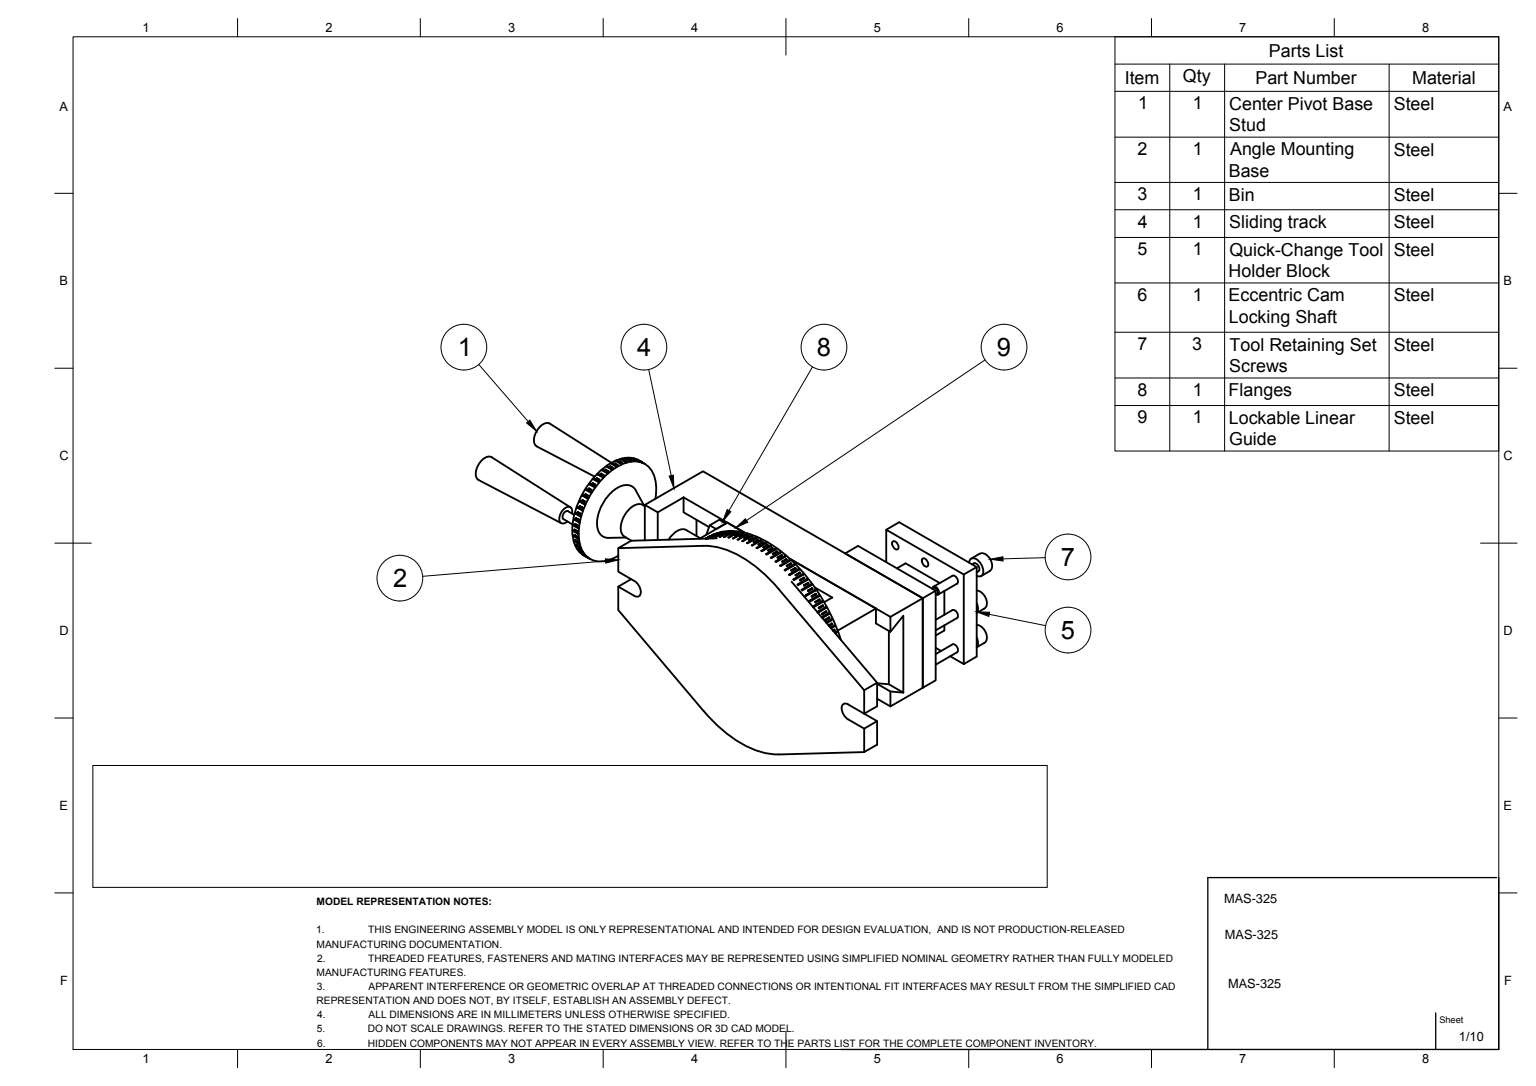
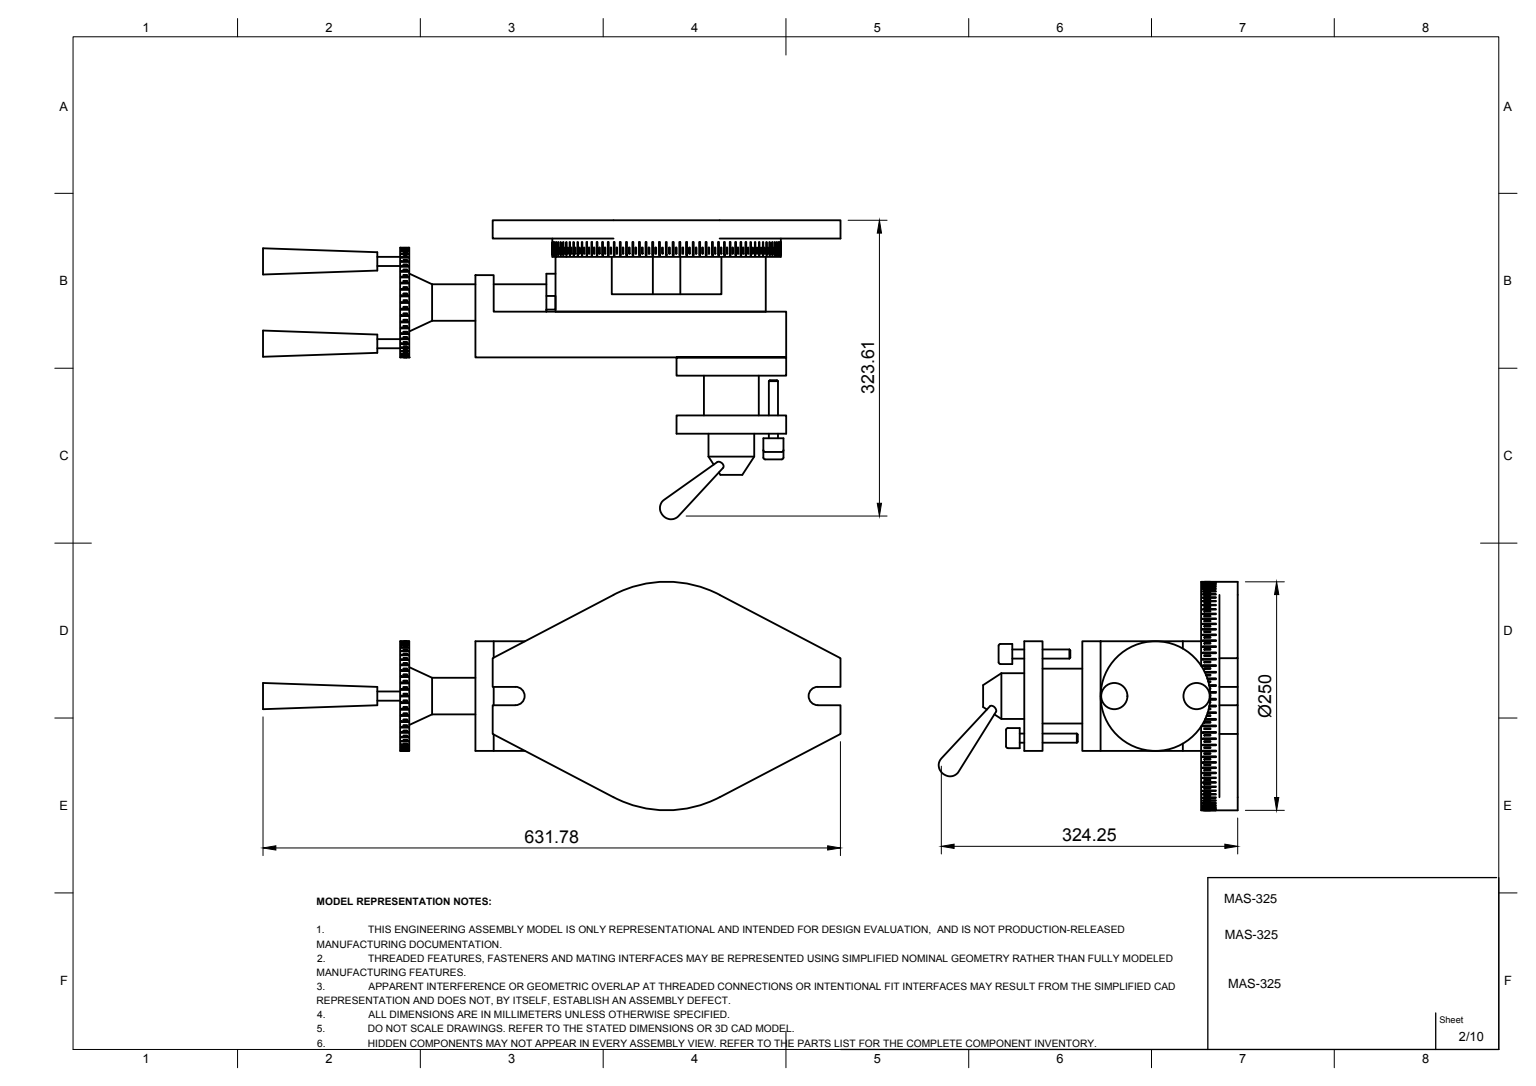
ISO-10303-21;
HEADER;
FILE_DESCRIPTION (('STEP AP214'),
    '1' );
FILE_NAME ('MAS-325',
    '2026-10-08T01:23:29',
    ( '' ),
    ( '' ),
    'SwSTEP 2.0',
    'SolidWorks 2025',
    '' );
FILE_SCHEMA (( 'AUTOMOTIVE_DESIGN' ));
ENDSEC;

DATA;
#1 = PLANE ( 'NONE',  #17713 ) ;
#2 = FACE_OUTER_BOUND ( 'NONE', #26944, .T. ) ;
#3 = VERTEX_POINT ( 'NONE', #17850 ) ;
#4 = VERTEX_POINT ( 'NONE', #2063 ) ;
#5 = EDGE_LOOP ( 'NONE', ( #45365, #39449, #49591, #6514 ) ) ;
#6 = EDGE_CURVE ( 'NONE', #30158, #26369, #45209, .T. ) ;
#7 = DIRECTION ( 'NONE',  ( 1.000000000000000000, -0.000000000000000000, -0.000000000000000000 ) ) ;
#8 = DIRECTION ( 'NONE',  ( 0.000000000000000000, 0.000000000000000000, -1.000000000000000000 ) ) ;
#9 = FACE_OUTER_BOUND ( 'NONE', #31225, .T. ) ;
#10 = ORIENTED_EDGE ( 'NONE', *, *, #44040, .F. ) ;
#11 = CARTESIAN_POINT ( 'NONE',  ( 2.729299751253404072, 51.29764658765966345, -20.73231253916988237 ) ) ;
#12 = ORIENTED_EDGE ( 'NONE', *, *, #51700, .T. ) ;
#13 = ORIENTED_EDGE ( 'NONE', *, *, #43268, .F. ) ;
#14 = ORIENTED_EDGE ( 'NONE', *, *, #20809, .T. ) ;
#15 = LINE ( 'NONE', #16057, #4072 ) ;
#16 = EDGE_CURVE ( 'NONE', #34125, #29247, #18107, .T. ) ;
#17 = ADVANCED_FACE ( 'NONE', ( #34134 ), #14181, .T. ) ;
#18 = ORIENTED_EDGE ( 'NONE', *, *, #15943, .T. ) ;
#19 = AXIS2_PLACEMENT_3D ( 'NONE', #21420, #9597, #9087 ) ;
#20 = AXIS2_PLACEMENT_3D ( 'NONE', #37352, #1353, #33432 ) ;
#21 = EDGE_CURVE ( 'NONE', #1891, #35017, #9977, .T. ) ;
#22 = CARTESIAN_POINT ( 'NONE',  ( -159.8192355313504720, -177.1207230881787780, -56.81883646197830018 ) ) ;
#23 = DIRECTION ( 'NONE',  ( -0.000000000000000000, 1.000000000000000000, -0.000000000000000000 ) ) ;
#26 = ORIENTED_EDGE ( 'NONE', *, *, #11216, .F. ) ;
#25 = CARTESIAN_POINT ( 'NONE',  ( -336.3521761649654422, -170.5607375887735770, 35.68215131113770155 ) ) ;
#24 = CARTESIAN_POINT ( 'NONE',  ( -0.3054481938615447034, -177.1207230881787780, 115.3442529744090592 ) ) ;
#27 = DIRECTION ( 'NONE',  ( -0.000000000000000000, 1.000000000000000000, -0.000000000000000000 ) ) ;
#28 = EDGE_LOOP ( 'NONE', ( #8074, #9559, #4118, #19918 ) ) ;
#29 = DIRECTION ( 'NONE',  ( 0.000000000000000000, -0.3546048870425363986, -0.9350162426854146114 ) ) ;
#30 = ORIENTED_EDGE ( 'NONE', *, *, #16889, .F. ) ;
#31 = CARTESIAN_POINT ( 'NONE',  ( -339.1964088526558498, -131.1080185721124849, 58.50955523165764305 ) ) ;
#32 = LINE ( 'NONE', #15292, #22958 ) ;
#34 = CARTESIAN_POINT ( 'NONE',  ( 15.29189835570547551, -175.3837268820161057, 106.3450133598704213 ) ) ;
#33 = CARTESIAN_POINT ( 'NONE',  ( -56.05401443572774411, -175.3837268820161057, 124.7702732086912931 ) ) ;
#35 = VERTEX_POINT ( 'NONE', #9196 ) ;
#36 = DIRECTION ( 'NONE',  ( -1.000000000000000000, -0.000000000000000000, -0.000000000000000000 ) ) ;
#37 = FACE_OUTER_BOUND ( 'NONE', #25266, .T. ) ;
#39 = AXIS2_PLACEMENT_3D ( 'NONE', #35953, #36729, #8094 ) ;
#38 =( NAMED_UNIT ( * ) PLANE_ANGLE_UNIT ( ) SI_UNIT ( $, .RADIAN. ) );
#40 = ORIENTED_EDGE ( 'NONE', *, *, #10845, .T. ) ;
#41 = EDGE_CURVE ( 'NONE', #38866, #36143, #5787, .T. ) ;
#42 = DIRECTION ( 'NONE',  ( -0.000000000000000000, 1.000000000000000000, -0.000000000000000000 ) ) ;
#43 = LINE ( 'NONE', #8442, #5592 ) ;
#44 = DIRECTION ( 'NONE',  ( -0.8455960035018311727, 0.000000000000000000, 0.5338233779647826305 ) ) ;
#45 = ORIENTED_EDGE ( 'NONE', *, *, #35189, .T. ) ;
#46 = CARTESIAN_POINT ( 'NONE',  ( 63.31225588004632243, -183.6283474603465606, 55.92572546981597981 ) ) ;
#47 = FACE_OUTER_BOUND ( 'NONE', #8464, .T. ) ;
#48 = EDGE_CURVE ( 'NONE', #19235, #10210, #19545, .T. ) ;
#49 = ORIENTED_EDGE ( 'NONE', *, *, #34843, .T. ) ;
#50 = DIRECTION ( 'NONE',  ( -0.4031234292879665171, 0.000000000000000000, -0.9151456172430210145 ) ) ;
#51 = ORIENTED_EDGE ( 'NONE', *, *, #6223, .F. ) ;
#52 = DIRECTION ( 'NONE',  ( 0.000000000000000000, 1.341519488088730767E-14, -1.000000000000000000 ) ) ;
#53 = CARTESIAN_POINT ( 'NONE',  ( -47.55243714407702527, -193.5000000000000000, 0.3758275821142491591 ) ) ;
#54 = AXIS2_PLACEMENT_3D ( 'NONE', #38179, #2187, #21657 ) ;
#55 = CARTESIAN_POINT ( 'NONE',  ( -332.3517673607765914, -139.2044816956407089, -56.89493493766761389 ) ) ;
#56 = CARTESIAN_POINT ( 'NONE',  ( 74.95461934957533856, -175.3837268820161057, -11.83705339977243121 ) ) ;
#57 = PLANE ( 'NONE',  #3915 ) ;
#58 = CIRCLE ( 'NONE', #10119, 125.0000000000000000 ) ;
#59 = CARTESIAN_POINT ( 'NONE',  ( -336.3521761649654422, -123.5000000000000284, 0.000000000000000000 ) ) ;
#60 = CARTESIAN_POINT ( 'NONE',  ( -330.4913330509368166, -178.8432607619606358, 20.45418021416736565 ) ) ;
#61 = LINE ( 'NONE', #8461, #49088 ) ;
#63 = ORIENTED_EDGE ( 'NONE', *, *, #44474, .F. ) ;
#62 = CARTESIAN_POINT ( 'NONE',  ( -135.4449840867448813, -193.5000000000000000, -88.39086586114740385 ) ) ;
#64 = ORIENTED_EDGE ( 'NONE', *, *, #9737, .T. ) ;
#65 = CARTESIAN_POINT ( 'NONE',  ( -339.1964088526558498, -175.5095439275173135, 27.86139516340941213 ) ) ;
#66 = CARTESIAN_POINT ( 'NONE',  ( -332.3517673607765914, -91.61526299123897843, -50.82679948493848343 ) ) ;
#67 = ORIENTED_EDGE ( 'NONE', *, *, #21766, .T. ) ;
#68 = ORIENTED_EDGE ( 'NONE', *, *, #41329, .T. ) ;
#69 = VECTOR ( 'NONE', #22524, 1000.000000000000000 ) ;
#70 = ORIENTED_EDGE ( 'NONE', *, *, #36153, .T. ) ;
#71 = CARTESIAN_POINT ( 'NONE',  ( 74.13662511985246795, -189.7472609257535510, 18.47640724094593523 ) ) ;
#72 = DIRECTION ( 'NONE',  ( 0.000000000000000000, 0.000000000000000000, 1.000000000000000000 ) ) ;
#73 = EDGE_CURVE ( 'NONE', #1427, #18230, #29600, .T. ) ;
#74 = CARTESIAN_POINT ( 'NONE',  ( -52.47502265695594303, -183.6283474603465606, -124.9361149384469627 ) ) ;
#75 = DIRECTION ( 'NONE',  ( 0.000000000000000000, -0.000000000000000000, 1.000000000000000000 ) ) ;
#76 = VERTEX_POINT ( 'NONE', #10211 ) ;
#77 = VERTEX_POINT ( 'NONE', #49406 ) ;
#78 = ORIENTED_EDGE ( 'NONE', *, *, #31301, .F. ) ;
#79 = DIRECTION ( 'NONE',  ( -0.000000000000000000, 1.000000000000000000, -0.000000000000000000 ) ) ;
#80 = DIRECTION ( 'NONE',  ( 0.6749830015182038956, 0.000000000000000000, 0.7378332790417333475 ) ) ;
#81 = CARTESIAN_POINT ( 'NONE',  ( -330.4913330509368166, -183.4979166304964622, -0.4999999999999551470 ) ) ;
#82 = LINE ( 'NONE', #16386, #13659 ) ;
#83 = FACE_OUTER_BOUND ( 'NONE', #49301, .T. ) ;
#84 = ORIENTED_EDGE ( 'NONE', *, *, #48754, .F. ) ;
#85 = DIRECTION ( 'NONE',  ( -0.000000000000000000, 1.000000000000000000, -0.000000000000000000 ) ) ;
#86 = AXIS2_PLACEMENT_3D ( 'NONE', #8984, #303, #32633 ) ;
#87 = LINE ( 'NONE', #8748, #33300 ) ;
#88 = CARTESIAN_POINT ( 'NONE',  ( -29.73468717939733708, -193.5000000000000000, 123.5865930638410930 ) ) ;
#89 = DIRECTION ( 'NONE',  ( -0.2059786187411094538, 0.000000000000000000, 0.9785564922995017012 ) ) ;
#90 = ORIENTED_EDGE ( 'NONE', *, *, #2858, .T. ) ;
#91 = ORIENTED_EDGE ( 'NONE', *, *, #37914, .F. ) ;
#92 = ORIENTED_EDGE ( 'NONE', *, *, #9964, .T. ) ;
#93 = CARTESIAN_POINT ( 'NONE',  ( -171.9740864388383557, -189.7472609257535510, -11.18012358327903577 ) ) ;
#94 = DIRECTION ( 'NONE',  ( -0.8757349421956412971, 0.000000000000000000, 0.4827922027307366970 ) ) ;
#95 = ORIENTED_EDGE ( 'NONE', *, *, #42836, .F. ) ;
#96 = EDGE_CURVE ( 'NONE', #8568, #51994, #49908, .T. ) ;
#97 = LINE ( 'NONE', #16919, #528 ) ;
#98 = DIRECTION ( 'NONE',  ( -0.9982437317643214625, 0.000000000000000000, -0.05924062789371441901 ) ) ;
#99 = CARTESIAN_POINT ( 'NONE',  ( 141.7825277784304205, -193.5000000000000000, -9.999999999999987566 ) ) ;
#100 = ORIENTED_EDGE ( 'NONE', *, *, #32040, .F. ) ;
#101 = LINE ( 'NONE', #40291, #9133 ) ;
#102 = ORIENTED_EDGE ( 'NONE', *, *, #46111, .F. ) ;
#103 = CARTESIAN_POINT ( 'NONE',  ( -336.3521761649654422, -123.5000000000000284, 0.000000000000000000 ) ) ;
#104 = ORIENTED_EDGE ( 'NONE', *, *, #44978, .T. ) ;
#105 = LINE ( 'NONE', #39778, #22073 ) ;
#106 = FACE_BOUND ( 'NONE', #42826, .T. ) ;
#107 = VECTOR ( 'NONE', #36864, 1000.000000000000000 ) ;
#108 = DIRECTION ( 'NONE',  ( -0.1768902751225802927, 0.000000000000000000, 0.9842305779475953864 ) ) ;
#109 = ORIENTED_EDGE ( 'NONE', *, *, #36766, .T. ) ;
#110 = DIRECTION ( 'NONE',  ( 1.000000000000000000, -0.000000000000000000, -0.000000000000000000 ) ) ;
#111 = DIRECTION ( 'NONE',  ( 0.9785564922995032555, 0.000000000000000000, 0.2059786187411021818 ) ) ;
#112 = DIRECTION ( 'NONE',  ( 0.000000000000000000, -1.000000000000000000, 0.000000000000000000 ) ) ;
#113 = EDGE_CURVE ( 'NONE', #39629, #40896, #21795, .T. ) ;
#114 = CARTESIAN_POINT ( 'NONE',  ( -339.1964088526558498, -122.9999999999993747, 59.00000000000002132 ) ) ;
#115 = EDGE_LOOP ( 'NONE', ( #6615, #26573, #34341, #46200 ) ) ;
#116 = CARTESIAN_POINT ( 'NONE',  ( -162.3451783319732726, -183.6283474603465606, 51.57055649762781968 ) ) ;
#117 = VERTEX_POINT ( 'NONE', #22299 ) ;
#118 = EDGE_LOOP ( 'NONE', ( #5505, #7567, #35660, #29019 ) ) ;
#119 = CARTESIAN_POINT ( 'NONE',  ( -47.97059563285962724, -189.7472609257535510, -0.8610436117673480050 ) ) ;
#121 = VERTEX_POINT ( 'NONE', #29930 ) ;
#120 = DIRECTION ( 'NONE',  ( 0.000000000000000000, 0.000000000000000000, -1.000000000000000000 ) ) ;
#122 = VECTOR ( 'NONE', #5953, 1000.000000000000000 ) ;
#123 = ORIENTED_EDGE ( 'NONE', *, *, #8914, .F. ) ;
#124 = CARTESIAN_POINT ( 'NONE',  ( 76.04209377433248562, -193.5000000000000000, -10.93003379476866677 ) ) ;
#125 = CIRCLE ( 'NONE', #14436, 125.0000000000000000 ) ;
#126 = AXIS2_PLACEMENT_3D ( 'NONE', #20035, #19509, #35530 ) ;
#127 = EDGE_CURVE ( 'NONE', #48981, #10059, #6022, .T. ) ;
#128 = CARTESIAN_POINT ( 'NONE',  ( 23.33927677392131628, -183.6283474603465606, -102.3089288139528747 ) ) ;
#129 = EDGE_LOOP ( 'NONE', ( #1022, #18617, #38243, #43508 ) ) ;
#130 = FACE_OUTER_BOUND ( 'NONE', #50584, .T. ) ;
#131 = FACE_OUTER_BOUND ( 'NONE', #2320, .T. ) ;
#132 = EDGE_LOOP ( 'NONE', ( #26426, #7526, #45933, #33902, #50296, #18073, #41197, #48921 ) ) ;
#133 = LINE ( 'NONE', #35615, #5709 ) ;
#134 = DIRECTION ( 'NONE',  ( 0.000000000000000000, 0.000000000000000000, -1.000000000000000000 ) ) ;
#135 = ADVANCED_FACE ( 'NONE', ( #33613 ), #26232, .F. ) ;
#136 = LINE ( 'NONE', #12733, #6804 ) ;
#137 = CARTESIAN_POINT ( 'NONE',  ( -180.0000000000000568, -123.5000000000000284, 6.938893903907228378E-15 ) ) ;
#138 = VERTEX_POINT ( 'NONE', #51213 ) ;
#139 = EDGE_LOOP ( 'NONE', ( #49981, #10287, #23201, #19361 ) ) ;
#140 = EDGE_CURVE ( 'NONE', #35696, #40857, #2842, .T. ) ;
#141 = EDGE_LOOP ( 'NONE', ( #33716, #13532, #31496, #14076 ) ) ;
#142 = FACE_OUTER_BOUND ( 'NONE', #28523, .T. ) ;
#143 = FACE_OUTER_BOUND ( 'NONE', #34738, .T. ) ;
#144 = ADVANCED_FACE ( 'NONE', ( #30434 ), #14678, .T. ) ;
#145 = AXIS2_PLACEMENT_3D ( 'NONE', #44882, #32531, #8363 ) ;
#146 = DIRECTION ( 'NONE',  ( 0.000000000000000000, 0.000000000000000000, 1.000000000000000000 ) ) ;
#147 = FACE_BOUND ( 'NONE', #3566, .T. ) ;
#148 = CARTESIAN_POINT ( 'NONE',  ( -49.42645310536303782, -193.5000000000000000, -0.3202698538628417357 ) ) ;
#149 = EDGE_LOOP ( 'NONE', ( #37158, #34749, #12622, #8315 ) ) ;
#150 = VERTEX_POINT ( 'NONE', #38840 ) ;
#152 = ORIENTED_EDGE ( 'NONE', *, *, #45435, .F. ) ;
#151 = DIRECTION ( 'NONE',  ( 0.000000000000000000, -0.000000000000000000, 1.000000000000000000 ) ) ;
#153 = VERTEX_POINT ( 'NONE', #46748 ) ;
#154 = CARTESIAN_POINT ( 'NONE',  ( -332.3517673607765914, -153.2494431741581025, -51.01861988938816950 ) ) ;
#155 = EDGE_CURVE ( 'NONE', #5943, #22832, #22063, .T. ) ;
#156 = DIRECTION ( 'NONE',  ( -1.000000000000000000, 0.000000000000000000, 0.000000000000000000 ) ) ;
#157 = VECTOR ( 'NONE', #9488, 1000.000000000000000 ) ;
#158 = DIRECTION ( 'NONE',  ( 0.000000000000000000, 0.000000000000000000, 1.000000000000000000 ) ) ;
#159 = CARTESIAN_POINT ( 'NONE',  ( -84.53143451966467126, -175.3837268820161057, -118.6432945265036807 ) ) ;
#160 = ORIENTED_EDGE ( 'NONE', *, *, #6029, .T. ) ;
#161 = LINE ( 'NONE', #28016, #26684 ) ;
#162 = AXIS2_PLACEMENT_3D ( 'NONE', #7997, #20089, #36113 ) ;
#163 = ORIENTED_EDGE ( 'NONE', *, *, #20136, .T. ) ;
#164 = AXIS2_PLACEMENT_3D ( 'NONE', #24435, #20760, #36510 ) ;
#165 = ORIENTED_EDGE ( 'NONE', *, *, #4140, .T. ) ;
#166 = DIRECTION ( 'NONE',  ( 0.000000000000000000, -0.000000000000000000, 1.000000000000000000 ) ) ;
#167 = CARTESIAN_POINT ( 'NONE',  ( -139.0630283577175987, -193.5000000000000000, -86.13684908212448477 ) ) ;
#168 = CARTESIAN_POINT ( 'NONE',  ( -15.24927435600541692, -177.1207230881787780, 120.5021863277719234 ) ) ;
#169 = CARTESIAN_POINT ( 'NONE',  ( -336.3521761649654422, -161.4024510877913485, 45.24454186338643780 ) ) ;
#170 = CARTESIAN_POINT ( 'NONE',  ( -144.0067397530739299, -183.6283474603465606, -80.61932246194588458 ) ) ;
#171 = CARTESIAN_POINT ( 'NONE',  ( -41.24387117724851493, -189.7472609257535510, 124.7904286264581231 ) ) ;
#172 = VERTEX_POINT ( 'NONE', #26760 ) ;
#173 = DIRECTION ( 'NONE',  ( -0.8896570909947467687, 0.000000000000000000, -0.4566292373937140270 ) ) ;
#174 = CARTESIAN_POINT ( 'NONE',  ( -134.9734323446613473, -175.3837268820161057, 88.85232316304892208 ) ) ;
#175 = CIRCLE ( 'NONE', #31206, 125.0000000000000000 ) ;
#176 = FACE_BOUND ( 'NONE', #45465, .T. ) ;
#177 = VERTEX_POINT ( 'NONE', #42529 ) ;
#178 = AXIS2_PLACEMENT_3D ( 'NONE', #15666, #4339, #31680 ) ;
#179 = CIRCLE ( 'NONE', #49719, 4.000000000000003553 ) ;
#180 = DIRECTION ( 'NONE',  ( -0.000000000000000000, 1.000000000000000000, -0.000000000000000000 ) ) ;
#181 = FACE_OUTER_BOUND ( 'NONE', #6191, .T. ) ;
#182 = EDGE_CURVE ( 'NONE', #39742, #38924, #15463, .T. ) ;
#183 = ORIENTED_EDGE ( 'NONE', *, *, #47786, .F. ) ;
#184 = ADVANCED_FACE ( 'NONE', ( #15201 ), #27530, .F. ) ;
#185 = DIRECTION ( 'NONE',  ( 0.4827922027307366970, 0.000000000000000000, 0.8757349421956412971 ) ) ;
#186 = VERTEX_POINT ( 'NONE', #51463 ) ;
#187 = CARTESIAN_POINT ( 'NONE',  ( -148.0127667507368585, -183.6283474603465606, -75.61781872352626976 ) ) ;
#188 = CARTESIAN_POINT ( 'NONE',  ( -48.47912675150885065, -193.5000000000000000, 6.938893903907228378E-15 ) ) ;
#190 = EDGE_LOOP ( 'NONE', ( #41506, #8467, #35219, #32996 ) ) ;
#189 = DIRECTION ( 'NONE',  ( 0.000000000000000000, 0.000000000000000000, 1.000000000000000000 ) ) ;
#191 = AXIS2_PLACEMENT_3D ( 'NONE', #6779, #42505, #19123 ) ;
#192 = ADVANCED_FACE ( 'NONE', ( #46484 ), #50954, .F. ) ;
#193 = FACE_OUTER_BOUND ( 'NONE', #27346, .T. ) ;
#194 = VERTEX_POINT ( 'NONE', #14955 ) ;
#195 = EDGE_CURVE ( 'NONE', #34486, #40282, #15361, .T. ) ;
#196 = AXIS2_PLACEMENT_3D ( 'NONE', #12070, #3180, #43634 ) ;
#197 = ORIENTED_EDGE ( 'NONE', *, *, #15389, .T. ) ;
#198 = ADVANCED_FACE ( 'NONE', ( #19392 ), #26495, .F. ) ;
#199 = EDGE_LOOP ( 'NONE', ( #48171, #38497, #32246, #32492 ) ) ;
#200 = DIRECTION ( 'NONE',  ( 0.000000000000000000, 0.2393156642875615969, 0.9709418174260511236 ) ) ;
#201 = CARTESIAN_POINT ( 'NONE',  ( -339.1964088526558498, -180.9052250602809977, -13.63415328425247885 ) ) ;
#202 = EDGE_CURVE ( 'NONE', #8838, #28521, #30963, .T. ) ;
#203 = AXIS2_PLACEMENT_3D ( 'NONE', #1568, #37299, #37818 ) ;
#204 = AXIS2_PLACEMENT_3D ( 'NONE', #4568, #29258, #44511 ) ;
#205 = CARTESIAN_POINT ( 'NONE',  ( -157.8637630444124795, -175.3837268820161057, -60.49794494914009135 ) ) ;
#206 = CARTESIAN_POINT ( 'NONE',  ( -332.3517673607765914, -86.34605966037949543, -45.90766452162698386 ) ) ;
#207 = ORIENTED_EDGE ( 'NONE', *, *, #866, .T. ) ;
#210 = VERTEX_POINT ( 'NONE', #34890 ) ;
#209 = DIRECTION ( 'NONE',  ( 0.000000000000000000, 0.000000000000000000, 1.000000000000000000 ) ) ;
#208 = DIRECTION ( 'NONE',  ( 0.000000000000000000, 0.000000000000000000, 1.000000000000000000 ) ) ;
#211 = AXIS2_PLACEMENT_3D ( 'NONE', #44344, #36428, #28543 ) ;
#212 = AXIS2_PLACEMENT_3D ( 'NONE', #15523, #6858, #2909 ) ;
#213 = EDGE_LOOP ( 'NONE', ( #16091, #33158, #8108, #2239 ) ) ;
#214 = CARTESIAN_POINT ( 'NONE',  ( -339.1964088526558498, -157.4273119900853146, -48.27201571435997352 ) ) ;
#215 = ORIENTED_EDGE ( 'NONE', *, *, #9578, .T. ) ;
#216 = CARTESIAN_POINT ( 'NONE',  ( -339.1964088526558498, -83.33976666098951114, 44.57752413667933666 ) ) ;
#217 = ORIENTED_EDGE ( 'NONE', *, *, #6337, .T. ) ;
#218 = VECTOR ( 'NONE', #39857, 1000.000000000000227 ) ;
#219 = DIRECTION ( 'NONE',  ( 0.000000000000000000, 1.000000000000000000, 0.000000000000000000 ) ) ;
#220 = ORIENTED_EDGE ( 'NONE', *, *, #16410, .F. ) ;
#222 = DIRECTION ( 'NONE',  ( -0.000000000000000000, 0.2393156642875685636, 0.9709418174260492362 ) ) ;
#221 = CARTESIAN_POINT ( 'NONE',  ( 0.000000000000000000, 103.6102204319011832, -100.2584055548201292 ) ) ;
#223 = ORIENTED_EDGE ( 'NONE', *, *, #649, .T. ) ;
#224 = ORIENTED_EDGE ( 'NONE', *, *, #48940, .F. ) ;
#225 = FACE_OUTER_BOUND ( 'NONE', #49522, .T. ) ;
#226 = DIRECTION ( 'NONE',  ( -0.9890401873221633666, 0.000000000000000000, -0.1476465640024850756 ) ) ;
#227 = FACE_OUTER_BOUND ( 'NONE', #2223, .T. ) ;
#228 = DIRECTION ( 'NONE',  ( 0.000000000000000000, 0.000000000000000000, 1.000000000000000000 ) ) ;
#229 = FACE_OUTER_BOUND ( 'NONE', #4833, .T. ) ;
#230 = CIRCLE ( 'NONE', #6149, 125.0000000000000000 ) ;
#231 = DIRECTION ( 'NONE',  ( -0.000000000000000000, 1.000000000000000000, -0.000000000000000000 ) ) ;
#232 = VERTEX_POINT ( 'NONE', #18624 ) ;
#233 = FACE_OUTER_BOUND ( 'NONE', #34259, .T. ) ;
#234 = CARTESIAN_POINT ( 'NONE',  ( -47.82630463331833681, -177.1207230881787780, 0.7575112421616305713 ) ) ;
#235 = AXIS2_PLACEMENT_3D ( 'NONE', #29797, #45849, #41895 ) ;
#236 = ADVANCED_FACE ( 'NONE', ( #38589 ), #47005, .T. ) ;
#237 = CARTESIAN_POINT ( 'NONE',  ( -180.0000000000000568, -115.7896721143442278, 18.45401972188388839 ) ) ;
#238 = ORIENTED_EDGE ( 'NONE', *, *, #26470, .F. ) ;
#239 = CARTESIAN_POINT ( 'NONE',  ( 74.49773146996551532, -183.6283474603465606, -22.39848972532281834 ) ) ;
#240 = EDGE_CURVE ( 'NONE', #16530, #9197, #11238, .T. ) ;
#241 = FACE_OUTER_BOUND ( 'NONE', #10500, .T. ) ;
#242 = CYLINDRICAL_SURFACE ( 'NONE', #15746, 20.00000000000001066 ) ;
#243 = EDGE_CURVE ( 'NONE', #48355, #27011, #50682, .T. ) ;
#244 = ORIENTED_EDGE ( 'NONE', *, *, #45271, .T. ) ;
#245 = EDGE_CURVE ( 'NONE', #35901, #35187, #7056, .T. ) ;
#246 = VERTEX_POINT ( 'NONE', #50438 ) ;
#247 = CIRCLE ( 'NONE', #6976, 125.0000000000000000 ) ;
#248 = EDGE_LOOP ( 'NONE', ( #15059, #26707, #42311, #35212 ) ) ;
#249 = CIRCLE ( 'NONE', #45592, 125.0000000000000000 ) ;
#250 = EDGE_CURVE ( 'NONE', #5889, #26611, #27078, .T. ) ;
#251 = LINE ( 'NONE', #40705, #46952 ) ;
#252 = AXIS2_PLACEMENT_3D ( 'NONE', #33154, #25277, #24755 ) ;
#253 = ADVANCED_FACE ( 'NONE', ( #3105 ), #7314, .F. ) ;
#254 = CARTESIAN_POINT ( 'NONE',  ( 1.959434878635765131E-15, -63.50000000000000000, 16.00000000000000000 ) ) ;
#255 = CARTESIAN_POINT ( 'NONE',  ( -157.8637630444124795, -175.3837268820161057, -60.49794494914009846 ) ) ;
#256 = DIRECTION ( 'NONE',  ( -0.000000000000000000, 0.8229838658936556861, -0.5680647467311569221 ) ) ;
#257 = EDGE_LOOP ( 'NONE', ( #21171, #20586, #46600, #11240 ) ) ;
#258 = AXIS2_PLACEMENT_3D ( 'NONE', #32515, #48563, #24621 ) ;
#259 = EDGE_CURVE ( 'NONE', #47910, #27371, #721, .T. ) ;
#260 = CARTESIAN_POINT ( 'NONE',  ( -332.3517673607765914, -133.2247606357419443, -58.25253621232173629 ) ) ;
#261 = ORIENTED_EDGE ( 'NONE', *, *, #51004, .T. ) ;
#262 = EDGE_CURVE ( 'NONE', #7509, #26454, #12272, .T. ) ;
#263 = ORIENTED_EDGE ( 'NONE', *, *, #26885, .T. ) ;
#264 = EDGE_CURVE ( 'NONE', #15715, #30086, #23588, .T. ) ;
#265 = VERTEX_POINT ( 'NONE', #44078 ) ;
#266 = CARTESIAN_POINT ( 'NONE',  ( -111.6834028793037987, -175.3837268820161057, 106.6827995071088253 ) ) ;
#267 = VECTOR ( 'NONE', #9756, 1000.000000000000000 ) ;
#268 = EDGE_CURVE ( 'NONE', #19322, #4539, #40375, .T. ) ;
#269 = ORIENTED_EDGE ( 'NONE', *, *, #12211, .F. ) ;
#270 = ADVANCED_FACE ( 'NONE', ( #39602 ), #440, .T. ) ;
#271 = AXIS2_PLACEMENT_3D ( 'NONE', #37551, #38049, #18093 ) ;
#272 = CARTESIAN_POINT ( 'NONE',  ( -102.9981419485577732, -193.5000000000000000, -111.3726929437936377 ) ) ;
#273 = LINE ( 'NONE', #29176, #44951 ) ;
#276 = ORIENTED_EDGE ( 'NONE', *, *, #30764, .F. ) ;
#275 = DIRECTION ( 'NONE',  ( 0.000000000000000000, 0.000000000000000000, -1.000000000000000000 ) ) ;
#274 = DIRECTION ( 'NONE',  ( -0.6300878435817094392, 0.000000000000000000, -0.7765238627180437447 ) ) ;
#277 = CARTESIAN_POINT ( 'NONE',  ( -108.4791267515088435, -173.5000000000000284, 60.00000000000002132 ) ) ;
#278 = ORIENTED_EDGE ( 'NONE', *, *, #14380, .F. ) ;
#279 = LINE ( 'NONE', #11844, #1238 ) ;
#280 = ORIENTED_EDGE ( 'NONE', *, *, #40635, .T. ) ;
#281 = DIRECTION ( 'NONE',  ( 0.000000000000000000, 0.000000000000000000, 1.000000000000000000 ) ) ;
#282 = CARTESIAN_POINT ( 'NONE',  ( -117.6201219941651601, -193.5000000000000000, 104.1370384486469902 ) ) ;
#284 = LINE ( 'NONE', #32615, #29005 ) ;
#283 = DIRECTION ( 'NONE',  ( 0.9785564922995060311, 0.000000000000000000, -0.2059786187410889424 ) ) ;
#285 = VECTOR ( 'NONE', #4558, 999.9999999999998863 ) ;
#286 = EDGE_CURVE ( 'NONE', #41564, #12706, #20162, .T. ) ;
#287 = EDGE_LOOP ( 'NONE', ( #13570, #29381, #45686, #19106 ) ) ;
#288 = CARTESIAN_POINT ( 'NONE',  ( -332.3517673607765914, -139.4384828369889249, -57.84431488793872944 ) ) ;
#289 = VECTOR ( 'NONE', #42767, 1000.000000000000000 ) ;
#290 = LINE ( 'NONE', #41018, #22829 ) ;
#291 =( NAMED_UNIT ( * ) SI_UNIT ( $, .STERADIAN. ) SOLID_ANGLE_UNIT ( ) );
#292 = ORIENTED_EDGE ( 'NONE', *, *, #4293, .T. ) ;
#293 = DIRECTION ( 'NONE',  ( -0.7378332790417285736, 0.000000000000000000, 0.6749830015182091136 ) ) ;
#294 = DIRECTION ( 'NONE',  ( 0.000000000000000000, 1.000000000000000000, 0.000000000000000000 ) ) ;
#295 = DIRECTION ( 'NONE',  ( -0.5315839928299663786, 0.000000000000000000, 0.8470055835512245723 ) ) ;
#296 = ORIENTED_EDGE ( 'NONE', *, *, #7021, .F. ) ;
#297 = PLANE ( 'NONE',  #12496 ) ;
#298 = CARTESIAN_POINT ( 'NONE',  ( -332.3517673607765914, -70.03480886230919111, 25.08789112700620194 ) ) ;
#299 = ORIENTED_EDGE ( 'NONE', *, *, #48513, .F. ) ;
#300 = DIRECTION ( 'NONE',  ( -0.000000000000000000, 1.000000000000000000, -0.000000000000000000 ) ) ;
#301 = ORIENTED_EDGE ( 'NONE', *, *, #17600, .T. ) ;
#302 = LINE ( 'NONE', #51846, #44972 ) ;
#303 = DIRECTION ( 'NONE',  ( 0.000000000000000000, -1.000000000000000000, -0.000000000000000000 ) ) ;
#304 = VECTOR ( 'NONE', #6008, 999.9999999999998863 ) ;
#305 = EDGE_CURVE ( 'NONE', #49014, #8114, #15730, .T. ) ;
#306 = CARTESIAN_POINT ( 'NONE',  ( -305.0000000000000568, -71.64707600775140861, -30.18731974611341684 ) ) ;
#307 = DIRECTION ( 'NONE',  ( 0.000000000000000000, 1.000000000000000000, 0.000000000000000000 ) ) ;
#308 = DIRECTION ( 'NONE',  ( -1.000000000000000000, 0.000000000000000000, 0.000000000000000000 ) ) ;
#309 = ADVANCED_FACE ( 'NONE', ( #15976 ), #8082, .T. ) ;
#310 = AXIS2_PLACEMENT_3D ( 'NONE', #50252, #42607, #38132 ) ;
#311 = EDGE_CURVE ( 'NONE', #37290, #775, #44603, .T. ) ;
#312 = DIRECTION ( 'NONE',  ( -0.000000000000000000, 1.000000000000000000, -0.000000000000000000 ) ) ;
#313 = EDGE_CURVE ( 'NONE', #8692, #47336, #37219, .T. ) ;
#314 = CARTESIAN_POINT ( 'NONE',  ( 60.00000000000000000, -113.5000000000000000, 60.00000000000000711 ) ) ;
#315 = LINE ( 'NONE', #15321, #378 ) ;
#317 = EDGE_LOOP ( 'NONE', ( #32171, #36986, #20388, #10523 ) ) ;
#316 = CARTESIAN_POINT ( 'NONE',  ( -330.4913330509368166, -109.8658467157472813, -57.40522506028090532 ) ) ;
#318 = EDGE_LOOP ( 'NONE', ( #38235, #13867, #475, #2486 ) ) ;
#319 = CARTESIAN_POINT ( 'NONE',  ( 52.36832552120769435, -189.7472609257535510, -72.15117186584490128 ) ) ;
#320 = CARTESIAN_POINT ( 'NONE',  ( -41.24387117724851493, -189.7472609257535510, 124.7904286264581231 ) ) ;
#321 = EDGE_LOOP ( 'NONE', ( #34166, #26853, #15993, #21976 ) ) ;
#322 = EDGE_LOOP ( 'NONE', ( #10542, #48454, #37812, #15490 ) ) ;
#323 = EDGE_CURVE ( 'NONE', #36975, #28008, #47779, .T. ) ;
#324 = ORIENTED_EDGE ( 'NONE', *, *, #11588, .T. ) ;
#325 = DIRECTION ( 'NONE',  ( 0.000000000000000000, 0.2393156642875516049, -0.9709418174260534551 ) ) ;
#326 = DIRECTION ( 'NONE',  ( 0.000000000000000000, 0.000000000000000000, 1.000000000000000000 ) ) ;
#327 = CARTESIAN_POINT ( 'NONE',  ( -66.64622755927948106, -193.5000000000000000, 123.6727797384707515 ) ) ;
#328 = ORIENTED_EDGE ( 'NONE', *, *, #49475, .F. ) ;
#329 = ORIENTED_EDGE ( 'NONE', *, *, #42921, .T. ) ;
#330 = EDGE_CURVE ( 'NONE', #27930, #47785, #15401, .T. ) ;
#331 = ORIENTED_EDGE ( 'NONE', *, *, #18307, .T. ) ;
#332 = DIRECTION ( 'NONE',  ( 0.000000000000000000, 0.000000000000000000, -1.000000000000000000 ) ) ;
#333 = CARTESIAN_POINT ( 'NONE',  ( -330.4913330509368166, -75.22798428563987727, -33.92731199008506593 ) ) ;
#335 = EDGE_LOOP ( 'NONE', ( #354, #13466, #39178, #31091 ) ) ;
#334 = DIRECTION ( 'NONE',  ( 0.000000000000000000, -1.000000000000000000, 0.000000000000000000 ) ) ;
#336 = CARTESIAN_POINT ( 'NONE',  ( -170.0000000000000284, -123.5000000000000284, 41.63467731922665394 ) ) ;
#337 = CARTESIAN_POINT ( 'NONE',  ( -84.19171550243321178, -175.3837268820161057, 119.7898618611247485 ) ) ;
#338 = VECTOR ( 'NONE', #11663, 1000.000000000000000 ) ;
#339 = ORIENTED_EDGE ( 'NONE', *, *, #31396, .F. ) ;
#340 = CARTESIAN_POINT ( 'NONE',  ( -339.1964088526558498, -137.1341532842523065, 57.40522506028101901 ) ) ;
#341 = VECTOR ( 'NONE', #5496, 1000.000000000000000 ) ;
#342 = DIRECTION ( 'NONE',  ( 0.000000000000000000, 0.000000000000000000, -1.000000000000000000 ) ) ;
#343 = CARTESIAN_POINT ( 'NONE',  ( -332.3517673607765914, -126.1322888500942270, -59.00000000000001421 ) ) ;
#344 = DIRECTION ( 'NONE',  ( -1.000000000000000000, 0.000000000000000000, 0.000000000000000000 ) ) ;
#345 = VECTOR ( 'NONE', #6207, 1000.000000000000000 ) ;
#346 = VERTEX_POINT ( 'NONE', #3887 ) ;
#347 = ORIENTED_EDGE ( 'NONE', *, *, #7630, .T. ) ;
#348 = EDGE_LOOP ( 'NONE', ( #40499, #34840, #43093, #48028 ) ) ;
#349 = CARTESIAN_POINT ( 'NONE',  ( -180.0000000000000568, -130.6726371812771959, -60.00000000000000711 ) ) ;
#350 = CARTESIAN_POINT ( 'NONE',  ( -332.3517673607765914, -65.24746378767824240, -9.724760635741734660 ) ) ;
#351 = ORIENTED_EDGE ( 'NONE', *, *, #10876, .T. ) ;
#352 = DIRECTION ( 'NONE',  ( 0.000000000000000000, 0.000000000000000000, 1.000000000000000000 ) ) ;
#353 = CARTESIAN_POINT ( 'NONE',  ( -332.3517673607765914, -135.2893155068536828, 58.83036664750491695 ) ) ;
#354 = ORIENTED_EDGE ( 'NONE', *, *, #40714, .F. ) ;
#355 = CARTESIAN_POINT ( 'NONE',  ( -59.28786813212836648, -183.6283474603465606, 124.5318076226587465 ) ) ;
#356 = VECTOR ( 'NONE', #3324, 1000.000000000000000 ) ;
#357 = CARTESIAN_POINT ( 'NONE',  ( 27.50603775690333563, -175.3837268820161057, -99.25348746834811209 ) ) ;
#358 = ORIENTED_EDGE ( 'NONE', *, *, #16677, .F. ) ;
#359 = DIRECTION ( 'NONE',  ( 1.000000000000000000, -0.000000000000000000, -0.000000000000000000 ) ) ;
#360 = ORIENTED_EDGE ( 'NONE', *, *, #30567, .T. ) ;
#361 = FACE_BOUND ( 'NONE', #24793, .T. ) ;
#362 = DIRECTION ( 'NONE',  ( 0.000000000000000000, -1.000000000000000000, 0.000000000000000000 ) ) ;
#363 = ORIENTED_EDGE ( 'NONE', *, *, #47489, .F. ) ;
#364 = DIRECTION ( 'NONE',  ( -0.000000000000000000, -0.9350162426854132791, 0.3546048870425396182 ) ) ;
#365 = CARTESIAN_POINT ( 'NONE',  ( -330.4913330509368166, -145.2430625708875880, -55.92172413327818958 ) ) ;
#366 = DIRECTION ( 'NONE',  ( -8.718379230999707126E-17, 0.7485107481711024136, 0.6631226582407937498 ) ) ;
#367 = ADVANCED_FACE ( 'NONE', ( #12542 ), #28557, .F. ) ;
#368 = EDGE_CURVE ( 'NONE', #39057, #30451, #5316, .T. ) ;
#369 = LINE ( 'NONE', #36375, #20714 ) ;
#370 = ORIENTED_EDGE ( 'NONE', *, *, #34030, .F. ) ;
#371 = CARTESIAN_POINT ( 'NONE',  ( -336.3521761649654422, -135.0638248728647852, 57.91551518289418254 ) ) ;
#372 = EDGE_LOOP ( 'NONE', ( #12308, #32950, #15983, #21673 ) ) ;
#373 = ORIENTED_EDGE ( 'NONE', *, *, #33329, .T. ) ;
#374 = DIRECTION ( 'NONE',  ( 0.000000000000000000, 0.7485107481711000821, -0.6631226582407965253 ) ) ;
#376 = ORIENTED_EDGE ( 'NONE', *, *, #30512, .F. ) ;
#375 = DIRECTION ( 'NONE',  ( -0.000000000000000000, 1.000000000000000000, -0.000000000000000000 ) ) ;
#377 = CIRCLE ( 'NONE', #16331, 125.0000000000000000 ) ;
#378 = VECTOR ( 'NONE', #32371, 1000.000000000000114 ) ;
#379 = EDGE_LOOP ( 'NONE', ( #7863, #48040, #19439, #9554 ) ) ;
#380 = CARTESIAN_POINT ( 'NONE',  ( 67.66641500972446011, -193.5000000000000000, 46.20836643931067300 ) ) ;
#381 = AXIS2_PLACEMENT_3D ( 'NONE', #38755, #31139, #39013 ) ;
#382 = CARTESIAN_POINT ( 'NONE',  ( 67.29303306501927295, -175.3837268820161057, 47.13604789772129777 ) ) ;
#383 = EDGE_LOOP ( 'NONE', ( #92, #27260, #27029, #39388 ) ) ;
#384 = LINE ( 'NONE', #24315, #19709 ) ;
#385 = EDGE_CURVE ( 'NONE', #3976, #38174, #2777, .T. ) ;
#386 = ORIENTED_EDGE ( 'NONE', *, *, #9915, .F. ) ;
#387 = CARTESIAN_POINT ( 'NONE',  ( -339.1964088526558498, -123.5000000000000284, 0.000000000000000000 ) ) ;
#388 = PLANE ( 'NONE',  #37573 ) ;
#390 = AXIS2_PLACEMENT_3D ( 'NONE', #5869, #10563, #18713 ) ;
#389 = DIRECTION ( 'NONE',  ( -0.4566292373937018145, 0.000000000000000000, -0.8896570909947529859 ) ) ;
#391 = LINE ( 'NONE', #24573, #45885 ) ;
#392 = ORIENTED_EDGE ( 'NONE', *, *, #15989, .F. ) ;
#393 = ORIENTED_EDGE ( 'NONE', *, *, #9573, .T. ) ;
#394 = EDGE_CURVE ( 'NONE', #38668, #51204, #28813, .T. ) ;
#395 = ORIENTED_EDGE ( 'NONE', *, *, #34509, .F. ) ;
#396 = DIRECTION ( 'NONE',  ( -0.000000000000000000, 1.000000000000000000, -0.000000000000000000 ) ) ;
#397 = CARTESIAN_POINT ( 'NONE',  ( -105.4063847101408840, -189.7472609257535510, -111.2847127925096657 ) ) ;
#398 = CARTESIAN_POINT ( 'NONE',  ( -332.3517673607765914, -174.5186198893880771, 29.74944317415823392 ) ) ;
#399 = FACE_BOUND ( 'NONE', #32267, .T. ) ;
#400 = DIRECTION ( 'NONE',  ( 0.000000000000000000, -0.8854560256532110207, -0.4647231720437664526 ) ) ;
#401 = ORIENTED_EDGE ( 'NONE', *, *, #48751, .T. ) ;
#402 = EDGE_CURVE ( 'NONE', #42461, #43377, #31986, .T. ) ;
#403 = ORIENTED_EDGE ( 'NONE', *, *, #7972, .T. ) ;
#405 = ORIENTED_EDGE ( 'NONE', *, *, #47135, .T. ) ;
#404 = DIRECTION ( 'NONE',  ( 0.000000000000000000, -0.000000000000000000, -1.000000000000000000 ) ) ;
#406 = ORIENTED_EDGE ( 'NONE', *, *, #20390, .F. ) ;
#407 = AXIS2_PLACEMENT_3D ( 'NONE', #634, #16408, #32423 ) ;
#408 = DIRECTION ( 'NONE',  ( 0.000000000000000000, 0.000000000000000000, -1.000000000000000000 ) ) ;
#409 = DIRECTION ( 'NONE',  ( -0.000000000000000000, 1.000000000000000000, -0.000000000000000000 ) ) ;
#410 = VECTOR ( 'NONE', #3277, 1000.000000000000000 ) ;
#411 = VECTOR ( 'NONE', #28290, 1000.000000000000114 ) ;
#412 = CARTESIAN_POINT ( 'NONE',  ( -339.1964088526558498, -171.7720157143598669, 33.92731199008546383 ) ) ;
#413 = CARTESIAN_POINT ( 'NONE',  ( 61.38599058177058510, -189.7472609257535510, 59.62093586438192716 ) ) ;
#414 = ORIENTED_EDGE ( 'NONE', *, *, #28899, .F. ) ;
#415 = CARTESIAN_POINT ( 'NONE',  ( -161.6832731452239500, -175.3837268820161057, -53.00774697410101055 ) ) ;
#416 = ORIENTED_EDGE ( 'NONE', *, *, #12405, .T. ) ;
#417 = AXIS2_PLACEMENT_3D ( 'NONE', #40245, #307, #23211 ) ;
#418 = ADVANCED_FACE ( 'NONE', ( #4154 ), #32244, .T. ) ;
#419 = ORIENTED_EDGE ( 'NONE', *, *, #11216, .T. ) ;
#420 = CARTESIAN_POINT ( 'NONE',  ( -58.17235712592530916, -183.6283474603465606, 123.6213615703899649 ) ) ;
#421 = AXIS2_PLACEMENT_3D ( 'NONE', #37260, #26195, #17811 ) ;
#422 = DIRECTION ( 'NONE',  ( -0.000000000000000000, 0.2393156642875685636, 0.9709418174260492362 ) ) ;
#423 = PLANE ( 'NONE',  #17324 ) ;
#424 = VECTOR ( 'NONE', #5391, 999.9999999999998863 ) ;
#425 = DIRECTION ( 'NONE',  ( 0.000000000000000000, -1.000000000000000000, 0.000000000000000000 ) ) ;
#426 = DIRECTION ( 'NONE',  ( 0.000000000000000000, -1.000000000000000000, 0.000000000000000000 ) ) ;
#427 = CARTESIAN_POINT ( 'NONE',  ( -172.9089226952081617, -175.3837268820161057, 11.92584929509620117 ) ) ;
#428 = EDGE_CURVE ( 'NONE', #27513, #27045, #24890, .T. ) ;
#429 = ORIENTED_EDGE ( 'NONE', *, *, #25783, .T. ) ;
#430 = VECTOR ( 'NONE', #3916, 1000.000000000000227 ) ;
#431 = CARTESIAN_POINT ( 'NONE',  ( -305.0000000000000568, -104.7054247829104270, -56.98038208374144631 ) ) ;
#432 = DIRECTION ( 'NONE',  ( -0.6528221181905227155, 0.000000000000000000, 0.7575112421616191360 ) ) ;
#433 = AXIS2_PLACEMENT_3D ( 'NONE', #44101, #16519, #40659 ) ;
#434 = FACE_BOUND ( 'NONE', #5358, .T. ) ;
#435 = ORIENTED_EDGE ( 'NONE', *, *, #51093, .T. ) ;
#436 = EDGE_CURVE ( 'NONE', #23558, #41176, #21468, .T. ) ;
#437 = DIRECTION ( 'NONE',  ( -0.000000000000000000, 1.000000000000000000, -0.000000000000000000 ) ) ;
#438 = CARTESIAN_POINT ( 'NONE',  ( -332.3517673607765914, -64.87442053112221174, 12.76876783163883466 ) ) ;
#439 = EDGE_LOOP ( 'NONE', ( #48444, #5234, #33273, #2136 ) ) ;
#440 = PLANE ( 'NONE',  #29634 ) ;
#441 = ORIENTED_EDGE ( 'NONE', *, *, #34593, .F. ) ;
#442 = LINE ( 'NONE', #40137, #35182 ) ;
#443 = AXIS2_PLACEMENT_3D ( 'NONE', #25570, #1406, #41340 ) ;
#444 = FACE_BOUND ( 'NONE', #2815, .T. ) ;
#446 = ORIENTED_EDGE ( 'NONE', *, *, #50072, .F. ) ;
#445 = LINE ( 'NONE', #39606, #1079 ) ;
#447 = EDGE_CURVE ( 'NONE', #41848, #50197, #50115, .T. ) ;
#448 = VECTOR ( 'NONE', #9806, 999.9999999999998863 ) ;
#449 = CIRCLE ( 'NONE', #45791, 60.00000000000000000 ) ;
#450 = DIRECTION ( 'NONE',  ( -0.000000000000000000, 1.000000000000000000, -0.000000000000000000 ) ) ;
#451 = ORIENTED_EDGE ( 'NONE', *, *, #12405, .F. ) ;
#452 = ORIENTED_EDGE ( 'NONE', *, *, #45255, .T. ) ;
#453 = DIRECTION ( 'NONE',  ( -1.000000000000000000, -0.000000000000000000, 0.000000000000000000 ) ) ;
#454 = ORIENTED_EDGE ( 'NONE', *, *, #27223, .T. ) ;
#455 = CIRCLE ( 'NONE', #14742, 125.0000000000000000 ) ;
#456 =( NAMED_UNIT ( * ) SI_UNIT ( $, .STERADIAN. ) SOLID_ANGLE_UNIT ( ) );
#457 = VECTOR ( 'NONE', #6292, 1000.000000000000000 ) ;
#458 = LINE ( 'NONE', #21229, #24488 ) ;
#459 = LINE ( 'NONE', #16516, #47341 ) ;
#460 = CIRCLE ( 'NONE', #37427, 125.0000000000000000 ) ;
#461 = VECTOR ( 'NONE', #50848, 1000.000000000000000 ) ;
#462 = DIRECTION ( 'NONE',  ( -0.000000000000000000, 1.000000000000000000, -0.000000000000000000 ) ) ;
#463 = ORIENTED_EDGE ( 'NONE', *, *, #19689, .T. ) ;
#466 = ORIENTED_EDGE ( 'NONE', *, *, #5475, .F. ) ;
#465 = DIRECTION ( 'NONE',  ( -0.000000000000000000, 1.000000000000000000, -0.000000000000000000 ) ) ;
#464 = LINE ( 'NONE', #17047, #51738 ) ;
#467 = VERTEX_POINT ( 'NONE', #40910 ) ;
#468 = DIRECTION ( 'NONE',  ( 0.000000000000000000, 0.000000000000000000, 1.000000000000000000 ) ) ;
#469 = EDGE_LOOP ( 'NONE', ( #38599, #878, #20633, #16037 ) ) ;
#470 = LINE ( 'NONE', #12822, #33168 ) ;
#471 = VERTEX_POINT ( 'NONE', #25411 ) ;
#472 = EDGE_CURVE ( 'NONE', #25437, #18236, #29078, .T. ) ;
#473 = CARTESIAN_POINT ( 'NONE',  ( -305.0000000000000568, -150.9396941197155968, -53.35787839313373127 ) ) ;
#474 = DIRECTION ( 'NONE',  ( 0.000000000000000000, 1.000000000000000000, 0.000000000000000000 ) ) ;
#475 = ORIENTED_EDGE ( 'NONE', *, *, #47971, .T. ) ;
#477 = CARTESIAN_POINT ( 'NONE',  ( -171.2727421180348415, -193.5000000000000000, 23.38221600314377113 ) ) ;
#476 = CARTESIAN_POINT ( 'NONE',  ( -111.3904503173946523, -193.5000000000000000, -106.8558168688113312 ) ) ;
#478 = ORIENTED_EDGE ( 'NONE', *, *, #41754, .F. ) ;
#479 = ORIENTED_EDGE ( 'NONE', *, *, #35123, .F. ) ;
#480 = DIRECTION ( 'NONE',  ( -0.9982437317643222396, 0.000000000000000000, 0.05924062789370006937 ) ) ;
#481 = PLANE ( 'NONE',  #41527 ) ;
#482 = DIRECTION ( 'NONE',  ( 0.000000000000000000, 0.000000000000000000, 1.000000000000000000 ) ) ;
#483 = LINE ( 'NONE', #20735, #14074 ) ;
#484 = DIRECTION ( 'NONE',  ( -0.000000000000000000, 1.000000000000000000, 0.000000000000000000 ) ) ;
#485 = AXIS2_PLACEMENT_3D ( 'NONE', #11794, #47566, #31787 ) ;
#486 = PLANE ( 'NONE',  #22221 ) ;
#487 = VECTOR ( 'NONE', #43426, 1000.000000000000000 ) ;
#488 = APPLICATION_PROTOCOL_DEFINITION ( 'draft international standard', 'automotive_design', 1998, #41108 ) ;
#489 = DIRECTION ( 'NONE',  ( 0.000000000000000000, 0.000000000000000000, -1.000000000000000000 ) ) ;
#490 = EDGE_CURVE ( 'NONE', #1315, #121, #1960, .T. ) ;
#491 = DIRECTION ( 'NONE',  ( 0.000000000000000000, -0.4647231720437664526, 0.8854560256532110207 ) ) ;
#492 = LINE ( 'NONE', #31262, #6402 ) ;
#493 = EDGE_CURVE ( 'NONE', #46777, #16167, #41946, .T. ) ;
#494 = DIRECTION ( 'NONE',  ( 0.7378332790417285736, 0.000000000000000000, -0.6749830015182091136 ) ) ;
#495 = ORIENTED_EDGE ( 'NONE', *, *, #20083, .F. ) ;
#496 = EDGE_LOOP ( 'NONE', ( #18205, #42343, #51625, #42919 ) ) ;
#497 = EDGE_CURVE ( 'NONE', #30653, #14763, #4477, .T. ) ;
#498 = DIRECTION ( 'NONE',  ( 0.7175072570443249420, 0.000000000000000000, 0.6965510290630033685 ) ) ;
#499 = AXIS2_PLACEMENT_3D ( 'NONE', #42166, #25251, #24463 ) ;
#500 = AXIS2_PLACEMENT_3D ( 'NONE', #889, #41099, #37682 ) ;
#501 = CARTESIAN_POINT ( 'NONE',  ( -47.51449116960048968, -175.3837268820161057, 0.2635871660690785045 ) ) ;
#502 = CARTESIAN_POINT ( 'NONE',  ( 3.652658254809377336, -183.6283474603465606, -112.5098962032389522 ) ) ;
#503 = VERTEX_POINT ( 'NONE', #45393 ) ;
#504 = ORIENTED_EDGE ( 'NONE', *, *, #17516, .T. ) ;
#505 = VECTOR ( 'NONE', #2539, 1000.000000000000000 ) ;
#506 = ORIENTED_EDGE ( 'NONE', *, *, #34160, .T. ) ;
#507 = AXIS2_PLACEMENT_3D ( 'NONE', #38992, #47165, #35568 ) ;
#508 = LINE ( 'NONE', #40199, #762 ) ;
#509 = DIRECTION ( 'NONE',  ( 0.000000000000000000, 1.000000000000000000, 0.000000000000000000 ) ) ;
#510 = CARTESIAN_POINT ( 'NONE',  ( -336.3521761649654422, -87.81784868886214213, 47.06073758877343494 ) ) ;
#511 = DIRECTION ( 'NONE',  ( 1.000000000000000000, -0.000000000000000000, 0.000000000000000000 ) ) ;
#512 = VERTEX_POINT ( 'NONE', #41693 ) ;
#513 = CARTESIAN_POINT ( 'NONE',  ( -330.4913330509368166, -89.82879061784696262, -49.66134974749687103 ) ) ;
#514 = DIRECTION ( 'NONE',  ( -0.000000000000000000, 1.000000000000000000, -0.000000000000000000 ) ) ;
#515 = EDGE_LOOP ( 'NONE', ( #35303, #20587, #15349, #40172 ) ) ;
#516 = DIRECTION ( 'NONE',  ( -0.000000000000000000, 1.000000000000000000, -0.000000000000000000 ) ) ;
#517 = ORIENTED_EDGE ( 'NONE', *, *, #50630, .F. ) ;
#518 = AXIS2_PLACEMENT_3D ( 'NONE', #30428, #18860, #10727 ) ;
#519 = CIRCLE ( 'NONE', #6403, 4.999999999999997335 ) ;
#520 = EDGE_LOOP ( 'NONE', ( #44694, #25345, #12703, #2844 ) ) ;
#521 = DIRECTION ( 'NONE',  ( 1.000000000000000000, -0.000000000000000000, -0.000000000000000000 ) ) ;
#522 = AXIS2_PLACEMENT_3D ( 'NONE', #5834, #21590, #45254 ) ;
#523 = CARTESIAN_POINT ( 'NONE',  ( -48.65601702663143868, -175.3837268820161057, 0.9842305779476024918 ) ) ;
#524 = DIRECTION ( 'NONE',  ( 0.000000000000000000, 1.000000000000000000, 0.000000000000000000 ) ) ;
#527 = ORIENTED_EDGE ( 'NONE', *, *, #25028, .F. ) ;
#526 = LINE ( 'NONE', #16591, #33385 ) ;
#525 = DIRECTION ( 'NONE',  ( 0.9564009842765244240, 0.000000000000000000, -0.2920567706369695538 ) ) ;
#528 = VECTOR ( 'NONE', #5098, 1000.000000000000000 ) ;
#529 =( GEOMETRIC_REPRESENTATION_CONTEXT ( 3 ) GLOBAL_UNCERTAINTY_ASSIGNED_CONTEXT ( ( #31631 ) ) GLOBAL_UNIT_ASSIGNED_CONTEXT ( ( #33419, #33134, #45500 ) ) REPRESENTATION_CONTEXT ( 'NONE', 'WORKASPACE' ) );
#530 = VECTOR ( 'NONE', #17595, 1000.000000000000114 ) ;
#531 = DIRECTION ( 'NONE',  ( 0.000000000000000000, 0.000000000000000000, -1.000000000000000000 ) ) ;
#533 = ORIENTED_EDGE ( 'NONE', *, *, #2819, .F. ) ;
#532 = VECTOR ( 'NONE', #16412, 1000.000000000000000 ) ;
#534 = DIRECTION ( 'NONE',  ( -1.000000000000000000, 0.000000000000000000, 0.000000000000000000 ) ) ;
#535 = CARTESIAN_POINT ( 'NONE',  ( -48.47912675150885065, -177.1207230881787780, 6.938893903907228378E-15 ) ) ;
#536 = EDGE_LOOP ( 'NONE', ( #8280, #13076, #45536, #37068 ) ) ;
#537 = EDGE_CURVE ( 'NONE', #48832, #33712, #33804, .T. ) ;
#538 = ADVANCED_FACE ( 'NONE', ( #9385 ), #38000, .T. ) ;
#539 = ADVANCED_FACE ( 'NONE', ( #1222 ), #33292, .T. ) ;
#540 = CYLINDRICAL_SURFACE ( 'NONE', #26625, 125.0000000000000000 ) ;
#541 = CIRCLE ( 'NONE', #34986, 125.0000000000000000 ) ;
#542 = PLANE ( 'NONE',  #18314 ) ;
#544 = CARTESIAN_POINT ( 'NONE',  ( -330.4913330509368166, -96.52406086224436876, -52.47426709956133806 ) ) ;
#543 = PLANE ( 'NONE',  #42489 ) ;
#545 = ORIENTED_EDGE ( 'NONE', *, *, #18432, .T. ) ;
#546 = ADVANCED_FACE ( 'NONE', ( #5447 ), #41169, .F. ) ;
#547 = AXIS2_PLACEMENT_3D ( 'NONE', #8240, #28457, #27946 ) ;
#548 = DIRECTION ( 'NONE',  ( 0.000000000000000000, 1.156482317317871449E-14, 1.000000000000000000 ) ) ;
#549 = CARTESIAN_POINT ( 'NONE',  ( -336.3521761649654422, -94.63601285149479736, 51.48334306143172512 ) ) ;
#550 = DIRECTION ( 'NONE',  ( -0.000000000000000000, -1.000000000000000000, 0.000000000000000000 ) ) ;
#551 = ORIENTED_EDGE ( 'NONE', *, *, #41443, .F. ) ;
#552 = EDGE_CURVE ( 'NONE', #15284, #26962, #8852, .T. ) ;
#553 = CARTESIAN_POINT ( 'NONE',  ( -47.82630463331833681, -175.3837268820161057, 0.7575112421616305713 ) ) ;
#554 = CARTESIAN_POINT ( 'NONE',  ( -59.86929868745811945, -183.6283474603465606, -124.4799742258549458 ) ) ;
#555 = EDGE_CURVE ( 'NONE', #9556, #9203, #5961, .T. ) ;
#556 = DIRECTION ( 'NONE',  ( 0.8455960035018234011, 0.000000000000000000, 0.5338233779647948429 ) ) ;
#557 = ORIENTED_EDGE ( 'NONE', *, *, #40396, .F. ) ;
#558 = CARTESIAN_POINT ( 'NONE',  ( -165.2002711502080672, -177.1207230881787780, 44.73448837594998651 ) ) ;
#559 = EDGE_CURVE ( 'NONE', #4633, #10838, #13706, .T. ) ;
#560 = DIRECTION ( 'NONE',  ( 0.000000000000000000, -1.000000000000000000, 0.000000000000000000 ) ) ;
#561 = ADVANCED_FACE ( 'NONE', ( #17273 ), #45651, .T. ) ;
#562 = ADVANCED_FACE ( 'NONE', ( #30126 ), #20957, .T. ) ;
#563 = VERTEX_POINT ( 'NONE', #10148 ) ;
#564 = DIRECTION ( 'NONE',  ( 0.000000000000000000, 0.000000000000000000, -1.000000000000000000 ) ) ;
#565 = ORIENTED_EDGE ( 'NONE', *, *, #9989, .F. ) ;
#566 = AXIS2_PLACEMENT_3D ( 'NONE', #47062, #11037, #17979 ) ;
#567 = VECTOR ( 'NONE', #28228, 1000.000000000000000 ) ;
#568 = EDGE_CURVE ( 'NONE', #13340, #30763, #46948, .T. ) ;
#569 = CARTESIAN_POINT ( 'NONE',  ( -339.1964088526558498, -84.75001853787809125, 44.49369547121489887 ) ) ;
#570 = DIRECTION ( 'NONE',  ( -0.000000000000000000, 1.000000000000000000, -0.000000000000000000 ) ) ;
#571 = AXIS2_PLACEMENT_3D ( 'NONE', #47908, #11884, #19515 ) ;
#572 = EDGE_CURVE ( 'NONE', #18675, #17957, #26165, .T. ) ;
#573 = DIRECTION ( 'NONE',  ( 0.4566292373937077542, 0.000000000000000000, 0.8896570909947499883 ) ) ;
#574 = LINE ( 'NONE', #20541, #13865 ) ;
#575 = FACE_OUTER_BOUND ( 'NONE', #48196, .T. ) ;
#576 = DIRECTION ( 'NONE',  ( 0.000000000000000000, 0.000000000000000000, -1.000000000000000000 ) ) ;
#577 = VECTOR ( 'NONE', #4041, 1000.000000000000000 ) ;
#578 = CARTESIAN_POINT ( 'NONE',  ( -330.4913330509368166, -157.4273119900845757, 48.27201571436049932 ) ) ;
#579 = PLANE ( 'NONE',  #5256 ) ;
#581 = ORIENTED_EDGE ( 'NONE', *, *, #32751, .F. ) ;
#580 = DIRECTION ( 'NONE',  ( 0.000000000000000000, 0.000000000000000000, 1.000000000000000000 ) ) ;
#582 = VECTOR ( 'NONE', #15550, 1000.000000000000000 ) ;
#583 = AXIS2_PLACEMENT_3D ( 'NONE', #26617, #42121, #49770 ) ;
#584 = ORIENTED_EDGE ( 'NONE', *, *, #37671, .T. ) ;
#585 = CARTESIAN_POINT ( 'NONE',  ( -116.2964108826154330, -193.5000000000000000, -105.0038855142073260 ) ) ;
#586 = AXIS2_PLACEMENT_3D ( 'NONE', #20301, #16649, #32387 ) ;
#587 = EDGE_CURVE ( 'NONE', #26454, #4175, #3633, .T. ) ;
#588 = AXIS2_PLACEMENT_3D ( 'NONE', #26268, #42293, #6829 ) ;
#589 = LINE ( 'NONE', #24496, #50635 ) ;
#590 = ORIENTED_EDGE ( 'NONE', *, *, #34142, .F. ) ;
#591 = ORIENTED_EDGE ( 'NONE', *, *, #49335, .F. ) ;
#592 = EDGE_LOOP ( 'NONE', ( #44540, #11697, #28068, #50995 ) ) ;
#593 = DIRECTION ( 'NONE',  ( 0.9473263538541899509, 0.000000000000000000, 0.3202698538628415692 ) ) ;
#594 = CARTESIAN_POINT ( 'NONE',  ( 76.28370911321322012, -177.1207230881787780, -7.696413904697510411 ) ) ;
#595 = DIRECTION ( 'NONE',  ( -1.000000000000000000, 0.000000000000000000, -0.000000000000000000 ) ) ;
#596 = ORIENTED_EDGE ( 'NONE', *, *, #42681, .F. ) ;
#597 = ADVANCED_FACE ( 'NONE', ( #6737 ), #50883, .T. ) ;
#598 = DIRECTION ( 'NONE',  ( -0.000000000000000000, 1.000000000000000000, -0.000000000000000000 ) ) ;
#599 = DIRECTION ( 'NONE',  ( -0.000000000000000000, 1.000000000000000000, -0.000000000000000000 ) ) ;
#600 = VECTOR ( 'NONE', #9609, 1000.000000000000000 ) ;
#602 = VERTEX_POINT ( 'NONE', #27200 ) ;
#601 = FACE_OUTER_BOUND ( 'NONE', #39994, .T. ) ;
#603 = CIRCLE ( 'NONE', #46761, 125.0000000000000000 ) ;
#604 = DIRECTION ( 'NONE',  ( -0.9960498426152158968, 0.000000000000000000, -0.08879589532294571153 ) ) ;
#605 = CARTESIAN_POINT ( 'NONE',  ( 67.29303306501925874, -175.3837268820161057, 47.13604789772129777 ) ) ;
#606 = ORIENTED_EDGE ( 'NONE', *, *, #1748, .F. ) ;
#607 = CARTESIAN_POINT ( 'NONE',  ( -330.4913330509368166, -108.6560878169896256, 58.13482838284702581 ) ) ;
#608 = VECTOR ( 'NONE', #44679, 1000.000000000000114 ) ;
#609 = EDGE_LOOP ( 'NONE', ( #43892, #41673, #35161, #47597 ) ) ;
#610 = ADVANCED_FACE ( 'NONE', ( #10402 ), #26946, .F. ) ;
#611 = ADVANCED_FACE ( 'NONE', ( #22233 ), #22758, .F. ) ;
#612 = EDGE_CURVE ( 'NONE', #17894, #29760, #22933, .T. ) ;
#613 = ADVANCED_FACE ( 'NONE', ( #30368 ), #18310, .T. ) ;
#614 = CARTESIAN_POINT ( 'NONE',  ( -102.0975050429523776, -183.6283474603465606, -111.8087531435654682 ) ) ;
#615 = LINE ( 'NONE', #29498, #4504 ) ;
#616 = DIRECTION ( 'NONE',  ( -0.7948544414133523750, 0.000000000000000000, -0.6068001458185945385 ) ) ;
#617 = EDGE_CURVE ( 'NONE', #30167, #21474, #51158, .T. ) ;
#618 = ORIENTED_EDGE ( 'NONE', *, *, #18542, .T. ) ;
#619 = CIRCLE ( 'NONE', #20770, 60.00000000000000000 ) ;
#620 = ORIENTED_EDGE ( 'NONE', *, *, #35779, .F. ) ;
#621 = CARTESIAN_POINT ( 'NONE',  ( -47.55243714407701816, -189.7472609257535510, -0.3758275821142288420 ) ) ;
#622 = DIRECTION ( 'NONE',  ( 0.000000000000000000, 0.000000000000000000, -1.000000000000000000 ) ) ;
#623 = CONICAL_SURFACE ( 'NONE', #29126, 10.00000000000000711, 0.03490658503988659789 ) ;
#624 = ORIENTED_EDGE ( 'NONE', *, *, #8566, .T. ) ;
#625 = EDGE_CURVE ( 'NONE', #8999, #27120, #46420, .T. ) ;
#626 = EDGE_CURVE ( 'NONE', #50991, #48252, #50369, .T. ) ;
#627 = DIRECTION ( 'NONE',  ( 0.000000000000000000, -1.000000000000000000, -0.000000000000000000 ) ) ;
#628 = AXIS2_PLACEMENT_3D ( 'NONE', #14923, #21763, #1775 ) ;
#629 = DIRECTION ( 'NONE',  ( -1.000000000000000000, -0.000000000000000000, 0.000000000000000000 ) ) ;
#630 = ORIENTED_EDGE ( 'NONE', *, *, #47620, .F. ) ;
#631 = CARTESIAN_POINT ( 'NONE',  ( -365.0000000000001137, -78.50000000000002842, 0.000000000000000000 ) ) ;
#632 = AXIS2_PLACEMENT_3D ( 'NONE', #7367, #43090, #14727 ) ;
#633 = EDGE_CURVE ( 'NONE', #35850, #14215, #51404, .T. ) ;
#634 = CARTESIAN_POINT ( 'NONE',  ( 0.000000000000000000, -162.6242368362065918, 44.16213414209531862 ) ) ;
#635 = EDGE_CURVE ( 'NONE', #30065, #6051, #38528, .T. ) ;
#636 = VECTOR ( 'NONE', #32808, 1000.000000000000000 ) ;
#637 = ORIENTED_EDGE ( 'NONE', *, *, #43796, .F. ) ;
#638 = CARTESIAN_POINT ( 'NONE',  ( -23.01747912075234836, -193.5000000000000000, -122.3793467049370634 ) ) ;
#639 = ORIENTED_EDGE ( 'NONE', *, *, #7258, .T. ) ;
#640 = LINE ( 'NONE', #48731, #27621 ) ;
#641 = EDGE_CURVE ( 'NONE', #20455, #18266, #17916, .T. ) ;
#642 = FACE_OUTER_BOUND ( 'NONE', #50489, .T. ) ;
#643 = ORIENTED_EDGE ( 'NONE', *, *, #44701, .T. ) ;
#644 = EDGE_CURVE ( 'NONE', #25704, #37475, #2776, .T. ) ;
#645 = DIRECTION ( 'NONE',  ( -0.8757349421956412971, 0.000000000000000000, 0.4827922027307366970 ) ) ;
#646 = DIRECTION ( 'NONE',  ( 1.000000000000000000, -0.000000000000000000, 6.978251959525016136E-17 ) ) ;
#647 = DIRECTION ( 'NONE',  ( 0.000000000000000000, 0.1205366802553164696, -0.9927088740980548609 ) ) ;
#648 = DIRECTION ( 'NONE',  ( 0.000000000000000000, 0.000000000000000000, -1.000000000000000000 ) ) ;
#649 = EDGE_CURVE ( 'NONE', #21906, #4350, #15399, .T. ) ;
#650 = VERTEX_POINT ( 'NONE', #26700 ) ;
#651 = CARTESIAN_POINT ( 'NONE',  ( -81.70897914701308196, -183.6283474603465606, -120.5021863277716534 ) ) ;
#652 = ORIENTED_EDGE ( 'NONE', *, *, #33377, .T. ) ;
#653 = VERTEX_POINT ( 'NONE', #42734 ) ;
#654 = CIRCLE ( 'NONE', #29192, 125.0000000000000000 ) ;
#655 = VECTOR ( 'NONE', #37602, 1000.000000000000114 ) ;
#656 = CARTESIAN_POINT ( 'NONE',  ( -92.43312097795266880, -175.3837268820161057, -115.9484881370935483 ) ) ;
#658 = ORIENTED_EDGE ( 'NONE', *, *, #5431, .T. ) ;
#657 = DIRECTION ( 'NONE',  ( 0.000000000000000000, -1.000000000000000000, 0.000000000000000000 ) ) ;
#659 = ORIENTED_EDGE ( 'NONE', *, *, #1459, .T. ) ;
#660 = DIRECTION ( 'NONE',  ( -0.000000000000000000, 0.6631226582407863113, -0.7485107481711089639 ) ) ;
#661 = EDGE_CURVE ( 'NONE', #39966, #40406, #17095, .T. ) ;
#662 = DIRECTION ( 'NONE',  ( -1.000000000000000000, 0.000000000000000000, -0.000000000000000000 ) ) ;
#663 = VECTOR ( 'NONE', #44301, 1000.000000000000000 ) ;
#664 = VERTEX_POINT ( 'NONE', #28494 ) ;
#665 = CARTESIAN_POINT ( 'NONE',  ( 9.518239912201957864, -213.5000000000000000, 110.7307791902283043 ) ) ;
#666 = ORIENTED_EDGE ( 'NONE', *, *, #48169, .F. ) ;
#667 = CARTESIAN_POINT ( 'NONE',  ( -330.4913330509368166, -150.4759391377553186, 52.47426709956150859 ) ) ;
#668 = CARTESIAN_POINT ( 'NONE',  ( -48.71401279728984690, -175.3837268820161057, 0.9720229140804159673 ) ) ;
#669 = CARTESIAN_POINT ( 'NONE',  ( -9.671950287350391307, -177.1207230881787780, -118.8234112238815641 ) ) ;
#670 = DIRECTION ( 'NONE',  ( -0.000000000000000000, 1.000000000000000000, -0.000000000000000000 ) ) ;
#671 = ORIENTED_EDGE ( 'NONE', *, *, #14170, .F. ) ;
#672 = VERTEX_POINT ( 'NONE', #23531 ) ;
#673 = ORIENTED_EDGE ( 'NONE', *, *, #38806, .F. ) ;
#674 = VECTOR ( 'NONE', #17108, 1000.000000000000000 ) ;
#675 = CARTESIAN_POINT ( 'NONE',  ( 70.68712318874649725, -193.5000000000000000, -37.74128873232327663 ) ) ;
#676 = CARTESIAN_POINT ( 'NONE',  ( -59.28786813212837359, -177.1207230881787780, 124.5318076226587323 ) ) ;
#677 = DIRECTION ( 'NONE',  ( 0.000000000000000000, 0.000000000000000000, -1.000000000000000000 ) ) ;
#678 = CARTESIAN_POINT ( 'NONE',  ( -305.0000000000000568, -123.5000000000000284, 0.000000000000000000 ) ) ;
#679 = DIRECTION ( 'NONE',  ( 0.000000000000000000, -0.000000000000000000, -1.000000000000000000 ) ) ;
#680 = ORIENTED_EDGE ( 'NONE', *, *, #28374, .T. ) ;
#681 = EDGE_CURVE ( 'NONE', #49313, #49622, #43755, .T. ) ;
#682 = ADVANCED_FACE ( 'NONE', ( #43509 ), #31674, .F. ) ;
#683 = EDGE_LOOP ( 'NONE', ( #15147, #11656, #13583, #27814 ) ) ;
#685 = ORIENTED_EDGE ( 'NONE', *, *, #39363, .T. ) ;
#684 = CARTESIAN_POINT ( 'NONE',  ( 2.266533711611407043, -189.7472609257535510, 113.1409892739925453 ) ) ;
#686 = PLANE ( 'NONE',  #7824 ) ;
#687 = VECTOR ( 'NONE', #26344, 999.9999999999998863 ) ;
#688 = ORIENTED_EDGE ( 'NONE', *, *, #14374, .T. ) ;
#689 = AXIS2_PLACEMENT_3D ( 'NONE', #43278, #30663, #18596 ) ;
#691 = CIRCLE ( 'NONE', #15817, 125.0000000000000000 ) ;
#690 = FACE_OUTER_BOUND ( 'NONE', #23025, .T. ) ;
#692 = CARTESIAN_POINT ( 'NONE',  ( 60.00000000000000000, -113.5000000000000000, 60.00000000000000711 ) ) ;
#693 = VECTOR ( 'NONE', #26320, 1000.000000000000000 ) ;
#694 = CARTESIAN_POINT ( 'NONE',  ( -162.3451783319732442, -193.5000000000000000, 51.57055649762783389 ) ) ;
#695 = DIRECTION ( 'NONE',  ( -1.000000000000000000, -0.000000000000000000, -0.000000000000000000 ) ) ;
#696 = ORIENTED_EDGE ( 'NONE', *, *, #41387, .T. ) ;
#697 = FACE_OUTER_BOUND ( 'NONE', #41985, .T. ) ;
#698 = ORIENTED_EDGE ( 'NONE', *, *, #20067, .T. ) ;
#699 = ORIENTED_EDGE ( 'NONE', *, *, #15129, .T. ) ;
#700 = DIRECTION ( 'NONE',  ( 0.000000000000000000, -0.8854560256532093554, 0.4647231720437695057 ) ) ;
#701 = VECTOR ( 'NONE', #47280, 1000.000000000000000 ) ;
#702 = ADVANCED_FACE ( 'NONE', ( #27983 ), #12209, .T. ) ;
#703 = CARTESIAN_POINT ( 'NONE',  ( 75.02564229359539638, -175.3837268820161057, -19.27620354518634826 ) ) ;
#704 = DIRECTION ( 'NONE',  ( 0.000000000000000000, 0.000000000000000000, 1.000000000000000000 ) ) ;
#705 = LINE ( 'NONE', #17971, #36499 ) ;
#706 = CARTESIAN_POINT ( 'NONE',  ( -336.3521761649654422, -64.50000000000000000, -2.632288850093980503 ) ) ;
#707 = FACE_OUTER_BOUND ( 'NONE', #11234, .T. ) ;
#708 = DIRECTION ( 'NONE',  ( 0.6965510290629982615, 0.000000000000000000, -0.7175072570443298270 ) ) ;
#709 = ORIENTED_EDGE ( 'NONE', *, *, #13446, .T. ) ;
#710 = LINE ( 'NONE', #28803, #21329 ) ;
#711 = LINE ( 'NONE', #28547, #40806 ) ;
#712 = ADVANCED_FACE ( 'NONE', ( #16169 ), #36129, .F. ) ;
#713 = VECTOR ( 'NONE', #18142, 1000.000000000000000 ) ;
#714 = LINE ( 'NONE', #49585, #32837 ) ;
#715 = FACE_BOUND ( 'NONE', #39731, .T. ) ;
#716 = VERTEX_POINT ( 'NONE', #8281 ) ;
#717 = FACE_OUTER_BOUND ( 'NONE', #32723, .T. ) ;
#718 = ORIENTED_EDGE ( 'NONE', *, *, #2218, .F. ) ;
#719 = DIRECTION ( 'NONE',  ( 1.000000000000000000, 0.000000000000000000, 0.000000000000000000 ) ) ;
#720 = ORIENTED_EDGE ( 'NONE', *, *, #4486, .T. ) ;
#721 = LINE ( 'NONE', #24371, #22893 ) ;
#722 = EDGE_LOOP ( 'NONE', ( #13255, #44779, #48049, #3646 ) ) ;
#723 = CARTESIAN_POINT ( 'NONE',  ( -106.2948367055610106, -189.7472609257535510, -110.8257356506552185 ) ) ;
#724 = AXIS2_PLACEMENT_3D ( 'NONE', #34745, #11088, #18732 ) ;
#725 = VECTOR ( 'NONE', #35694, 1000.000000000000114 ) ;
#726 = FACE_BOUND ( 'NONE', #3636, .T. ) ;
#728 = VERTEX_POINT ( 'NONE', #39544 ) ;
#727 = CARTESIAN_POINT ( 'NONE',  ( -330.4913330509368166, -131.1080185721124849, 58.50955523165764305 ) ) ;
#729 = VECTOR ( 'NONE', #13592, 1000.000000000000114 ) ;
#730 = CARTESIAN_POINT ( 'NONE',  ( -332.3517673607765914, -170.5607375887735770, 35.68215131113770155 ) ) ;
#731 = EDGE_LOOP ( 'NONE', ( #11953, #13338, #18048, #14655 ) ) ;
#732 = ORIENTED_EDGE ( 'NONE', *, *, #40407, .F. ) ;
#733 = CARTESIAN_POINT ( 'NONE',  ( -49.45768324380835423, -183.6283474603465606, 0.2059786187410958813 ) ) ;
#734 = VECTOR ( 'NONE', #15159, 1000.000000000000000 ) ;
#735 = CARTESIAN_POINT ( 'NONE',  ( -127.4665351220365892, -177.1207230881787780, -96.88131563365291754 ) ) ;
#736 = ORIENTED_EDGE ( 'NONE', *, *, #2249, .F. ) ;
#737 = SURFACE_STYLE_FILL_AREA ( #32790 ) ;
#738 = CARTESIAN_POINT ( 'NONE',  ( 0.000000000000000000, 108.6102204319011832, -108.9186595926644969 ) ) ;
#739 = DIRECTION ( 'NONE',  ( 1.000000000000000000, -7.719741424018441012E-17, 4.051632851310786670E-17 ) ) ;
#740 = ADVANCED_FACE ( 'NONE', ( #35605 ), #3552, .F. ) ;
#741 = VECTOR ( 'NONE', #42768, 1000.000000000000000 ) ;
#742 = DIRECTION ( 'NONE',  ( 0.000000000000000000, -1.000000000000000000, 0.000000000000000000 ) ) ;
#743 = LINE ( 'NONE', #44889, #7201 ) ;
#744 = ORIENTED_EDGE ( 'NONE', *, *, #18260, .T. ) ;
#747 = EDGE_LOOP ( 'NONE', ( #32037, #24725, #215, #545 ) ) ;
#746 = CARTESIAN_POINT ( 'NONE',  ( -46.00000000000000711, 0.000000000000000000, 8.673617379884035472E-15 ) ) ;
#745 = DIRECTION ( 'NONE',  ( -0.000000000000000000, -1.000000000000000000, -0.000000000000000000 ) ) ;
#748 = ORIENTED_EDGE ( 'NONE', *, *, #46870, .F. ) ;
#749 = PLANE ( 'NONE',  #44990 ) ;
#750 = EDGE_LOOP ( 'NONE', ( #47763, #48042, #43578, #36505 ) ) ;
#751 = DIRECTION ( 'NONE',  ( -0.000000000000000000, -1.000000000000000000, 0.000000000000000000 ) ) ;
#752 = ORIENTED_EDGE ( 'NONE', *, *, #16107, .F. ) ;
#753 = FACE_OUTER_BOUND ( 'NONE', #12516, .T. ) ;
#754 = LINE ( 'NONE', #16800, #2405 ) ;
#755 = VERTEX_POINT ( 'NONE', #51930 ) ;
#757 = DIRECTION ( 'NONE',  ( -0.000000000000000000, 1.000000000000000000, -0.000000000000000000 ) ) ;
#756 = DIRECTION ( 'NONE',  ( 1.000000000000000000, -0.000000000000000000, 0.000000000000000000 ) ) ;
#758 = ORIENTED_EDGE ( 'NONE', *, *, #47440, .F. ) ;
#759 = ORIENTED_EDGE ( 'NONE', *, *, #12652, .T. ) ;
#760 = CARTESIAN_POINT ( 'NONE',  ( -37.78865854180985195, -183.6283474603465606, -123.5388265266451242 ) ) ;
#761 = CARTESIAN_POINT ( 'NONE',  ( -339.1964088526558498, -137.1341532842523065, 57.40522506028101901 ) ) ;
#762 = VECTOR ( 'NONE', #33094, 1000.000000000000000 ) ;
#763 = ADVANCED_FACE ( 'NONE', ( #11698 ), #48503, .F. ) ;
#764 = CARTESIAN_POINT ( 'NONE',  ( -330.4913330509368166, -102.1108035431471279, 54.98865587491800255 ) ) ;
#765 = CARTESIAN_POINT ( 'NONE',  ( 22.03849146056077757, -175.3837268820161057, 103.2098131075567267 ) ) ;
#766 = ORIENTED_EDGE ( 'NONE', *, *, #47209, .F. ) ;
#767 = AXIS2_PLACEMENT_3D ( 'NONE', #28514, #22135, #9088 ) ;
#768 = CARTESIAN_POINT ( 'NONE',  ( -160.4991136281923332, -193.5000000000000000, 53.17445600718630061 ) ) ;
#769 = DIRECTION ( 'NONE',  ( 1.000000000000000000, 0.000000000000000000, 0.000000000000000000 ) ) ;
#770 = CARTESIAN_POINT ( 'NONE',  ( -48.47912675150885065, -189.7472609257535510, 6.938893903907228378E-15 ) ) ;
#771 = LINE ( 'NONE', #21264, #26347 ) ;
#772 = CARTESIAN_POINT ( 'NONE',  ( -339.1964088526558498, -79.66942718702493664, 39.49849221029193558 ) ) ;
#773 = DIRECTION ( 'NONE',  ( 0.000000000000000000, -1.000000000000000000, 0.000000000000000000 ) ) ;
#774 = EDGE_LOOP ( 'NONE', ( #44968, #19861, #24735, #2334 ) ) ;
#775 = VERTEX_POINT ( 'NONE', #27723 ) ;
#776 = DIRECTION ( 'NONE',  ( 0.000000000000000000, -0.000000000000000000, -1.000000000000000000 ) ) ;
#777 = DIRECTION ( 'NONE',  ( 0.000000000000000000, 0.000000000000000000, -1.000000000000000000 ) ) ;
#778 = FACE_OUTER_BOUND ( 'NONE', #41872, .T. ) ;
#779 = VERTEX_POINT ( 'NONE', #32188 ) ;
#780 = ORIENTED_EDGE ( 'NONE', *, *, #5158, .F. ) ;
#781 = ORIENTED_EDGE ( 'NONE', *, *, #37550, .T. ) ;
#782 = VECTOR ( 'NONE', #29574, 1000.000000000000000 ) ;
#783 = DIRECTION ( 'NONE',  ( 0.000000000000000000, 0.000000000000000000, -1.000000000000000000 ) ) ;
#784 = DIRECTION ( 'NONE',  ( 0.9720229140804089729, 0.000000000000000000, 0.2348860457809911206 ) ) ;
#785 = LINE ( 'NONE', #510, #16196 ) ;
#786 = FACE_OUTER_BOUND ( 'NONE', #39466, .T. ) ;
#787 = VERTEX_POINT ( 'NONE', #11430 ) ;
#788 = EDGE_CURVE ( 'NONE', #45751, #9248, #24559, .T. ) ;
#789 = CARTESIAN_POINT ( 'NONE',  ( -330.4913330509368166, -183.1207326066167411, -6.735595255826296146 ) ) ;
#790 = CARTESIAN_POINT ( 'NONE',  ( 23.33927677392130917, -183.6283474603465606, -102.3089288139528747 ) ) ;
#791 = ORIENTED_EDGE ( 'NONE', *, *, #493, .T. ) ;
#792 = CARTESIAN_POINT ( 'NONE',  ( -164.3791542526839180, -175.3837268820161057, 46.82076062204521349 ) ) ;
#793 = EDGE_CURVE ( 'NONE', #5683, #31493, #23789, .T. ) ;
#794 = VERTEX_POINT ( 'NONE', #32452 ) ;
#795 = AXIS2_PLACEMENT_3D ( 'NONE', #19587, #662, #28498 ) ;
#796 = ORIENTED_EDGE ( 'NONE', *, *, #49816, .F. ) ;
#797 = DIRECTION ( 'NONE',  ( -0.7765238627180393038, 0.000000000000000000, -0.6300878435817147682 ) ) ;
#798 = VECTOR ( 'NONE', #3197, 1000.000000000000000 ) ;
#799 = EDGE_CURVE ( 'NONE', #11174, #43506, #40316, .T. ) ;
#800 = EDGE_CURVE ( 'NONE', #35554, #10123, #31928, .T. ) ;
#801 = LINE ( 'NONE', #5808, #45204 ) ;
#802 = PRODUCT ( 'Lockable Linear Guide', 'Lockable Linear Guide', '', ( #17073 ) ) ;
#803 = CARTESIAN_POINT ( 'NONE',  ( -332.3517673607765914, -100.1170788342122080, 54.23253582808833073 ) ) ;
#806 = ORIENTED_EDGE ( 'NONE', *, *, #37358, .F. ) ;
#805 = CARTESIAN_POINT ( 'NONE',  ( 46.00000000000000711, 0.000000000000000000, 41.00000000000000000 ) ) ;
#804 = LINE ( 'NONE', #44961, #32554 ) ;
#807 = EDGE_CURVE ( 'NONE', #6494, #17445, #2198, .T. ) ;
#808 = DIRECTION ( 'NONE',  ( -0.9027978299657416494, 0.000000000000000000, -0.4300652022765245608 ) ) ;
#809 = VERTEX_POINT ( 'NONE', #15919 ) ;
#810 = LINE ( 'NONE', #33403, #44881 ) ;
#811 = CARTESIAN_POINT ( 'NONE',  ( -124.9871112439422092, -175.3837268820161057, -98.85104101073275729 ) ) ;
#812 = ORIENTED_EDGE ( 'NONE', *, *, #27131, .F. ) ;
#813 = CARTESIAN_POINT ( 'NONE',  ( -140.5285791076019279, -189.7472609257535510, -83.08371579725672973 ) ) ;
#815 = DIRECTION ( 'NONE',  ( -1.000000000000000000, -0.000000000000000000, -0.000000000000000000 ) ) ;
#814 = CARTESIAN_POINT ( 'NONE',  ( -339.1964088526558498, -175.9742670995615015, -26.97593913775538965 ) ) ;
#816 = ORIENTED_EDGE ( 'NONE', *, *, #28380, .T. ) ;
#817 = VECTOR ( 'NONE', #4352, 999.9999999999998863 ) ;
#818 = CARTESIAN_POINT ( 'NONE',  ( -170.0000000000000284, -123.5000000000000284, -15.24495751795538290 ) ) ;
#819 = CARTESIAN_POINT ( 'NONE',  ( -180.0000000000000568, -130.6726371812771959, 60.00000000000000711 ) ) ;
#820 = DIRECTION ( 'NONE',  ( -0.000000000000000000, -0.9350162426854169428, -0.3546048870425300148 ) ) ;
#821 = ORIENTED_EDGE ( 'NONE', *, *, #21477, .T. ) ;
#822 = EDGE_CURVE ( 'NONE', #37318, #29662, #44017, .T. ) ;
#823 = DIRECTION ( 'NONE',  ( 0.05924062789371441901, 0.000000000000000000, -0.9982437317643214625 ) ) ;
#824 = LINE ( 'NONE', #19745, #7267 ) ;
#825 = FACE_OUTER_BOUND ( 'NONE', #25719, .T. ) ;
#826 = ORIENTED_EDGE ( 'NONE', *, *, #45474, .F. ) ;
#827 = FACE_OUTER_BOUND ( 'NONE', #21946, .T. ) ;
#828 = CARTESIAN_POINT ( 'NONE',  ( -260.0000000000000000, -113.5000000000000000, -40.00000000000001421 ) ) ;
#829 = ORIENTED_EDGE ( 'NONE', *, *, #34198, .F. ) ;
#830 = CIRCLE ( 'NONE', #7550, 60.00000000000000000 ) ;
#831 = LINE ( 'NONE', #36308, #22296 ) ;
#832 = CARTESIAN_POINT ( 'NONE',  ( -171.7300019102062549, -193.5000000000000000, -20.83798868929510562 ) ) ;
#833 = DIRECTION ( 'NONE',  ( 0.1768902751225666370, 0.000000000000000000, 0.9842305779475979399 ) ) ;
#834 = DIRECTION ( 'NONE',  ( 0.000000000000000000, 0.000000000000000000, 1.000000000000000000 ) ) ;
#835 = DIRECTION ( 'NONE',  ( 0.000000000000000000, 1.000000000000000000, 0.000000000000000000 ) ) ;
#836 = CARTESIAN_POINT ( 'NONE',  ( 63.10841233855954613, -193.5000000000000000, -54.07611884703302962 ) ) ;
#837 = CARTESIAN_POINT ( 'NONE',  ( -108.4791267515088435, -173.5000000000000284, -186.7953921478704729 ) ) ;
#838 = DIRECTION ( 'NONE',  ( -0.000000000000000000, 1.000000000000000000, -0.000000000000000000 ) ) ;
#840 = VERTEX_POINT ( 'NONE', #40068 ) ;
#839 = DIRECTION ( 'NONE',  ( 0.000000000000000000, 1.000000000000000000, -0.000000000000000000 ) ) ;
#841 = ORIENTED_EDGE ( 'NONE', *, *, #9249, .F. ) ;
#842 = EDGE_CURVE ( 'NONE', #32383, #1430, #31407, .T. ) ;
#843 = EDGE_CURVE ( 'NONE', #40953, #1071, #11946, .T. ) ;
#844 = CARTESIAN_POINT ( 'NONE',  ( -336.3521761649654422, -123.5000000000000284, 0.000000000000000000 ) ) ;
#845 = CIRCLE ( 'NONE', #30231, 124.9999999999999858 ) ;
#846 = AXIS2_PLACEMENT_3D ( 'NONE', #1945, #25341, #16944 ) ;
#847 = DIRECTION ( 'NONE',  ( 0.000000000000000000, 0.7485107481711089639, 0.6631226582407863113 ) ) ;
#848 = ORIENTED_EDGE ( 'NONE', *, *, #2477, .T. ) ;
#849 = ORIENTED_EDGE ( 'NONE', *, *, #7386, .T. ) ;
#850 = ORIENTED_EDGE ( 'NONE', *, *, #23322, .T. ) ;
#851 = DIRECTION ( 'NONE',  ( 0.000000000000000000, -1.000000000000000000, 0.000000000000000000 ) ) ;
#852 = EDGE_CURVE ( 'NONE', #6390, #47279, #33225, .T. ) ;
#853 = LINE ( 'NONE', #25048, #29478 ) ;
#854 = CARTESIAN_POINT ( 'NONE',  ( -47.47956591500005885, -193.5000000000000000, -0.02963332782254939762 ) ) ;
#855 = ORIENTED_EDGE ( 'NONE', *, *, #4126, .F. ) ;
#856 = ORIENTED_EDGE ( 'NONE', *, *, #47489, .T. ) ;
#857 = EDGE_CURVE ( 'NONE', #42035, #39327, #29921, .T. ) ;
#858 = CARTESIAN_POINT ( 'NONE',  ( -5.113431607746556473, -193.5000000000000000, 117.2365833888819537 ) ) ;
#860 = ORIENTED_EDGE ( 'NONE', *, *, #5508, .F. ) ;
#859 = FACE_OUTER_BOUND ( 'NONE', #28097, .T. ) ;
#861 = EDGE_CURVE ( 'NONE', #38326, #8427, #29287, .T. ) ;
#862 = VECTOR ( 'NONE', #6226, 1000.000000000000000 ) ;
#863 = DIRECTION ( 'NONE',  ( 0.000000000000000000, 0.5680647467311540355, -0.8229838658936575735 ) ) ;
#864 = ORIENTED_EDGE ( 'NONE', *, *, #28901, .F. ) ;
#865 = DIRECTION ( 'NONE',  ( 0.000000000000000000, -0.8854560256532062468, 0.4647231720437755564 ) ) ;
#866 = EDGE_CURVE ( 'NONE', #47840, #37031, #15636, .T. ) ;
#867 = EDGE_LOOP ( 'NONE', ( #46785, #23788, #50525, #40212 ) ) ;
#868 = PLANE ( 'NONE',  #25728 ) ;
#869 = LINE ( 'NONE', #16911, #34690 ) ;
#870 = CARTESIAN_POINT ( 'NONE',  ( -153.7332855749581881, -193.5000000000000000, 67.42819922234390617 ) ) ;
#871 = ORIENTED_EDGE ( 'NONE', *, *, #43423, .T. ) ;
#872 = ORIENTED_EDGE ( 'NONE', *, *, #17504, .T. ) ;
#873 = FACE_OUTER_BOUND ( 'NONE', #29196, .T. ) ;
#874 = DIRECTION ( 'NONE',  ( -0.5586467658036415873, 0.000000000000000000, -0.8294056854502090959 ) ) ;
#875 = VERTEX_POINT ( 'NONE', #37695 ) ;
#876 = CARTESIAN_POINT ( 'NONE',  ( -37.08895481556041318, -183.6283474603465606, 124.4799742258550452 ) ) ;
#877 = CARTESIAN_POINT ( 'NONE',  ( 75.43907105790114542, -193.5000000000000000, -4.503971736580765217 ) ) ;
#878 = ORIENTED_EDGE ( 'NONE', *, *, #33812, .F. ) ;
#879 = FACE_BOUND ( 'NONE', #13817, .T. ) ;
#880 = LINE ( 'NONE', #29514, #15543 ) ;
#881 = AXIS2_PLACEMENT_3D ( 'NONE', #18199, #1900, #2427 ) ;
#882 = VECTOR ( 'NONE', #10796, 1000.000000000000000 ) ;
#883 = ORIENTED_EDGE ( 'NONE', *, *, #5967, .F. ) ;
#884 = PLANE ( 'NONE',  #11452 ) ;
#885 = VERTEX_POINT ( 'NONE', #20900 ) ;
#886 = FACE_BOUND ( 'NONE', #8884, .T. ) ;
#887 = PLANE ( 'NONE',  #37947 ) ;
#888 = EDGE_LOOP ( 'NONE', ( #12030, #10347, #16731, #21899 ) ) ;
#889 = CARTESIAN_POINT ( 'NONE',  ( 46.00000000000000711, 20.00000000000000000, 46.00000000000000000 ) ) ;
#890 = DIRECTION ( 'NONE',  ( 0.000000000000000000, 0.000000000000000000, -1.000000000000000000 ) ) ;
#891 = DIRECTION ( 'NONE',  ( -1.000000000000000000, 0.000000000000000000, 0.000000000000000000 ) ) ;
#892 = DIRECTION ( 'NONE',  ( -0.000000000000000000, -0.1205366802553233113, -0.9927088740980538617 ) ) ;
#893 = EDGE_LOOP ( 'NONE', ( #26823, #18504, #1153, #44757 ) ) ;
#894 = CARTESIAN_POINT ( 'NONE',  ( 39.18328161278952138, -189.7472609257535510, 89.10837311819237527 ) ) ;
#895 = VERTEX_POINT ( 'NONE', #24825 ) ;
#896 = EDGE_CURVE ( 'NONE', #15597, #13271, #36917, .T. ) ;
#897 = ORIENTED_EDGE ( 'NONE', *, *, #18009, .T. ) ;
#898 = VECTOR ( 'NONE', #3315, 1000.000000000000000 ) ;
#899 = LINE ( 'NONE', #29006, #1687 ) ;
#901 = EDGE_LOOP ( 'NONE', ( #1534, #46424, #46077, #38731 ) ) ;
#900 = CARTESIAN_POINT ( 'NONE',  ( -332.3517673607765914, -182.3871109312487420, -4.498567634386014369 ) ) ;
#902 = EDGE_CURVE ( 'NONE', #32022, #7418, #51728, .T. ) ;
#903 = VERTEX_POINT ( 'NONE', #16950 ) ;
#904 = EDGE_CURVE ( 'NONE', #21757, #43156, #32958, .T. ) ;
#905 = DIRECTION ( 'NONE',  ( 0.000000000000000000, 0.000000000000000000, 1.000000000000000000 ) ) ;
#906 = EDGE_CURVE ( 'NONE', #39920, #28294, #29044, .T. ) ;
#907 = ADVANCED_FACE ( 'NONE', ( #17209 ), #33746, .T. ) ;
#908 = CARTESIAN_POINT ( 'NONE',  ( 5.761208793373444359E-16, 50.59471834446340921, -21.36672353920344491 ) ) ;
#909 = ORIENTED_EDGE ( 'NONE', *, *, #36556, .F. ) ;
#910 = CARTESIAN_POINT ( 'NONE',  ( -48.47912675150885065, -177.1207230881787780, 6.938893903907228378E-15 ) ) ;
#911 = EDGE_CURVE ( 'NONE', #19332, #33563, #21674, .T. ) ;
#912 = ORIENTED_EDGE ( 'NONE', *, *, #15930, .T. ) ;
#913 = DIRECTION ( 'NONE',  ( 0.8610436117673514467, 0.000000000000000000, 0.5085311186492273983 ) ) ;
#914 = DIRECTION ( 'NONE',  ( 0.000000000000000000, 0.000000000000000000, -1.000000000000000000 ) ) ;
#915 = VECTOR ( 'NONE', #37349, 1000.000000000000000 ) ;
#916 = EDGE_CURVE ( 'NONE', #37855, #15026, #32709, .T. ) ;
#917 = FACE_OUTER_BOUND ( 'NONE', #10592, .T. ) ;
#918 = FACE_OUTER_BOUND ( 'NONE', #42235, .T. ) ;
#919 = ORIENTED_EDGE ( 'NONE', *, *, #27607, .F. ) ;
#920 = ORIENTED_EDGE ( 'NONE', *, *, #23700, .F. ) ;
#921 = EDGE_CURVE ( 'NONE', #5941, #31777, #13986, .T. ) ;
#923 = EDGE_LOOP ( 'NONE', ( #21309, #38408, #51549, #25066 ) ) ;
#922 = CIRCLE ( 'NONE', #7638, 4.000000000000003553 ) ;
#924 = CARTESIAN_POINT ( 'NONE',  ( -260.0000000000000000, -113.5000000000000142, 60.00000000000001421 ) ) ;
#925 = PLANE ( 'NONE',  #21797 ) ;
#926 = EDGE_CURVE ( 'NONE', #40282, #34006, #49542, .T. ) ;
#927 = DIRECTION ( 'NONE',  ( -1.000000000000000000, 0.000000000000000000, 0.000000000000000000 ) ) ;
#928 = FACE_BOUND ( 'NONE', #50304, .T. ) ;
#929 = DIRECTION ( 'NONE',  ( 0.2348860457809775482, 0.000000000000000000, 0.9720229140804121926 ) ) ;
#930 = ORIENTED_EDGE ( 'NONE', *, *, #25942, .T. ) ;
#931 = ADVANCED_FACE ( 'NONE', ( #48753 ), #49009, .F. ) ;
#932 = ADVANCED_FACE ( 'NONE', ( #28749 ), #41114, .T. ) ;
#933 = EDGE_CURVE ( 'NONE', #20143, #3616, #35758, .T. ) ;
#934 = ORIENTED_EDGE ( 'NONE', *, *, #18476, .T. ) ;
#936 = ORIENTED_EDGE ( 'NONE', *, *, #35799, .T. ) ;
#935 = DIRECTION ( 'NONE',  ( 0.000000000000000000, 0.000000000000000000, 1.000000000000000000 ) ) ;
#937 = ORIENTED_EDGE ( 'NONE', *, *, #49984, .T. ) ;
#938 = AXIS2_PLACEMENT_3D ( 'NONE', #18449, #43124, #7129 ) ;
#939 = PLANE ( 'NONE',  #35045 ) ;
#940 = PLANE ( 'NONE',  #18272 ) ;
#941 = CARTESIAN_POINT ( 'NONE',  ( 0.000000000000000000, -53.50000000000000000, 0.000000000000000000 ) ) ;
#942 = CARTESIAN_POINT ( 'NONE',  ( -365.0000000000001137, -78.50000000000002842, 0.000000000000000000 ) ) ;
#943 = ORIENTED_EDGE ( 'NONE', *, *, #8920, .F. ) ;
#944 = DIRECTION ( 'NONE',  ( 0.000000000000000000, -1.000000000000000000, 0.000000000000000000 ) ) ;
#945 = EDGE_LOOP ( 'NONE', ( #3380, #48657, #41462, #10623 ) ) ;
#946 = EDGE_CURVE ( 'NONE', #41454, #49394, #18152, .T. ) ;
#947 = ORIENTED_EDGE ( 'NONE', *, *, #41395, .F. ) ;
#948 = CARTESIAN_POINT ( 'NONE',  ( -1.771278280434274155, -177.1207230881787780, -115.9455772817710084 ) ) ;
#949 = DIRECTION ( 'NONE',  ( 0.000000000000000000, 0.000000000000000000, 1.000000000000000000 ) ) ;
#950 = VECTOR ( 'NONE', #32180, 1000.000000000000000 ) ;
#951 = DIRECTION ( 'NONE',  ( -0.8610436117673548884, 0.000000000000000000, -0.5085311186492216251 ) ) ;
#952 = DIRECTION ( 'NONE',  ( -0.000000000000000000, 1.000000000000000000, -0.000000000000000000 ) ) ;
#953 = DIRECTION ( 'NONE',  ( 0.000000000000000000, -0.000000000000000000, 1.000000000000000000 ) ) ;
#954 = EDGE_LOOP ( 'NONE', ( #27376, #42178, #35892, #9109 ) ) ;
#955 = FACE_OUTER_BOUND ( 'NONE', #46614, .T. ) ;
#956 = DIRECTION ( 'NONE',  ( 0.000000000000000000, 0.000000000000000000, -1.000000000000000000 ) ) ;
#957 = AXIS2_PLACEMENT_3D ( 'NONE', #26370, #34508, #6419 ) ;
#958 = DIRECTION ( 'NONE',  ( -0.000000000000000000, 1.000000000000000000, 0.000000000000000000 ) ) ;
#959 = FACE_BOUND ( 'NONE', #7939, .T. ) ;
#960 = ORIENTED_EDGE ( 'NONE', *, *, #47532, .T. ) ;
#961 = CARTESIAN_POINT ( 'NONE',  ( 20.10322172534453244, -175.3837268820161057, -103.3076327631962954 ) ) ;
#962 = EDGE_LOOP ( 'NONE', ( #46378, #36787, #38995, #31564 ) ) ;
#963 = CARTESIAN_POINT ( 'NONE',  ( -48.47912675150885065, -177.1207230881787780, 6.938893903907228378E-15 ) ) ;
#964 = EDGE_CURVE ( 'NONE', #13900, #12470, #48136, .T. ) ;
#965 = ORIENTED_EDGE ( 'NONE', *, *, #13376, .F. ) ;
#966 = EDGE_CURVE ( 'NONE', #23416, #47681, #16330, .T. ) ;
#967 = CARTESIAN_POINT ( 'NONE',  ( 36.84288420123323249, -193.5000000000000000, 91.35181687837503262 ) ) ;
#968 = ORIENTED_EDGE ( 'NONE', *, *, #13302, .F. ) ;
#969 = VECTOR ( 'NONE', #7507, 1000.000000000000114 ) ;
#970 = EDGE_CURVE ( 'NONE', #42763, #14296, #20524, .T. ) ;
#971 = EDGE_CURVE ( 'NONE', #12481, #41605, #26539, .T. ) ;
#972 = LINE ( 'NONE', #4397, #37714 ) ;
#973 = AXIS2_PLACEMENT_3D ( 'NONE', #43646, #11589, #36993 ) ;
#975 = VERTEX_POINT ( 'NONE', #15835 ) ;
#974 = CARTESIAN_POINT ( 'NONE',  ( -106.4764934152196645, -193.5000000000000000, -110.7307791902283043 ) ) ;
#976 = LINE ( 'NONE', #17029, #29407 ) ;
#977 = ORIENTED_EDGE ( 'NONE', *, *, #49157, .F. ) ;
#978 = VERTEX_POINT ( 'NONE', #36552 ) ;
#979 = ORIENTED_EDGE ( 'NONE', *, *, #41691, .T. ) ;
#980 = DIRECTION ( 'NONE',  ( -0.000000000000000000, -1.000000000000000000, 0.000000000000000000 ) ) ;
#981 = CARTESIAN_POINT ( 'NONE',  ( -339.1964088526558498, -137.3729703655840524, -58.37414404713467064 ) ) ;
#982 = ADVANCED_FACE ( 'NONE', ( #8191 ), #44714, .F. ) ;
#983 = ORIENTED_EDGE ( 'NONE', *, *, #25650, .T. ) ;
#984 = CARTESIAN_POINT ( 'NONE',  ( -46.00000000000000711, 20.00000000000000000, 51.00000000000000000 ) ) ;
#985 = CARTESIAN_POINT ( 'NONE',  ( -49.47517659412406488, -175.3837268820161057, -0.08879589532293878651 ) ) ;
#986 = CYLINDRICAL_SURFACE ( 'NONE', #16278, 125.0000000000000000 ) ;
#987 = VECTOR ( 'NONE', #1151, 1000.000000000000000 ) ;
#988 = VECTOR ( 'NONE', #34553, 1000.000000000000000 ) ;
#989 = EDGE_CURVE ( 'NONE', #1891, #26506, #4719, .T. ) ;
#990 = VECTOR ( 'NONE', #16883, 1000.000000000000000 ) ;
#991 = CARTESIAN_POINT ( 'NONE',  ( -48.24424070572786860, -193.5000000000000000, -0.9720229140804037549 ) ) ;
#992 = CARTESIAN_POINT ( 'NONE',  ( -70.24606818074174441, -175.3837268820161057, -122.0745693923548885 ) ) ;
#993 = VERTEX_POINT ( 'NONE', #554 ) ;
#996 = ORIENTED_EDGE ( 'NONE', *, *, #9660, .T. ) ;
#995 = DIRECTION ( 'NONE',  ( -1.000000000000000000, -0.000000000000000000, -0.000000000000000000 ) ) ;
#994 = CARTESIAN_POINT ( 'NONE',  ( -46.06708674231131084, -177.1207230881787780, -124.9767260852756863 ) ) ;
#997 = EDGE_LOOP ( 'NONE', ( #1624, #5799, #27642, #44383 ) ) ;
#998 = CARTESIAN_POINT ( 'NONE',  ( -48.47912675150885065, -175.3837268820161057, 6.938893903907228378E-15 ) ) ;
#999 = EDGE_LOOP ( 'NONE', ( #14345, #29915, #10914, #12170 ) ) ;
#1000 = CARTESIAN_POINT ( 'NONE',  ( -336.3521761649654422, -77.59233547837267508, 37.15394033962009246 ) ) ;
#1001 = VERTEX_POINT ( 'NONE', #8705 ) ;
#1002 = CARTESIAN_POINT ( 'NONE',  ( -72.96029774493611342, -193.5000000000000000, 122.5792489240759409 ) ) ;
#1003 = DIRECTION ( 'NONE',  ( 0.000000000000000000, -0.7485107481711046340, -0.6631226582407911962 ) ) ;
#1004 = ORIENTED_EDGE ( 'NONE', *, *, #33599, .F. ) ;
#1005 = CARTESIAN_POINT ( 'NONE',  ( -172.7479958471413966, -177.1207230881787780, -13.49993235881363418 ) ) ;
#1006 = ORIENTED_EDGE ( 'NONE', *, *, #3159, .T. ) ;
#1007 = AXIS2_PLACEMENT_3D ( 'NONE', #42136, #33499, #37944 ) ;
#1008 = ORIENTED_EDGE ( 'NONE', *, *, #2527, .F. ) ;
#1009 = LINE ( 'NONE', #40954, #47226 ) ;
#1010 = AXIS2_PLACEMENT_3D ( 'NONE', #24316, #19851, #28247 ) ;
#1012 = AXIS2_PLACEMENT_3D ( 'NONE', #3323, #35369, #51682 ) ;
#1011 = CARTESIAN_POINT ( 'NONE',  ( -1.578537454945990293, -183.6283474603465606, 114.7887733785766926 ) ) ;
#1013 = LINE ( 'NONE', #49120, #20489 ) ;
#1014 = CARTESIAN_POINT ( 'NONE',  ( -154.2693405752510500, -189.7472609257535510, 66.58401203837827609 ) ) ;
#1015 = ORIENTED_EDGE ( 'NONE', *, *, #49773, .T. ) ;
#1016 = DIRECTION ( 'NONE',  ( -0.000000000000000000, -0.6631226582407989678, -0.7485107481710977506 ) ) ;
#1017 = DIRECTION ( 'NONE',  ( 0.000000000000000000, 0.000000000000000000, -1.000000000000000000 ) ) ;
#1018 = CARTESIAN_POINT ( 'NONE',  ( 21.49274850782854074, -193.5000000000000000, -103.5805805771126700 ) ) ;
#1019 = DIRECTION ( 'NONE',  ( 0.000000000000000000, -1.000000000000000000, 0.000000000000000000 ) ) ;
#1020 = DIRECTION ( 'NONE',  ( 0.000000000000000000, 0.000000000000000000, 1.000000000000000000 ) ) ;
#1021 = CARTESIAN_POINT ( 'NONE',  ( -336.3521761649654422, -136.0347666902908372, 57.67619951860663718 ) ) ;
#1022 = ORIENTED_EDGE ( 'NONE', *, *, #4950, .T. ) ;
#1023 = AXIS2_PLACEMENT_3D ( 'NONE', #28600, #25706, #21511 ) ;
#1024 = DIRECTION ( 'NONE',  ( 0.000000000000000000, -1.000000000000000000, 0.000000000000000000 ) ) ;
#1025 = LINE ( 'NONE', #25468, #35362 ) ;
#1026 = ORIENTED_EDGE ( 'NONE', *, *, #19388, .F. ) ;
#1027 = EDGE_CURVE ( 'NONE', #12239, #8561, #37458, .T. ) ;
#1028 = ORIENTED_EDGE ( 'NONE', *, *, #30753, .T. ) ;
#1029 = ORIENTED_EDGE ( 'NONE', *, *, #9171, .T. ) ;
#1030 = CIRCLE ( 'NONE', #8567, 4.999999999999997335 ) ;
#1031 = PLANE ( 'NONE',  #16725 ) ;
#1032 = LINE ( 'NONE', #44675, #32050 ) ;
#1033 = CARTESIAN_POINT ( 'NONE',  ( -336.3521761649653854, -167.3116148657362032, 40.99441916720376611 ) ) ;
#1034 = DIRECTION ( 'NONE',  ( -0.000000000000000000, 1.000000000000000000, 0.000000000000000000 ) ) ;
#1035 = VERTEX_POINT ( 'NONE', #35777 ) ;
#1036 = DIRECTION ( 'NONE',  ( -1.000000000000000000, -0.000000000000000000, -0.000000000000000000 ) ) ;
#1037 = CARTESIAN_POINT ( 'NONE',  ( -48.47912675150885065, -132.5479369270331915, -14.99999999999999289 ) ) ;
#1038 = VECTOR ( 'NONE', #4734, 1000.000000000000227 ) ;
#1039 = EDGE_LOOP ( 'NONE', ( #32156, #50027, #34356, #41255 ) ) ;
#1040 = AXIS2_PLACEMENT_3D ( 'NONE', #5163, #8318, #16466 ) ;
#1041 = DIRECTION ( 'NONE',  ( 0.000000000000000000, 0.000000000000000000, 1.000000000000000000 ) ) ;
#1042 = ORIENTED_EDGE ( 'NONE', *, *, #34030, .T. ) ;
#1043 = PRODUCT_DEFINITION ( 'UNKNOWN', '', #41839, #39510 ) ;
#1044 = DIRECTION ( 'NONE',  ( -0.9960498426152177842, 0.000000000000000000, 0.08879589532292482545 ) ) ;
#1045 = VECTOR ( 'NONE', #12771, 1000.000000000000227 ) ;
#1046 = VECTOR ( 'NONE', #42393, 999.9999999999998863 ) ;
#1047 = ORIENTED_EDGE ( 'NONE', *, *, #10383, .F. ) ;
#1048 = EDGE_CURVE ( 'NONE', #47759, #11883, #36044, .T. ) ;
#1049 = DIRECTION ( 'NONE',  ( 1.000000000000000000, -0.000000000000000000, -0.000000000000000000 ) ) ;
#1050 = CARTESIAN_POINT ( 'NONE',  ( 0.000000000000000000, -66.21443277186293130, -14.11962419296594362 ) ) ;
#1051 = CARTESIAN_POINT ( 'NONE',  ( -330.4913330509368166, -138.1050951016791544, -57.16590939599326049 ) ) ;
#1054 = ORIENTED_EDGE ( 'NONE', *, *, #47532, .F. ) ;
#1053 = DIRECTION ( 'NONE',  ( 0.000000000000000000, -0.9927088740980526405, 0.1205366802553337890 ) ) ;
#1052 = CARTESIAN_POINT ( 'NONE',  ( 60.90550954139437323, -175.3837268820161057, 60.49794494914087295 ) ) ;
#1055 = CARTESIAN_POINT ( 'NONE',  ( -330.4913330509368166, -162.9984922102926532, -43.83057281297441676 ) ) ;
#1056 = ORIENTED_EDGE ( 'NONE', *, *, #35004, .T. ) ;
#1057 = CARTESIAN_POINT ( 'NONE',  ( -155.9608607592037401, -183.6283474603465606, 63.81752780153057358 ) ) ;
#1058 = AXIS2_PLACEMENT_3D ( 'NONE', #5694, #20664, #36698 ) ;
#1059 = DIRECTION ( 'NONE',  ( -0.000000000000000000, 1.000000000000000000, 0.000000000000000000 ) ) ;
#1060 = ORIENTED_EDGE ( 'NONE', *, *, #36657, .T. ) ;
#1061 = EDGE_CURVE ( 'NONE', #49231, #23542, #43, .T. ) ;
#1062 = DIRECTION ( 'NONE',  ( 0.000000000000000000, -1.000000000000000000, 0.000000000000000000 ) ) ;
#1064 = CYLINDRICAL_SURFACE ( 'NONE', #42444, 5.000000000000001776 ) ;
#1063 = DIRECTION ( 'NONE',  ( 0.000000000000000000, 0.000000000000000000, 1.000000000000000000 ) ) ;
#1065 = EDGE_LOOP ( 'NONE', ( #26857, #9484, #32742, #48666 ) ) ;
#1066 = CIRCLE ( 'NONE', #196, 14.00000000000001066 ) ;
#1067 = CARTESIAN_POINT ( 'NONE',  ( -168.9345475356665247, -193.5000000000000000, 29.43839964798726427 ) ) ;
#1068 = CARTESIAN_POINT ( 'NONE',  ( -339.1964088526558498, -64.50000000000000000, -0.5000000000000457412 ) ) ;
#1069 = DIRECTION ( 'NONE',  ( -0.000000000000000000, -1.000000000000000000, 0.000000000000000000 ) ) ;
#1070 = ADVANCED_FACE ( 'NONE', ( #24224 ), #43672, .T. ) ;
#1071 = VERTEX_POINT ( 'NONE', #12382 ) ;
#1072 = LINE ( 'NONE', #4247, #48477 ) ;
#1073 = SURFACE_SIDE_STYLE ('',( #5041 ) ) ;
#1074 = CARTESIAN_POINT ( 'NONE',  ( -171.2399149993172500, -189.7472609257535510, -17.48697739784461547 ) ) ;
#1075 = DIRECTION ( 'NONE',  ( 1.000000000000000000, 0.000000000000000000, -0.000000000000000000 ) ) ;
#1076 = EDGE_LOOP ( 'NONE', ( #42228, #13718, #8425, #36051 ) ) ;
#1077 = VECTOR ( 'NONE', #10028, 1000.000000000000114 ) ;
#1078 = LINE ( 'NONE', #17655, #267 ) ;
#1079 = VECTOR ( 'NONE', #40641, 1000.000000000000000 ) ;
#1080 = PLANE ( 'NONE',  #27310 ) ;
#1081 = EDGE_CURVE ( 'NONE', #19973, #15758, #3891, .T. ) ;
#1082 = FACE_OUTER_BOUND ( 'NONE', #774, .T. ) ;
#1083 = EDGE_LOOP ( 'NONE', ( #33373, #19923, #40663, #49967 ) ) ;
#1084 = AXIS2_PLACEMENT_3D ( 'NONE', #4869, #16702, #32704 ) ;
#1085 = FACE_OUTER_BOUND ( 'NONE', #1756, .T. ) ;
#1086 = DIRECTION ( 'NONE',  ( -0.000000000000000000, 1.000000000000000000, -0.000000000000000000 ) ) ;
#1087 = CARTESIAN_POINT ( 'NONE',  ( -172.6359455740846442, -177.1207230881787780, -14.49428645563791562 ) ) ;
#1088 = CARTESIAN_POINT ( 'NONE',  ( -47.64924157374594671, -193.5000000000000000, 124.9972451320097377 ) ) ;
#1089 = EDGE_CURVE ( 'NONE', #49077, #5683, #4772, .T. ) ;
#1090 = DIRECTION ( 'NONE',  ( 0.000000000000000000, 0.000000000000000000, 1.000000000000000000 ) ) ;
#1091 = ADVANCED_FACE ( 'NONE', ( #36295 ), #4248, .F. ) ;
#1092 = DIRECTION ( 'NONE',  ( -0.9929810960135169173, 0.000000000000000000, -0.1182731709213660498 ) ) ;
#1093 = CARTESIAN_POINT ( 'NONE',  ( 36.10886851198522152, -177.1207230881787780, 92.03190238880812046 ) ) ;
#1095 = VERTEX_POINT ( 'NONE', #48668 ) ;
#1094 = DIRECTION ( 'NONE',  ( 0.000000000000000000, 0.000000000000000000, 1.000000000000000000 ) ) ;
#1096 = AXIS2_PLACEMENT_3D ( 'NONE', #11928, #27966, #43997 ) ;
#1097 = ORIENTED_EDGE ( 'NONE', *, *, #46194, .T. ) ;
#1098 = DIRECTION ( 'NONE',  ( -0.1476465640024779702, 0.000000000000000000, -0.9890401873221644768 ) ) ;
#1099 = CIRCLE ( 'NONE', #43897, 125.0000000000000000 ) ;
#1100 = CARTESIAN_POINT ( 'NONE',  ( -336.3521761649654422, -105.0395444947681369, -56.09938080879045685 ) ) ;
#1102 = ORIENTED_EDGE ( 'NONE', *, *, #37849, .T. ) ;
#1101 = DIRECTION ( 'NONE',  ( 0.000000000000000000, -1.000000000000000000, 0.000000000000000000 ) ) ;
#1103 = EDGE_LOOP ( 'NONE', ( #16367, #2047, #5944, #42627, #29836, #15506, #24590, #45361, #42114, #27008, #14441, #17020 ) ) ;
#1104 = EDGE_LOOP ( 'NONE', ( #39856, #48441, #16840, #32095 ) ) ;
#1105 = EDGE_CURVE ( 'NONE', #9161, #6831, #824, .T. ) ;
#1106 = PLANE ( 'NONE',  #22538 ) ;
#1107 = DIRECTION ( 'NONE',  ( -0.000000000000000000, -0.2393156642875615969, -0.9709418174260511236 ) ) ;
#1108 = CARTESIAN_POINT ( 'NONE',  ( -48.47912675150885065, -183.6283474603465606, 1.000000000000006883 ) ) ;
#1109 = ORIENTED_EDGE ( 'NONE', *, *, #6562, .F. ) ;
#1110 = DIRECTION ( 'NONE',  ( 0.000000000000000000, 0.000000000000000000, -1.000000000000000000 ) ) ;
#1112 = ORIENTED_EDGE ( 'NONE', *, *, #36486, .T. ) ;
#1111 = DIRECTION ( 'NONE',  ( -0.000000000000000000, 1.000000000000000000, 0.000000000000000000 ) ) ;
#1113 = AXIS2_PLACEMENT_3D ( 'NONE', #40879, #12244, #40608 ) ;
#1114 = CARTESIAN_POINT ( 'NONE',  ( 0.000000000000000000, -89.98417994286192823, -48.55604808772582004 ) ) ;
#1115 = EDGE_LOOP ( 'NONE', ( #13335, #18984, #15871, #12888 ) ) ;
#1116 = DIRECTION ( 'NONE',  ( -0.000000000000000000, 1.000000000000000000, 0.000000000000000000 ) ) ;
#1117 = ORIENTED_EDGE ( 'NONE', *, *, #17462, .T. ) ;
#1118 = AXIS2_PLACEMENT_3D ( 'NONE', #44291, #51657, #20104 ) ;
#1119 = DIRECTION ( 'NONE',  ( -0.5338233779647887367, 0.000000000000000000, -0.8455960035018273979 ) ) ;
#1120 = CARTESIAN_POINT ( 'NONE',  ( -280.0000000000000000, -63.50000000000000000, 60.00000000000000711 ) ) ;
#1121 = DIRECTION ( 'NONE',  ( 0.6068001458185890984, 0.000000000000000000, 0.7948544414133565938 ) ) ;
#1122 = EDGE_LOOP ( 'NONE', ( #3944, #25050, #48076, #48134 ) ) ;
#1123 = ORIENTED_EDGE ( 'NONE', *, *, #4358, .F. ) ;
#1124 = DIRECTION ( 'NONE',  ( -0.2920567706369628924, 0.000000000000000000, -0.9564009842765264224 ) ) ;
#1125 = LINE ( 'NONE', #21898, #22530 ) ;
#1126 = VERTEX_POINT ( 'NONE', #22089 ) ;
#1127 = DIRECTION ( 'NONE',  ( 0.000000000000000000, 1.000000000000000000, 0.000000000000000000 ) ) ;
#1128 = VECTOR ( 'NONE', #19899, 1000.000000000000000 ) ;
#1129 = DIRECTION ( 'NONE',  ( 0.000000000000000000, 0.000000000000000000, 1.000000000000000000 ) ) ;
#1130 = EDGE_CURVE ( 'NONE', #12681, #24651, #10601, .T. ) ;
#1131 = ADVANCED_FACE ( 'NONE', ( #17398 ), #13432, .T. ) ;
#1132 = ORIENTED_EDGE ( 'NONE', *, *, #23366, .T. ) ;
#1133 = CARTESIAN_POINT ( 'NONE',  ( -336.3521761649654422, -87.28260048324005993, 47.83617848703422482 ) ) ;
#1135 = AXIS2_PLACEMENT_3D ( 'NONE', #38655, #26314, #14244 ) ;
#1134 = DIRECTION ( 'NONE',  ( 0.000000000000000000, 0.000000000000000000, 1.000000000000000000 ) ) ;
#1136 = ORIENTED_EDGE ( 'NONE', *, *, #6330, .F. ) ;
#1137 = PLANE ( 'NONE',  #20696 ) ;
#1138 = ORIENTED_EDGE ( 'NONE', *, *, #36258, .F. ) ;
#1139 = CARTESIAN_POINT ( 'NONE',  ( -84.82349129030166068, -193.5000000000000000, -119.5996955107802222 ) ) ;
#1140 = CARTESIAN_POINT ( 'NONE',  ( -332.3517673607765914, -158.3591674452439122, -47.62880233550485087 ) ) ;
#1141 = MANIFOLD_SOLID_BREP ( 'Cut-Extrude1', #17058 ) ;
#1142 = ORIENTED_EDGE ( 'NONE', *, *, #1857, .F. ) ;
#1143 = PLANE ( 'NONE',  #12243 ) ;
#1144 = DIRECTION ( 'NONE',  ( 0.000000000000000000, 0.000000000000000000, -1.000000000000000000 ) ) ;
#1145 = LINE ( 'NONE', #9828, #29943 ) ;
#1146 = ADVANCED_FACE ( 'NONE', ( #41812 ), #1852, .T. ) ;
#1147 = AXIS2_PLACEMENT_3D ( 'NONE', #10818, #4415, #40654 ) ;
#1148 = CARTESIAN_POINT ( 'NONE',  ( -336.3521761649654422, -86.34605966037949543, -45.90766452162698386 ) ) ;
#1149 = EDGE_CURVE ( 'NONE', #43162, #33480, #21057, .T. ) ;
#1150 = ORIENTED_EDGE ( 'NONE', *, *, #42462, .T. ) ;
#1151 = DIRECTION ( 'NONE',  ( 0.4031234292879730674, 0.000000000000000000, -0.9151456172430181280 ) ) ;
#1152 = ORIENTED_EDGE ( 'NONE', *, *, #33748, .T. ) ;
#1153 = ORIENTED_EDGE ( 'NONE', *, *, #48129, .F. ) ;
#1154 = EDGE_CURVE ( 'NONE', #5750, #45751, #25513, .T. ) ;
#1155 = DIRECTION ( 'NONE',  ( -0.000000000000000000, 1.156482317317871232E-16, 1.000000000000000000 ) ) ;
#1157 = ORIENTED_EDGE ( 'NONE', *, *, #23110, .F. ) ;
#1156 = DIRECTION ( 'NONE',  ( -0.000000000000000000, 1.000000000000000000, -0.000000000000000000 ) ) ;
#1158 = EDGE_CURVE ( 'NONE', #13843, #41304, #13691, .T. ) ;
#1159 = VERTEX_POINT ( 'NONE', #10021 ) ;
#1160 = DIRECTION ( 'NONE',  ( 0.000000000000000000, 0.000000000000000000, -1.000000000000000000 ) ) ;
#1161 = DIRECTION ( 'NONE',  ( 1.000000000000000000, -0.000000000000000000, -0.000000000000000000 ) ) ;
#1162 = LINE ( 'NONE', #12987, #20148 ) ;
#1163 = VERTEX_POINT ( 'NONE', #29709 ) ;
#1164 = DIRECTION ( 'NONE',  ( 0.000000000000000000, 0.000000000000000000, -1.000000000000000000 ) ) ;
#1165 = EDGE_LOOP ( 'NONE', ( #35019, #7711, #18752, #10228 ) ) ;
#1166 = CARTESIAN_POINT ( 'NONE',  ( -48.98765787015808115, -175.3837268820161057, 0.8610436117673582190 ) ) ;
#1167 = CARTESIAN_POINT ( 'NONE',  ( -170.0000000000000284, -115.7896721143442278, 18.45401972188388839 ) ) ;
#1168 = AXIS2_PLACEMENT_3D ( 'NONE', #5085, #48965, #865 ) ;
#1169 = CIRCLE ( 'NONE', #45683, 125.0000000000000000 ) ;
#1170 = PLANE ( 'NONE',  #26072 ) ;
#1171 = DIRECTION ( 'NONE',  ( 0.000000000000000000, -1.000000000000000000, 0.000000000000000000 ) ) ;
#1172 = ORIENTED_EDGE ( 'NONE', *, *, #26251, .T. ) ;
#1173 = ORIENTED_EDGE ( 'NONE', *, *, #32356, .T. ) ;
#1174 = CIRCLE ( 'NONE', #7886, 125.0000000000000000 ) ;
#1175 = ORIENTED_EDGE ( 'NONE', *, *, #16877, .T. ) ;
#1176 = CARTESIAN_POINT ( 'NONE',  ( -15.81236726369127155, -183.6283474603465606, -120.6560517527615559 ) ) ;
#1177 = DIRECTION ( 'NONE',  ( -0.8124868780056863082, 0.000000000000000000, 0.5829794791144649047 ) ) ;
#1178 = CARTESIAN_POINT ( 'NONE',  ( -151.9915035862630646, -183.6283474603465606, 70.07273251429430161 ) ) ;
#1179 = DIRECTION ( 'NONE',  ( 0.000000000000000000, 1.000000000000000000, 0.000000000000000000 ) ) ;
#1180 = ORIENTED_EDGE ( 'NONE', *, *, #48158, .T. ) ;
#1181 = AXIS2_PLACEMENT_3D ( 'NONE', #46702, #38019, #2299 ) ;
#1182 = ORIENTED_EDGE ( 'NONE', *, *, #51706, .F. ) ;
#1184 = ORIENTED_EDGE ( 'NONE', *, *, #26596, .T. ) ;
#1183 = CARTESIAN_POINT ( 'NONE',  ( -339.1964088526558498, -179.7763290203209863, -20.80804632820157352 ) ) ;
#1185 = EDGE_LOOP ( 'NONE', ( #30507, #5255 ) ) ;
#1186 = CARTESIAN_POINT ( 'NONE',  ( 28.02885774092381865, -193.5000000000000000, 98.85104101073331151 ) ) ;
#1187 = LINE ( 'NONE', #5418, #4841 ) ;
#1188 = EDGE_CURVE ( 'NONE', #36786, #30970, #9749, .T. ) ;
#1189 = CARTESIAN_POINT ( 'NONE',  ( 18.00181100848372751, -183.6283474603465606, -105.8550183720733742 ) ) ;
#1190 = EDGE_CURVE ( 'NONE', #42645, #40857, #17379, .T. ) ;
#1191 = EDGE_CURVE ( 'NONE', #36985, #10779, #37494, .T. ) ;
#1192 = DIRECTION ( 'NONE',  ( 0.7378332790417285736, 0.000000000000000000, -0.6749830015182091136 ) ) ;
#1193 = ORIENTED_EDGE ( 'NONE', *, *, #96, .F. ) ;
#1194 = DIRECTION ( 'NONE',  ( -0.000000000000000000, 1.000000000000000000, -0.000000000000000000 ) ) ;
#1195 = EDGE_LOOP ( 'NONE', ( #16137, #29792, #13880, #18999 ) ) ;
#1196 = ADVANCED_FACE ( 'NONE', ( #1614 ), #13179, .T. ) ;
#1197 = ORIENTED_EDGE ( 'NONE', *, *, #13985, .T. ) ;
#1198 = PLANE ( 'NONE',  #3612 ) ;
#1199 = EDGE_CURVE ( 'NONE', #48562, #22978, #48420, .T. ) ;
#1200 = FACE_OUTER_BOUND ( 'NONE', #51358, .T. ) ;
#1201 = ORIENTED_EDGE ( 'NONE', *, *, #11281, .F. ) ;
#1202 = ADVANCED_FACE ( 'NONE', ( #12902 ), #28923, .F. ) ;
#1203 = VECTOR ( 'NONE', #7902, 1000.000000000000114 ) ;
#1204 = VECTOR ( 'NONE', #27394, 1000.000000000000000 ) ;
#1205 = CARTESIAN_POINT ( 'NONE',  ( -339.1964088526558498, -64.99044476834235695, 7.608018572112245970 ) ) ;
#1206 = CARTESIAN_POINT ( 'NONE',  ( -330.4913330509368166, -102.6919536717981742, -56.27632902032085838 ) ) ;
#1207 = CARTESIAN_POINT ( 'NONE',  ( -336.3521761649654422, -174.5186198893880771, 29.74944317415823392 ) ) ;
#1208 = EDGE_CURVE ( 'NONE', #14314, #3375, #7100, .T. ) ;
#1209 = DIRECTION ( 'NONE',  ( -0.000000000000000000, 0.9350162426854194964, 0.3546048870425235200 ) ) ;
#1210 = CARTESIAN_POINT ( 'NONE',  ( -332.3517673607765914, -164.5945333327934463, -42.41660376256285048 ) ) ;
#1211 = VECTOR ( 'NONE', #1937, 1000.000000000000000 ) ;
#1212 = ADVANCED_FACE ( 'NONE', ( #27051 ), #30739, .T. ) ;
#1213 = DIRECTION ( 'NONE',  ( -0.000000000000000000, 1.000000000000000000, -0.000000000000000000 ) ) ;
#1214 = DIRECTION ( 'NONE',  ( 0.000000000000000000, 0.000000000000000000, 1.000000000000000000 ) ) ;
#1215 = ORIENTED_EDGE ( 'NONE', *, *, #12852, .F. ) ;
#1216 = EDGE_CURVE ( 'NONE', #37425, #42355, #6840, .T. ) ;
#1217 = CARTESIAN_POINT ( 'NONE',  ( -106.2948367055610106, -193.5000000000000000, -110.8257356506552185 ) ) ;
#1218 = ORIENTED_EDGE ( 'NONE', *, *, #43325, .F. ) ;
#1219 = DIRECTION ( 'NONE',  ( 0.8610436117673585521, 0.000000000000000000, -0.5085311186492154079 ) ) ;
#1220 = ADVANCED_FACE ( 'NONE', ( #2388 ), #51001, .T. ) ;
#1221 = ORIENTED_EDGE ( 'NONE', *, *, #11832, .F. ) ;
#1222 = FACE_OUTER_BOUND ( 'NONE', #32568, .T. ) ;
#1223 = VECTOR ( 'NONE', #24581, 1000.000000000000000 ) ;
#1224 = ORIENTED_EDGE ( 'NONE', *, *, #4058, .T. ) ;
#1225 = DIRECTION ( 'NONE',  ( 0.000000000000000000, -0.000000000000000000, -1.000000000000000000 ) ) ;
#1226 = CARTESIAN_POINT ( 'NONE',  ( -260.0000000000000000, -113.5000000000000142, -60.00000000000001421 ) ) ;
#1228 = VERTEX_POINT ( 'NONE', #26542 ) ;
#1227 = DIRECTION ( 'NONE',  ( -0.000000000000000000, 0.9709418174260553425, 0.2393156642875449158 ) ) ;
#1229 = FACE_BOUND ( 'NONE', #16915, .T. ) ;
#1230 = EDGE_CURVE ( 'NONE', #41535, #24657, #42580, .T. ) ;
#1231 = ORIENTED_EDGE ( 'NONE', *, *, #40377, .F. ) ;
#1232 = ORIENTED_EDGE ( 'NONE', *, *, #19726, .F. ) ;
#1233 = ORIENTED_EDGE ( 'NONE', *, *, #37875, .T. ) ;
#1234 = CARTESIAN_POINT ( 'NONE',  ( -88.78924379339714790, -193.5000000000000000, -118.3219948448692520 ) ) ;
#1235 = LINE ( 'NONE', #25936, #47834 ) ;
#1236 = VECTOR ( 'NONE', #14406, 1000.000000000000227 ) ;
#1237 = ORIENTED_EDGE ( 'NONE', *, *, #23580, .T. ) ;
#1238 = VECTOR ( 'NONE', #39954, 1000.000000000000000 ) ;
#1239 = PLANE ( 'NONE',  #145 ) ;
#1240 = DIRECTION ( 'NONE',  ( 0.9785564922995060311, 0.000000000000000000, -0.2059786187410889424 ) ) ;
#1241 = EDGE_LOOP ( 'NONE', ( #25430, #19183, #25852, #22627 ) ) ;
#1242 = VECTOR ( 'NONE', #4530, 1000.000000000000000 ) ;
#1243 = VECTOR ( 'NONE', #46234, 1000.000000000000000 ) ;
#1244 = DIRECTION ( 'NONE',  ( 0.000000000000000000, 0.000000000000000000, 1.000000000000000000 ) ) ;
#1245 = EDGE_CURVE ( 'NONE', #23736, #38723, #34435, .T. ) ;
#1246 = CARTESIAN_POINT ( 'NONE',  ( 5.542374969221969039, -193.5000000000000000, 112.7238987608088365 ) ) ;
#1247 = EDGE_LOOP ( 'NONE', ( #17224, #10364, #28770, #36287 ) ) ;
#1250 = ORIENTED_EDGE ( 'NONE', *, *, #49274, .T. ) ;
#1249 = DIRECTION ( 'NONE',  ( -1.000000000000000000, 0.000000000000000000, 0.000000000000000000 ) ) ;
#1248 = DIRECTION ( 'NONE',  ( 0.000000000000000000, -0.000000000000000000, 1.000000000000000000 ) ) ;
#1251 = VERTEX_POINT ( 'NONE', #10783 ) ;
#1252 = VECTOR ( 'NONE', #11527, 1000.000000000000000 ) ;
#1253 = ORIENTED_EDGE ( 'NONE', *, *, #24527, .T. ) ;
#1254 = CARTESIAN_POINT ( 'NONE',  ( 141.7825277784304205, -213.5000000000000000, 41.45482488023466772 ) ) ;
#1255 = VECTOR ( 'NONE', #11183, 1000.000000000000000 ) ;
#1256 = ORIENTED_EDGE ( 'NONE', *, *, #9263, .T. ) ;
#1257 = EDGE_CURVE ( 'NONE', #33644, #3411, #30240, .T. ) ;
#1258 = DIRECTION ( 'NONE',  ( 0.9785564922995032555, 0.000000000000000000, 0.2059786187411021818 ) ) ;
#1259 = ADVANCED_FACE ( 'NONE', ( #22618 ), #14476, .T. ) ;
#1260 = ADVANCED_FACE ( 'NONE', ( #11024 ), #43360, .T. ) ;
#1261 = CARTESIAN_POINT ( 'NONE',  ( -339.1964088526558498, -84.75001853787809125, 44.49369547121489887 ) ) ;
#1262 = ORIENTED_EDGE ( 'NONE', *, *, #23043, .T. ) ;
#1263 = DIRECTION ( 'NONE',  ( 0.000000000000000000, -1.000000000000000000, 0.000000000000000000 ) ) ;
#1264 = AXIS2_PLACEMENT_3D ( 'NONE', #4825, #20847, #25057 ) ;
#1265 = ORIENTED_EDGE ( 'NONE', *, *, #8650, .T. ) ;
#1266 = EDGE_CURVE ( 'NONE', #28257, #8870, #18418, .T. ) ;
#1267 = CIRCLE ( 'NONE', #16395, 125.0000000000000000 ) ;
#1268 = ORIENTED_EDGE ( 'NONE', *, *, #14115, .F. ) ;
#1269 = LINE ( 'NONE', #1786, #32901 ) ;
#1270 = DIRECTION ( 'NONE',  ( 0.000000000000000000, -7.725301879683381348E-14, -1.000000000000000000 ) ) ;
#1271 = CARTESIAN_POINT ( 'NONE',  ( 0.000000000000000000, -84.37576316379256980, 44.16213414209452992 ) ) ;
#1272 = CARTESIAN_POINT ( 'NONE',  ( -152.0588566364588132, -193.5000000000000000, -68.17212999877146729 ) ) ;
#1273 = ORIENTED_EDGE ( 'NONE', *, *, #35449, .T. ) ;
#1274 = DIRECTION ( 'NONE',  ( 1.000000000000000000, -0.000000000000000000, -0.000000000000000000 ) ) ;
#1275 = PRODUCT_CONTEXT ( 'NONE', #38416, 'mechanical' ) ;
#1276 = DIRECTION ( 'NONE',  ( 1.000000000000000000, -0.000000000000000000, -0.000000000000000000 ) ) ;
#1277 = CARTESIAN_POINT ( 'NONE',  ( -49.21696003055058810, -177.1207230881787780, 0.6749830015182108900 ) ) ;
#1278 = DIRECTION ( 'NONE',  ( 1.000000000000000000, 8.465038975556407387E-17, 2.086444717177515993E-17 ) ) ;
#1279 = CARTESIAN_POINT ( 'NONE',  ( -336.3521761649654422, -152.3639871485048900, -51.48334306143194539 ) ) ;
#1280 = CARTESIAN_POINT ( 'NONE',  ( -78.00521078983982193, -189.7472609257535510, 121.4627941443857111 ) ) ;
#1281 = ORIENTED_EDGE ( 'NONE', *, *, #36487, .T. ) ;
#1282 = AXIS2_PLACEMENT_3D ( 'NONE', #5837, #40755, #21323 ) ;
#1283 = ADVANCED_FACE ( 'NONE', ( #31006 ), #43091, .F. ) ;
#1284 = CIRCLE ( 'NONE', #23934, 125.0000000000000000 ) ;
#1285 = AXIS2_PLACEMENT_3D ( 'NONE', #35926, #11741, #11484 ) ;
#1286 = CYLINDRICAL_SURFACE ( 'NONE', #37013, 125.0000000000000000 ) ;
#1287 = ADVANCED_FACE ( 'NONE', ( #10509 ), #34685, .T. ) ;
#1288 = DIRECTION ( 'NONE',  ( -0.000000000000000000, 1.000000000000000000, -0.000000000000000000 ) ) ;
#1289 = ORIENTED_EDGE ( 'NONE', *, *, #2143, .F. ) ;
#1290 = DIRECTION ( 'NONE',  ( 0.9027978299657416494, 0.000000000000000000, 0.4300652022765245608 ) ) ;
#1291 = EDGE_LOOP ( 'NONE', ( #28690, #31738, #8081, #30017 ) ) ;
#1292 = AXIS2_PLACEMENT_3D ( 'NONE', #20681, #31736, #20159 ) ;
#1293 = EDGE_CURVE ( 'NONE', #32812, #28636, #36675, .T. ) ;
#1294 = LINE ( 'NONE', #1811, #23423 ) ;
#1295 = CARTESIAN_POINT ( 'NONE',  ( 41.41233698655025108, -183.6283474603465606, 86.85922373029362120 ) ) ;
#1296 = VECTOR ( 'NONE', #32739, 1000.000000000000000 ) ;
#1297 = PLANE ( 'NONE',  #40483 ) ;
#1298 = DIRECTION ( 'NONE',  ( -0.000000000000000000, 1.000000000000000000, -0.000000000000000000 ) ) ;
#1299 = CIRCLE ( 'NONE', #39875, 60.00000000000000000 ) ;
#1300 = ORIENTED_EDGE ( 'NONE', *, *, #51415, .F. ) ;
#1301 = DIRECTION ( 'NONE',  ( 0.000000000000000000, 0.000000000000000000, 1.000000000000000000 ) ) ;
#1302 = AXIS2_PLACEMENT_3D ( 'NONE', #21570, #13935, #41795 ) ;
#1303 = CARTESIAN_POINT ( 'NONE',  ( -41.90263914168910730, -175.3837268820161057, -124.8268793598473536 ) ) ;
#1304 = ORIENTED_EDGE ( 'NONE', *, *, #40768, .T. ) ;
#1306 = ADVANCED_FACE ( 'NONE', ( #6325 ), #51257, .T. ) ;
#1305 = DIRECTION ( 'NONE',  ( 0.000000000000000000, -1.000000000000000000, 0.000000000000000000 ) ) ;
#1307 = VERTEX_POINT ( 'NONE', #39395 ) ;
#1308 = VECTOR ( 'NONE', #44248, 1000.000000000000000 ) ;
#1309 = DIRECTION ( 'NONE',  ( 0.000000000000000000, 0.000000000000000000, 1.000000000000000000 ) ) ;
#1310 = ORIENTED_EDGE ( 'NONE', *, *, #47140, .T. ) ;
#1311 = DIRECTION ( 'NONE',  ( 0.000000000000000000, 0.000000000000000000, -1.000000000000000000 ) ) ;
#1312 = ORIENTED_EDGE ( 'NONE', *, *, #8264, .T. ) ;
#1313 = LINE ( 'NONE', #21035, #20954 ) ;
#1314 = FACE_OUTER_BOUND ( 'NONE', #49501, .T. ) ;
#1315 = VERTEX_POINT ( 'NONE', #31256 ) ;
#1318 = ORIENTED_EDGE ( 'NONE', *, *, #36446, .T. ) ;
#1317 = CARTESIAN_POINT ( 'NONE',  ( -169.3144491972411458, -193.5000000000000000, -27.83926365844662243 ) ) ;
#1316 = LINE ( 'NONE', #8951, #2361 ) ;
#1319 = AXIS2_PLACEMENT_3D ( 'NONE', #32034, #7374, #44132 ) ;
#1320 = CYLINDRICAL_SURFACE ( 'NONE', #34823, 125.0000000000000000 ) ;
#1321 = AXIS2_PLACEMENT_3D ( 'NONE', #40544, #44773, #48975 ) ;
#1322 = ORIENTED_EDGE ( 'NONE', *, *, #37609, .F. ) ;
#1323 = CARTESIAN_POINT ( 'NONE',  ( -332.3517673607765914, -180.4803820837415458, -18.79457521708939183 ) ) ;
#1324 = VERTEX_POINT ( 'NONE', #3403 ) ;
#1325 = CIRCLE ( 'NONE', #49993, 60.00000000000000000 ) ;
#1326 = EDGE_CURVE ( 'NONE', #33159, #27840, #47310, .T. ) ;
#1327 = ADVANCED_FACE ( 'NONE', ( #28604 ), #15503, .F. ) ;
#1328 = CARTESIAN_POINT ( 'NONE',  ( -27.18512803868276251, -175.3837268820161057, -123.1729094355498404 ) ) ;
#1331 = VERTEX_POINT ( 'NONE', #12050 ) ;
#1330 = CYLINDRICAL_SURFACE ( 'NONE', #2156, 125.0000000000000000 ) ;
#1329 = CARTESIAN_POINT ( 'NONE',  ( -49.03777351731249468, -183.6283474603465606, -0.8294056854502022125 ) ) ;
#1332 = EDGE_LOOP ( 'NONE', ( #38979, #26674, #17451, #47872 ) ) ;
#1333 = CARTESIAN_POINT ( 'NONE',  ( -28.74596282265200387, -183.6283474603465606, 123.4325817657431230 ) ) ;
#1334 = CARTESIAN_POINT ( 'NONE',  ( -339.1964088526558498, -109.8658467157473666, -57.40522506028092664 ) ) ;
#1335 = LINE ( 'NONE', #41270, #48338 ) ;
#1336 = ORIENTED_EDGE ( 'NONE', *, *, #2039, .T. ) ;
#1337 = CIRCLE ( 'NONE', #12241, 125.0000000000000000 ) ;
#1338 = DIRECTION ( 'NONE',  ( -1.000000000000000000, 0.000000000000000000, -0.000000000000000000 ) ) ;
#1339 = CARTESIAN_POINT ( 'NONE',  ( -48.59739992243022755, -193.5000000000000000, 0.9929810960135230236 ) ) ;
#1340 = FACE_OUTER_BOUND ( 'NONE', #45350, .T. ) ;
#1341 = VECTOR ( 'NONE', #36641, 1000.000000000000114 ) ;
#1342 = CARTESIAN_POINT ( 'NONE',  ( -339.1964088526558498, -167.9936954712156592, -38.74998146212110584 ) ) ;
#1343 = ORIENTED_EDGE ( 'NONE', *, *, #38802, .T. ) ;
#1344 = AXIS2_PLACEMENT_3D ( 'NONE', #32340, #36546, #548 ) ;
#1345 = CARTESIAN_POINT ( 'NONE',  ( -332.3517673607765914, -133.2247606357419443, -58.25253621232173629 ) ) ;
#1346 = CARTESIAN_POINT ( 'NONE',  ( -60.00000000000000000, 20.00000000000000000, 60.00000000000000711 ) ) ;
#1347 = VECTOR ( 'NONE', #15644, 1000.000000000000000 ) ;
#1348 = CARTESIAN_POINT ( 'NONE',  ( -339.1964088526558498, -90.39567187580801999, 48.84008046109089918 ) ) ;
#1349 = VERTEX_POINT ( 'NONE', #40428 ) ;
#1350 = LINE ( 'NONE', #33919, #27318 ) ;
#1351 = CARTESIAN_POINT ( 'NONE',  ( -336.3521761649654422, -125.1322888500942270, -59.00000000000002132 ) ) ;
#1352 = EDGE_CURVE ( 'NONE', #50157, #51897, #16548, .T. ) ;
#1353 = DIRECTION ( 'NONE',  ( -1.000000000000000000, 0.000000000000000000, 0.000000000000000000 ) ) ;
#1354 = DIRECTION ( 'NONE',  ( -0.000000000000000000, 0.7485107481711089639, 0.6631226582407863113 ) ) ;
#1355 = EDGE_CURVE ( 'NONE', #17812, #19399, #35716, .T. ) ;
#1356 = DIRECTION ( 'NONE',  ( -0.000000000000000000, 1.000000000000000000, -0.000000000000000000 ) ) ;
#1357 = CIRCLE ( 'NONE', #6443, 124.9999999999999858 ) ;
#1358 = AXIS2_PLACEMENT_3D ( 'NONE', #26818, #2910, #38904 ) ;
#1359 = DIRECTION ( 'NONE',  ( -0.000000000000000000, 0.9709418174260544543, 0.2393156642875482465 ) ) ;
#1360 = DIRECTION ( 'NONE',  ( 0.000000000000000000, 0.000000000000000000, 1.000000000000000000 ) ) ;
#1362 = ORIENTED_EDGE ( 'NONE', *, *, #1875, .F. ) ;
#1361 = DIRECTION ( 'NONE',  ( 0.000000000000000000, -0.5680647467311625842, -0.8229838658936516893 ) ) ;
#1363 = AXIS2_PLACEMENT_3D ( 'NONE', #49455, #13429, #21315 ) ;
#1364 = AXIS2_PLACEMENT_3D ( 'NONE', #15252, #31267, #31014 ) ;
#1365 = EDGE_LOOP ( 'NONE', ( #28857, #5254, #34237, #45166 ) ) ;
#1366 = PLANE ( 'NONE',  #33333 ) ;
#1367 = DIRECTION ( 'NONE',  ( 0.000000000000000000, 0.000000000000000000, -1.000000000000000000 ) ) ;
#1369 = ORIENTED_EDGE ( 'NONE', *, *, #13916, .T. ) ;
#1368 = LINE ( 'NONE', #17925, #36265 ) ;
#1370 = AXIS2_PLACEMENT_3D ( 'NONE', #25566, #10325, #29765 ) ;
#1371 = ORIENTED_EDGE ( 'NONE', *, *, #44149, .F. ) ;
#1372 = STYLED_ITEM ( 'NONE', ( #29978 ), #1141 ) ;
#1373 = ORIENTED_EDGE ( 'NONE', *, *, #19823, .T. ) ;
#1374 = CARTESIAN_POINT ( 'NONE',  ( -55.99477380783410041, -189.7472609257535510, 123.7720294769269742 ) ) ;
#1375 = AXIS2_PLACEMENT_3D ( 'NONE', #1800, #6273, #26223 ) ;
#1376 =( GEOMETRIC_REPRESENTATION_CONTEXT ( 3 ) GLOBAL_UNCERTAINTY_ASSIGNED_CONTEXT ( ( #45358 ) ) GLOBAL_UNIT_ASSIGNED_CONTEXT ( ( #4980, #49384, #49891 ) ) REPRESENTATION_CONTEXT ( 'NONE', 'WORKASPACE' ) );
#1378 = AXIS2_PLACEMENT_3D ( 'NONE', #23024, #34580, #2290 ) ;
#1377 = DIRECTION ( 'NONE',  ( 0.000000000000000000, 1.000000000000000000, -0.000000000000000000 ) ) ;
#1379 = DIRECTION ( 'NONE',  ( -0.9842305779475967187, 0.000000000000000000, -0.1768902751225733538 ) ) ;
#1380 = EDGE_LOOP ( 'NONE', ( #18598, #51441, #27941, #10825 ) ) ;
#1381 = EDGE_CURVE ( 'NONE', #30637, #50432, #14027, .T. ) ;
#1382 = CIRCLE ( 'NONE', #547, 125.0000000000000000 ) ;
#1383 = CYLINDRICAL_SURFACE ( 'NONE', #44480, 20.00000000000000000 ) ;
#1385 = ORIENTED_EDGE ( 'NONE', *, *, #18610, .T. ) ;
#1384 = DIRECTION ( 'NONE',  ( 0.000000000000000000, -0.000000000000000000, -1.000000000000000000 ) ) ;
#1386 = DIRECTION ( 'NONE',  ( 0.000000000000000000, -0.000000000000000000, -1.000000000000000000 ) ) ;
#1387 = ORIENTED_EDGE ( 'NONE', *, *, #32294, .F. ) ;
#1388 = CARTESIAN_POINT ( 'NONE',  ( -165.5546359831674295, -183.6283474603465606, 43.79868877201490562 ) ) ;
#1389 = ORIENTED_EDGE ( 'NONE', *, *, #5272, .T. ) ;
#1390 = ADVANCED_FACE ( 'NONE', ( #229 ), #43860, .T. ) ;
#1391 = FACE_OUTER_BOUND ( 'NONE', #37604, .T. ) ;
#1392 = CARTESIAN_POINT ( 'NONE',  ( 9.518239912201957864, -193.5000000000000000, 110.7307791902283043 ) ) ;
#1393 = DIRECTION ( 'NONE',  ( -0.000000000000000000, 1.000000000000000000, -0.000000000000000000 ) ) ;
#1394 = ORIENTED_EDGE ( 'NONE', *, *, #30188, .F. ) ;
#1395 = EDGE_CURVE ( 'NONE', #22171, #8674, #44653, .T. ) ;
#1396 = VECTOR ( 'NONE', #49263, 1000.000000000000000 ) ;
#1397 = ORIENTED_EDGE ( 'NONE', *, *, #43576, .F. ) ;
#1398 = CARTESIAN_POINT ( 'NONE',  ( 14.43219681437621205, -175.3837268820161057, 106.8558168688117860 ) ) ;
#1399 = AXIS2_PLACEMENT_3D ( 'NONE', #20888, #36905, #891 ) ;
#1400 = CARTESIAN_POINT ( 'NONE',  ( -48.47912675150885065, -175.3837268820161057, 6.938893903907228378E-15 ) ) ;
#1401 = ORIENTED_EDGE ( 'NONE', *, *, #39450, .F. ) ;
#1402 = DIRECTION ( 'NONE',  ( -0.4566292373937018145, 0.000000000000000000, -0.8896570909947529859 ) ) ;
#1403 = AXIS2_PLACEMENT_3D ( 'NONE', #46707, #26453, #42759 ) ;
#1404 = VERTEX_POINT ( 'NONE', #4447 ) ;
#1405 = FACE_BOUND ( 'NONE', #49064, .T. ) ;
#1406 = DIRECTION ( 'NONE',  ( -1.000000000000000000, -0.000000000000000000, -0.000000000000000000 ) ) ;
#1407 = VERTEX_POINT ( 'NONE', #31513 ) ;
#1408 = CARTESIAN_POINT ( 'NONE',  ( -330.4913330509368166, -70.14212160686619768, -27.43969411971537298 ) ) ;
#1409 = EDGE_LOOP ( 'NONE', ( #45324, #25123, #5443, #33590 ) ) ;
#1410 = VECTOR ( 'NONE', #21939, 1000.000000000000000 ) ;
#1411 = FACE_OUTER_BOUND ( 'NONE', #11537, .T. ) ;
#1412 = VECTOR ( 'NONE', #14848, 1000.000000000000114 ) ;
#1413 = DIRECTION ( 'NONE',  ( -0.000000000000000000, 1.000000000000000000, -0.000000000000000000 ) ) ;
#1414 = EDGE_CURVE ( 'NONE', #46358, #8157, #21568, .T. ) ;
#1415 = ORIENTED_EDGE ( 'NONE', *, *, #21138, .T. ) ;
#1416 = VECTOR ( 'NONE', #47097, 1000.000000000000114 ) ;
#1417 = CIRCLE ( 'NONE', #25764, 124.9999999999999858 ) ;
#1418 = CARTESIAN_POINT ( 'NONE',  ( -166.6265240196292439, -193.5000000000000000, 40.81902153125349741 ) ) ;
#1419 = CARTESIAN_POINT ( 'NONE',  ( 43.86477233319989466, -189.7472609257535510, -84.24728067915975771 ) ) ;
#1420 = CARTESIAN_POINT ( 'NONE',  ( 72.12732647922463514, -193.5000000000000000, 28.81338593824055394 ) ) ;
#1421 = AXIS2_PLACEMENT_3D ( 'NONE', #13531, #9336, #48766 ) ;
#1422 = CARTESIAN_POINT ( 'NONE',  ( -171.9838957966129556, -189.7472609257535510, 19.27620354518722579 ) ) ;
#1423 = ORIENTED_EDGE ( 'NONE', *, *, #37765, .F. ) ;
#1425 = CIRCLE ( 'NONE', #36683, 124.9999999999999858 ) ;
#1424 = PLANE ( 'NONE',  #45461 ) ;
#1426 = EDGE_LOOP ( 'NONE', ( #34689, #15461, #25125, #12672 ) ) ;
#1427 = VERTEX_POINT ( 'NONE', #27581 ) ;
#1428 = DIRECTION ( 'NONE',  ( 0.000000000000000000, -0.000000000000000000, -1.000000000000000000 ) ) ;
#1430 = VERTEX_POINT ( 'NONE', #8129 ) ;
#1429 = LINE ( 'NONE', #46361, #45515 ) ;
#1431 = ORIENTED_EDGE ( 'NONE', *, *, #38871, .T. ) ;
#1432 = CARTESIAN_POINT ( 'NONE',  ( -48.47912675150885065, -188.5000000000000284, 15.00000000000000711 ) ) ;
#1433 = LINE ( 'NONE', #13523, #32982 ) ;
#1434 = AXIS2_PLACEMENT_3D ( 'NONE', #10702, #26728, #42764 ) ;
#1435 = AXIS2_PLACEMENT_3D ( 'NONE', #12915, #12651, #28675 ) ;
#1436 = VERTEX_POINT ( 'NONE', #7861 ) ;
#1437 = DIRECTION ( 'NONE',  ( 0.9995608365087940150, 0.000000000000000000, 0.02963332782257007206 ) ) ;
#1438 = ORIENTED_EDGE ( 'NONE', *, *, #13221, .T. ) ;
#1439 = DIRECTION ( 'NONE',  ( 1.000000000000000000, -0.000000000000000000, 0.000000000000000000 ) ) ;
#1440 = DIRECTION ( 'NONE',  ( 1.000000000000000000, -0.000000000000000000, -0.000000000000000000 ) ) ;
#1441 = VECTOR ( 'NONE', #40097, 1000.000000000000000 ) ;
#1442 = ADVANCED_FACE ( 'NONE', ( #43610 ), #32285, .T. ) ;
#1443 = CARTESIAN_POINT ( 'NONE',  ( -49.29161362951453640, -177.1207230881787780, 0.5829794791144718991 ) ) ;
#1444 = DIRECTION ( 'NONE',  ( 1.000000000000000000, -0.000000000000000000, 0.000000000000000000 ) ) ;
#1445 = ORIENTED_EDGE ( 'NONE', *, *, #36918, .F. ) ;
#1446 = VERTEX_POINT ( 'NONE', #39904 ) ;
#1447 = ORIENTED_EDGE ( 'NONE', *, *, #35273, .F. ) ;
#1448 = EDGE_CURVE ( 'NONE', #4651, #32642, #39181, .T. ) ;
#1449 = CARTESIAN_POINT ( 'NONE',  ( -336.3521761649654422, -158.3591674452439122, -47.62880233550485087 ) ) ;
#1450 = DIRECTION ( 'NONE',  ( 0.000000000000000000, -0.6631226582408039638, -0.7485107481710934207 ) ) ;
#1451 = VECTOR ( 'NONE', #28447, 1000.000000000000000 ) ;
#1452 = VECTOR ( 'NONE', #32909, 1000.000000000000000 ) ;
#1453 = VECTOR ( 'NONE', #27230, 1000.000000000000000 ) ;
#1454 = CARTESIAN_POINT ( 'NONE',  ( 71.97629403264900816, -193.5000000000000000, -29.43839964798648268 ) ) ;
#1455 = CARTESIAN_POINT ( 'NONE',  ( -22.62315034598912433, -183.6283474603465606, 121.2748789083720879 ) ) ;
#1456 = ORIENTED_EDGE ( 'NONE', *, *, #49931, .F. ) ;
#1457 = EDGE_CURVE ( 'NONE', #13383, #6473, #40682, .T. ) ;
#1458 = VECTOR ( 'NONE', #12419, 1000.000000000000000 ) ;
#1459 = EDGE_CURVE ( 'NONE', #26931, #31330, #7607, .T. ) ;
#1460 = EDGE_CURVE ( 'NONE', #6422, #44107, #5635, .T. ) ;
#1461 = CIRCLE ( 'NONE', #44264, 125.0000000000000000 ) ;
#1462 = ORIENTED_EDGE ( 'NONE', *, *, #7208, .F. ) ;
#1464 = ORIENTED_EDGE ( 'NONE', *, *, #42679, .F. ) ;
#1463 = DIRECTION ( 'NONE',  ( 1.043714542225393697E-14, 0.2393156642875652051, 0.9709418174260502354 ) ) ;
#1465 = FACE_OUTER_BOUND ( 'NONE', #49649, .T. ) ;
#1466 = VERTEX_POINT ( 'NONE', #15782 ) ;
#1467 = EDGE_CURVE ( 'NONE', #44354, #3275, #3933, .T. ) ;
#1468 = DIRECTION ( 'NONE',  ( 1.000000000000000000, -0.000000000000000000, 0.000000000000000000 ) ) ;
#1469 = DIRECTION ( 'NONE',  ( -0.000000000000000000, 1.000000000000000000, -0.000000000000000000 ) ) ;
#1470 = CARTESIAN_POINT ( 'NONE',  ( -339.1964088526558498, -180.6659093959932250, 14.60509510167942437 ) ) ;
#1471 = CARTESIAN_POINT ( 'NONE',  ( -305.0000000000000568, -136.2687678316390532, 58.62557946887775273 ) ) ;
#1472 = VERTEX_POINT ( 'NONE', #28350 ) ;
#1473 = CARTESIAN_POINT ( 'NONE',  ( 66.36634345758741915, -189.7472609257535510, 46.76022031560703596 ) ) ;
#1474 = EDGE_LOOP ( 'NONE', ( #39536, #6604, #3195, #26345 ) ) ;
#1475 = EDGE_LOOP ( 'NONE', ( #14015, #32657, #16736, #7496 ) ) ;
#1476 = CYLINDRICAL_SURFACE ( 'NONE', #46396, 125.0000000000000000 ) ;
#1477 = VECTOR ( 'NONE', #36099, 1000.000000000000227 ) ;
#1478 = AXIS2_PLACEMENT_3D ( 'NONE', #9676, #2040, #17822 ) ;
#1479 = PLANE ( 'NONE',  #26156 ) ;
#1480 = ORIENTED_EDGE ( 'NONE', *, *, #21090, .F. ) ;
#1481 = AXIS2_PLACEMENT_3D ( 'NONE', #844, #9003, #25805 ) ;
#1482 = CARTESIAN_POINT ( 'NONE',  ( -121.1142239062970418, -193.5000000000000000, 101.7307360698549132 ) ) ;
#1483 = DIRECTION ( 'NONE',  ( 0.000000000000000000, -0.9927088740980548609, -0.1205366802553164696 ) ) ;
#1484 = DIRECTION ( 'NONE',  ( 0.000000000000000000, -0.000000000000000000, -1.000000000000000000 ) ) ;
#1485 = LINE ( 'NONE', #44852, #45041 ) ;
#1486 = CARTESIAN_POINT ( 'NONE',  ( -80.17897391495031911, -183.6283474603465606, 120.9136869416132498 ) ) ;
#1487 = DIRECTION ( 'NONE',  ( -0.000000000000000000, -1.000000000000000000, 3.491481338843133355E-15 ) ) ;
#1488 = ORIENTED_EDGE ( 'NONE', *, *, #1518, .F. ) ;
#1489 = VECTOR ( 'NONE', #48761, 1000.000000000000000 ) ;
#1490 = CARTESIAN_POINT ( 'NONE',  ( -49.35486169370448550, -193.5000000000000000, -0.4827922027307481878 ) ) ;
#1491 = ORIENTED_EDGE ( 'NONE', *, *, #11344, .F. ) ;
#1492 = VERTEX_POINT ( 'NONE', #35991 ) ;
#1493 = CARTESIAN_POINT ( 'NONE',  ( 57.12946453413545100, -193.5000000000000000, 66.87170886602000053 ) ) ;
#1494 = ORIENTED_EDGE ( 'NONE', *, *, #1571, .T. ) ;
#1495 = AXIS2_PLACEMENT_3D ( 'NONE', #23370, #3637, #3381 ) ;
#1496 = FACE_OUTER_BOUND ( 'NONE', #51419, .T. ) ;
#1497 = LINE ( 'NONE', #49596, #21745 ) ;
#1499 = ORIENTED_EDGE ( 'NONE', *, *, #25402, .F. ) ;
#1498 = CARTESIAN_POINT ( 'NONE',  ( -332.3517673607765914, -123.5000000000000284, 0.000000000000000000 ) ) ;
#1500 = EDGE_CURVE ( 'NONE', #31475, #26646, #15679, .T. ) ;
#1501 = ADVANCED_FACE ( 'NONE', ( #31792 ), #47827, .F. ) ;
#1502 = FACE_OUTER_BOUND ( 'NONE', #47137, .T. ) ;
#1503 = VERTEX_POINT ( 'NONE', #31885 ) ;
#1504 = ORIENTED_EDGE ( 'NONE', *, *, #23750, .F. ) ;
#1505 = VERTEX_POINT ( 'NONE', #7204 ) ;
#1506 = DIRECTION ( 'NONE',  ( -0.000000000000000000, -0.9927088740980530845, 0.1205366802553303057 ) ) ;
#1507 = AXIS2_PLACEMENT_3D ( 'NONE', #18467, #14795, #22151 ) ;
#1508 = CARTESIAN_POINT ( 'NONE',  ( 1.707904493811027491, 28.00000000000000355, -46.30033279450969985 ) ) ;
#1509 = VECTOR ( 'NONE', #49312, 1000.000000000000000 ) ;
#1510 = ORIENTED_EDGE ( 'NONE', *, *, #25715, .F. ) ;
#1511 = DIRECTION ( 'NONE',  ( -0.1768902751225592818, 0.000000000000000000, -0.9842305779475992722 ) ) ;
#1512 = ADVANCED_FACE ( 'NONE', ( #47158 ), #35308, .T. ) ;
#1513 = CARTESIAN_POINT ( 'NONE',  ( -46.12632737020501850, -177.1207230881787780, -123.9784823535113532 ) ) ;
#1514 = LINE ( 'NONE', #48837, #36407 ) ;
#1515 = VERTEX_POINT ( 'NONE', #19036 ) ;
#1516 = AXIS2_PLACEMENT_3D ( 'NONE', #47396, #7462, #43182 ) ;
#1517 = EDGE_CURVE ( 'NONE', #37290, #42583, #47923, .T. ) ;
#1518 = EDGE_CURVE ( 'NONE', #16167, #12446, #40015, .T. ) ;
#1519 = FILL_AREA_STYLE_COLOUR ( '', #35988 ) ;
#1520 = DIRECTION ( 'NONE',  ( 0.000000000000000000, 1.137978600240785454E-13, -1.000000000000000000 ) ) ;
#1521 = ORIENTED_EDGE ( 'NONE', *, *, #13723, .T. ) ;
#1523 = ORIENTED_EDGE ( 'NONE', *, *, #45643, .F. ) ;
#1522 = DIRECTION ( 'NONE',  ( 0.000000000000000000, 0.000000000000000000, 1.000000000000000000 ) ) ;
#1524 = CIRCLE ( 'NONE', #51063, 125.0000000000000000 ) ;
#1525 = VERTEX_POINT ( 'NONE', #6945 ) ;
#1526 = ADVANCED_FACE ( 'NONE', ( #35827 ), #23242, .T. ) ;
#1527 = VERTEX_POINT ( 'NONE', #43193 ) ;
#1528 = DIRECTION ( 'NONE',  ( 0.000000000000000000, 1.000000000000000000, 0.000000000000000000 ) ) ;
#1529 = DIRECTION ( 'NONE',  ( 0.000000000000000000, 0.000000000000000000, 1.000000000000000000 ) ) ;
#1530 = ORIENTED_EDGE ( 'NONE', *, *, #4318, .T. ) ;
#1531 = ADVANCED_FACE ( 'NONE', ( #19302 ), #22974, .F. ) ;
#1532 = DIRECTION ( 'NONE',  ( 0.000000000000000000, -1.000000000000000000, 0.000000000000000000 ) ) ;
#1533 = DIRECTION ( 'NONE',  ( 0.000000000000000000, 0.000000000000000000, -1.000000000000000000 ) ) ;
#1534 = ORIENTED_EDGE ( 'NONE', *, *, #21442, .F. ) ;
#1535 = DIRECTION ( 'NONE',  ( 0.000000000000000000, 0.000000000000000000, -1.000000000000000000 ) ) ;
#1536 = EDGE_LOOP ( 'NONE', ( #49246, #12763, #14368, #6720 ) ) ;
#1537 = AXIS2_PLACEMENT_3D ( 'NONE', #40671, #219, #8630 ) ;
#1538 = ORIENTED_EDGE ( 'NONE', *, *, #40564, .T. ) ;
#1539 = DIRECTION ( 'NONE',  ( -0.000000000000000000, 1.000000000000000000, 0.000000000000000000 ) ) ;
#1540 = CARTESIAN_POINT ( 'NONE',  ( -31.47951320919342777, -177.1207230881787780, -122.8300162461135301 ) ) ;
#1541 = FACE_OUTER_BOUND ( 'NONE', #22455, .T. ) ;
#1542 = PRESENTATION_STYLE_ASSIGNMENT (( #41212 ) ) ;
#1543 = ORIENTED_EDGE ( 'NONE', *, *, #21168, .F. ) ;
#1544 = LINE ( 'NONE', #13627, #43335 ) ;
#1545 = CARTESIAN_POINT ( 'NONE',  ( 76.09804998693969935, -189.7472609257535510, 10.27263529369908035 ) ) ;
#1546 = PLANE ( 'NONE',  #35528 ) ;
#1547 = CARTESIAN_POINT ( 'NONE',  ( -87.28630321566652128, -183.6283474603465606, 118.8234112238818483 ) ) ;
#1548 = EDGE_LOOP ( 'NONE', ( #37061, #47666, #15788, #32243 ) ) ;
#1549 = DIRECTION ( 'NONE',  ( 0.000000000000000000, 3.561965537339043690E-14, 1.000000000000000000 ) ) ;
#1550 = DIRECTION ( 'NONE',  ( 0.000000000000000000, 0.000000000000000000, 1.000000000000000000 ) ) ;
#1551 = CARTESIAN_POINT ( 'NONE',  ( -157.5429198988176438, -175.3837268820161057, 61.07445476073480961 ) ) ;
#1552 = VERTEX_POINT ( 'NONE', #11387 ) ;
#1553 = VECTOR ( 'NONE', #42887, 1000.000000000000114 ) ;
#1554 = EDGE_LOOP ( 'NONE', ( #48728, #48848, #29321, #42812 ) ) ;
#1555 = AXIS2_PLACEMENT_3D ( 'NONE', #46658, #7224, #10650 ) ;
#1556 = CIRCLE ( 'NONE', #18330, 125.0000000000000000 ) ;
#1557 = VECTOR ( 'NONE', #5013, 1000.000000000000114 ) ;
#1558 = FACE_OUTER_BOUND ( 'NONE', #34449, .T. ) ;
#1559 = PLANE ( 'NONE',  #7687 ) ;
#1560 = ORIENTED_EDGE ( 'NONE', *, *, #31455, .F. ) ;
#1561 = CARTESIAN_POINT ( 'NONE',  ( -48.47912675150885065, -177.1207230881787780, 6.938893903907228378E-15 ) ) ;
#1562 = ORIENTED_EDGE ( 'NONE', *, *, #29542, .F. ) ;
#1563 = EDGE_CURVE ( 'NONE', #29872, #35764, #38985, .T. ) ;
#1564 = AXIS2_PLACEMENT_3D ( 'NONE', #7827, #453, #36733 ) ;
#1565 = LINE ( 'NONE', #33617, #30129 ) ;
#1566 = CARTESIAN_POINT ( 'NONE',  ( -19.28375372365792728, -189.7472609257535510, 121.5427093402341114 ) ) ;
#1567 = DIRECTION ( 'NONE',  ( 0.000000000000000000, 0.000000000000000000, -1.000000000000000000 ) ) ;
#1568 = CARTESIAN_POINT ( 'NONE',  ( -49.29161362951453640, -183.6283474603465606, 0.5829794791144718991 ) ) ;
#1569 = EDGE_CURVE ( 'NONE', #44024, #49925, #28264, .T. ) ;
#1570 = ADVANCED_FACE ( 'NONE', ( #27421 ), #7471, .F. ) ;
#1571 = EDGE_CURVE ( 'NONE', #13360, #44682, #27937, .T. ) ;
#1572 = DIRECTION ( 'NONE',  ( 0.000000000000000000, 0.000000000000000000, -1.000000000000000000 ) ) ;
#1573 = EDGE_CURVE ( 'NONE', #16038, #8568, #35063, .T. ) ;
#1574 = CARTESIAN_POINT ( 'NONE',  ( -339.1964088526558498, -182.5000000000000568, 0.5000000000000457412 ) ) ;
#1575 = VERTEX_POINT ( 'NONE', #15106 ) ;
#1576 = EDGE_CURVE ( 'NONE', #38828, #26805, #47678, .T. ) ;
#1577 = VECTOR ( 'NONE', #46399, 1000.000000000000114 ) ;
#1578 = CARTESIAN_POINT ( 'NONE',  ( -336.3521761649654422, -163.8460225846223466, -43.07972642080364523 ) ) ;
#1579 = EDGE_LOOP ( 'NONE', ( #13682, #26359, #41007, #16265 ) ) ;
#1580 = CARTESIAN_POINT ( 'NONE',  ( -60.00000000000000000, 0.000000000000000000, 60.00000000000000711 ) ) ;
#1581 = ORIENTED_EDGE ( 'NONE', *, *, #49509, .T. ) ;
#1582 = EDGE_CURVE ( 'NONE', #28072, #40574, #34159, .T. ) ;
#1583 = FACE_OUTER_BOUND ( 'NONE', #3576, .T. ) ;
#1584 = ORIENTED_EDGE ( 'NONE', *, *, #16405, .F. ) ;
#1585 = EDGE_CURVE ( 'NONE', #49925, #31203, #27158, .T. ) ;
#1586 = EDGE_CURVE ( 'NONE', #7784, #2629, #11903, .T. ) ;
#1587 = DIRECTION ( 'NONE',  ( 0.000000000000000000, 0.000000000000000000, -1.000000000000000000 ) ) ;
#1588 = DIRECTION ( 'NONE',  ( -0.000000000000000000, 0.000000000000000000, 1.000000000000000000 ) ) ;
#1589 = ORIENTED_EDGE ( 'NONE', *, *, #20475, .T. ) ;
#1592 = ORIENTED_EDGE ( 'NONE', *, *, #16049, .F. ) ;
#1591 = CARTESIAN_POINT ( 'NONE',  ( -339.1964088526558498, -123.5000000000000284, 0.000000000000000000 ) ) ;
#1590 = CARTESIAN_POINT ( 'NONE',  ( -330.4913330509368166, -101.7569374291120710, 55.92172413327804037 ) ) ;
#1593 = AXIS2_PLACEMENT_3D ( 'NONE', #30422, #5766, #33348 ) ;
#1594 = EDGE_CURVE ( 'NONE', #38089, #37325, #46907, .T. ) ;
#1595 = AXIS2_PLACEMENT_3D ( 'NONE', #25690, #45671, #48842 ) ;
#1596 = CARTESIAN_POINT ( 'NONE',  ( -32.87124591993210743, -193.5000000000000000, 124.0217483183788119 ) ) ;
#1597 = ORIENTED_EDGE ( 'NONE', *, *, #23576, .F. ) ;
#1598 = CARTESIAN_POINT ( 'NONE',  ( -339.1964088526558498, -138.1050951016792681, -57.16590939599323917 ) ) ;
#1599 = VECTOR ( 'NONE', #1511, 1000.000000000000000 ) ;
#1600 = ORIENTED_EDGE ( 'NONE', *, *, #14060, .T. ) ;
#1601 = EDGE_CURVE ( 'NONE', #45652, #30169, #23292, .T. ) ;
#1602 = CARTESIAN_POINT ( 'NONE',  ( 18.00181100848376303, -193.5000000000000000, -105.8550183720733742 ) ) ;
#1605 = VERTEX_POINT ( 'NONE', #9276 ) ;
#1604 = CARTESIAN_POINT ( 'NONE',  ( -339.1964088526558498, -183.4979166304964622, 0.5000000000000457412 ) ) ;
#1603 = CARTESIAN_POINT ( 'NONE',  ( 55.91309001144630031, -183.6283474603465606, 68.75510947788670535 ) ) ;
#1606 = VERTEX_POINT ( 'NONE', #4286 ) ;
#1607 = ADVANCED_FACE ( 'NONE', ( #45295 ), #28189, .F. ) ;
#1608 = AXIS2_PLACEMENT_3D ( 'NONE', #17791, #50624, #41950 ) ;
#1609 = LINE ( 'NONE', #49691, #13125 ) ;
#1610 = FACE_BOUND ( 'NONE', #35499, .T. ) ;
#1611 = CARTESIAN_POINT ( 'NONE',  ( -159.8192355313504720, -177.1207230881787780, -56.81883646197830018 ) ) ;
#1612 = EDGE_LOOP ( 'NONE', ( #12933, #1584, #930, #8824 ) ) ;
#1613 = CARTESIAN_POINT ( 'NONE',  ( -47.87232660569026166, -177.1207230881787780, 0.7948544414133635883 ) ) ;
#1614 = FACE_OUTER_BOUND ( 'NONE', #12502, .T. ) ;
#1615 = CARTESIAN_POINT ( 'NONE',  ( 38.71172987070728055, -175.3837268820161057, -89.56983042009262874 ) ) ;
#1616 = CARTESIAN_POINT ( 'NONE',  ( 51.65665342072240662, -177.1207230881787780, 74.81861753132422166 ) ) ;
#1617 = ORIENTED_EDGE ( 'NONE', *, *, #41907, .F. ) ;
#1618 = CARTESIAN_POINT ( 'NONE',  ( -164.3791542526839180, -175.3837268820161057, 46.82076062204521349 ) ) ;
#1619 = EDGE_CURVE ( 'NONE', #33402, #4, #12936, .T. ) ;
#1620 = DIRECTION ( 'NONE',  ( 1.000000000000000000, -0.000000000000000000, 0.000000000000000000 ) ) ;
#1621 = VECTOR ( 'NONE', #1192, 1000.000000000000000 ) ;
#1622 = EDGE_CURVE ( 'NONE', #34403, #5990, #24777, .T. ) ;
#1623 = PLANE ( 'NONE',  #24598 ) ;
#1624 = ORIENTED_EDGE ( 'NONE', *, *, #28231, .F. ) ;
#1625 = CARTESIAN_POINT ( 'NONE',  ( -339.1964088526558498, -116.8846903019852164, -58.63009191191289915 ) ) ;
#1626 = DIRECTION ( 'NONE',  ( 0.000000000000000000, 0.000000000000000000, 1.000000000000000000 ) ) ;
#1627 = LINE ( 'NONE', #17664, #43724 ) ;
#1628 = LINE ( 'NONE', #13193, #27463 ) ;
#1629 = PLANE ( 'NONE',  #44758 ) ;
#1630 = VECTOR ( 'NONE', #5258, 1000.000000000000227 ) ;
#1631 = DIRECTION ( 'NONE',  ( 0.000000000000000000, 1.000000000000000000, 0.000000000000000000 ) ) ;
#1632 = CARTESIAN_POINT ( 'NONE',  ( 54.54686566053560881, -177.1207230881787780, 69.00559874123592863 ) ) ;
#1634 = ORIENTED_EDGE ( 'NONE', *, *, #11718, .F. ) ;
#1633 = LINE ( 'NONE', #10286, #39618 ) ;
#1635 = VECTOR ( 'NONE', #40333, 1000.000000000000114 ) ;
#1636 = VERTEX_POINT ( 'NONE', #81 ) ;
#1637 = EDGE_CURVE ( 'NONE', #4347, #48702, #44495, .T. ) ;
#1638 = ADVANCED_FACE ( 'NONE', ( #16383 ), #40795, .T. ) ;
#1639 = PLANE ( 'NONE',  #41690 ) ;
#1640 = ADVANCED_FACE ( 'NONE', ( #601 ), #44756, .F. ) ;
#1641 = EDGE_CURVE ( 'NONE', #36857, #41966, #48448, .T. ) ;
#1642 = CARTESIAN_POINT ( 'NONE',  ( 46.00000000000000711, 33.00000000000000000, -46.00000000000000000 ) ) ;
#1644 = ORIENTED_EDGE ( 'NONE', *, *, #44601, .F. ) ;
#1643 = DIRECTION ( 'NONE',  ( 0.000000000000000000, 0.000000000000000000, -1.000000000000000000 ) ) ;
#1645 = ORIENTED_EDGE ( 'NONE', *, *, #27554, .T. ) ;
#1646 = ORIENTED_EDGE ( 'NONE', *, *, #11005, .T. ) ;
#1647 = CARTESIAN_POINT ( 'NONE',  ( 69.66827051661184100, -189.7472609257535510, -40.81902153125260213 ) ) ;
#1648 = LINE ( 'NONE', #41309, #30310 ) ;
#1649 = DIRECTION ( 'NONE',  ( 0.05924062789371441901, 0.000000000000000000, -0.9982437317643214625 ) ) ;
#1650 = ORIENTED_EDGE ( 'NONE', *, *, #18108, .F. ) ;
#1651 = AXIS2_PLACEMENT_3D ( 'NONE', #15372, #42953, #19316 ) ;
#1652 = CARTESIAN_POINT ( 'NONE',  ( -58.29063029684667896, -183.6283474603465606, 124.6143426664034735 ) ) ;
#1654 = ORIENTED_EDGE ( 'NONE', *, *, #39305, .F. ) ;
#1653 = PLANE ( 'NONE',  #16580 ) ;
#1655 = ADVANCED_FACE ( 'NONE', ( #16656 ), #8739, .F. ) ;
#1656 = CARTESIAN_POINT ( 'NONE',  ( -48.47912675150885065, -183.6283474603465606, 6.938893903907228378E-15 ) ) ;
#1657 = ORIENTED_EDGE ( 'NONE', *, *, #8173, .F. ) ;
#1658 = CARTESIAN_POINT ( 'NONE',  ( -143.3583119192899744, -193.5000000000000000, -81.38144888055202841 ) ) ;
#1659 = ORIENTED_EDGE ( 'NONE', *, *, #47832, .T. ) ;
#1660 = DIRECTION ( 'NONE',  ( 0.000000000000000000, 0.000000000000000000, 1.000000000000000000 ) ) ;
#1661 = LINE ( 'NONE', #1392, #15608 ) ;
#1662 = DIRECTION ( 'NONE',  ( 0.000000000000000000, 0.000000000000000000, -1.000000000000000000 ) ) ;
#1663 = EDGE_CURVE ( 'NONE', #6375, #21742, #5341, .T. ) ;
#1664 = ORIENTED_EDGE ( 'NONE', *, *, #10936, .T. ) ;
#1665 = ORIENTED_EDGE ( 'NONE', *, *, #5139, .F. ) ;
#1666 = CARTESIAN_POINT ( 'NONE',  ( -129.3001299485802633, -175.3837268820161057, -94.04236105995796891 ) ) ;
#1668 = VECTOR ( 'NONE', #24624, 1000.000000000000000 ) ;
#1667 = DIRECTION ( 'NONE',  ( -0.000000000000000000, -1.000000000000000000, -0.000000000000000000 ) ) ;
#1669 = EDGE_LOOP ( 'NONE', ( #25620, #39974, #32774, #39054 ) ) ;
#1670 = DIRECTION ( 'NONE',  ( -0.000000000000000000, -1.000000000000000000, 0.000000000000000000 ) ) ;
#1671 = VERTEX_POINT ( 'NONE', #36084 ) ;
#1672 = DIRECTION ( 'NONE',  ( -0.2920567706369764371, 0.000000000000000000, 0.9564009842765223146 ) ) ;
#1673 = DIRECTION ( 'NONE',  ( 0.000000000000000000, 1.000000000000000000, 0.000000000000000000 ) ) ;
#1674 = ORIENTED_EDGE ( 'NONE', *, *, #37092, .F. ) ;
#1675 = DIRECTION ( 'NONE',  ( 1.000000000000000000, 0.000000000000000000, -0.000000000000000000 ) ) ;
#1676 = ORIENTED_EDGE ( 'NONE', *, *, #27684, .T. ) ;
#1677 = DIRECTION ( 'NONE',  ( -0.000000000000000000, 1.000000000000000000, -0.000000000000000000 ) ) ;
#1678 = FACE_OUTER_BOUND ( 'NONE', #16337, .T. ) ;
#1679 = FACE_OUTER_BOUND ( 'NONE', #11462, .T. ) ;
#1680 = ORIENTED_EDGE ( 'NONE', *, *, #6740, .T. ) ;
#1681 = FACE_OUTER_BOUND ( 'NONE', #23617, .T. ) ;
#1682 = DIRECTION ( 'NONE',  ( -0.000000000000000000, 1.000000000000000000, -0.000000000000000000 ) ) ;
#1683 = PLANE ( 'NONE',  #41686 ) ;
#1684 = CARTESIAN_POINT ( 'NONE',  ( -146.0653709326077490, -175.3837268820161057, -78.11481899503411341 ) ) ;
#1685 = CIRCLE ( 'NONE', #22652, 125.0000000000000000 ) ;
#1686 = ORIENTED_EDGE ( 'NONE', *, *, #8609, .T. ) ;
#1687 = VECTOR ( 'NONE', #13517, 999.9999999999998863 ) ;
#1688 = DIRECTION ( 'NONE',  ( 0.000000000000000000, 1.000000000000000000, 0.000000000000000000 ) ) ;
#1689 = EDGE_LOOP ( 'NONE', ( #8500, #18459, #42674, #33934 ) ) ;
#1690 = FACE_OUTER_BOUND ( 'NONE', #43640, .T. ) ;
#1692 = ORIENTED_EDGE ( 'NONE', *, *, #36282, .T. ) ;
#1691 = DIRECTION ( 'NONE',  ( 0.000000000000000000, 0.000000000000000000, 1.000000000000000000 ) ) ;
#1693 = ORIENTED_EDGE ( 'NONE', *, *, #22106, .T. ) ;
#1694 = DIRECTION ( 'NONE',  ( -0.000000000000000000, 1.000000000000000000, -0.000000000000000000 ) ) ;
#1695 = EDGE_CURVE ( 'NONE', #32525, #6745, #4548, .T. ) ;
#1696 = CARTESIAN_POINT ( 'NONE',  ( 0.000000000000000000, -53.50000000000000000, 0.000000000000000000 ) ) ;
#1697 = ORIENTED_EDGE ( 'NONE', *, *, #26896, .T. ) ;
#1698 = AXIS2_PLACEMENT_3D ( 'NONE', #42605, #6618, #30510 ) ;
#1699 = DIRECTION ( 'NONE',  ( 5.399917434947259359E-17, 1.000000000000000000, -0.000000000000000000 ) ) ;
#1700 = ORIENTED_EDGE ( 'NONE', *, *, #15194, .T. ) ;
#1701 = PLANE ( 'NONE',  #14933 ) ;
#1702 = CARTESIAN_POINT ( 'NONE',  ( 64.01121016852529522, -189.7472609257535510, -54.50618404930953176 ) ) ;
#1703 = PLANE ( 'NONE',  #31958 ) ;
#1704 = CARTESIAN_POINT ( 'NONE',  ( -339.1964088526558498, -162.2499814621209850, 44.49369547121574442 ) ) ;
#1705 = ORIENTED_EDGE ( 'NONE', *, *, #22438, .T. ) ;
#1706 = ORIENTED_EDGE ( 'NONE', *, *, #8640, .T. ) ;
#1707 = LINE ( 'NONE', #33763, #11529 ) ;
#1708 = CARTESIAN_POINT ( 'NONE',  ( -336.3521761649654422, -135.0638248728647852, 57.91551518289418254 ) ) ;
#1709 = ADVANCED_FACE ( 'NONE', ( #24267 ), #623, .T. ) ;
#1710 = CARTESIAN_POINT ( 'NONE',  ( -171.5592422664403216, -193.5000000000000000, -21.82395850507255730 ) ) ;
#1711 = CARTESIAN_POINT ( 'NONE',  ( 20.10322172534453244, -193.5000000000000000, -103.3076327631963096 ) ) ;
#1712 = VERTEX_POINT ( 'NONE', #32663 ) ;
#1713 = UNCERTAINTY_MEASURE_WITH_UNIT (LENGTH_MEASURE( 1.000000000000000082E-05 ), #20522, 'distance_accuracy_value', 'NONE');
#1714 = VECTOR ( 'NONE', #20843, 1000.000000000000114 ) ;
#1715 = VECTOR ( 'NONE', #14032, 1000.000000000000000 ) ;
#1716 = ORIENTED_EDGE ( 'NONE', *, *, #3686, .F. ) ;
#1718 = ORIENTED_EDGE ( 'NONE', *, *, #41687, .T. ) ;
#1717 = DIRECTION ( 'NONE',  ( 1.000000000000000000, 0.000000000000000000, 0.000000000000000000 ) ) ;
#1719 = ORIENTED_EDGE ( 'NONE', *, *, #6024, .F. ) ;
#1720 = DIRECTION ( 'NONE',  ( -0.000000000000000000, 1.000000000000000000, -0.000000000000000000 ) ) ;
#1721 = ADVANCED_FACE ( 'NONE', ( #20845 ), #48960, .T. ) ;
#1722 = CARTESIAN_POINT ( 'NONE',  ( -332.3517673607765914, -164.5945333327934463, -42.41660376256285048 ) ) ;
#1723 = CARTESIAN_POINT ( 'NONE',  ( -77.77032474405883988, -189.7472609257535510, 120.4907712303052989 ) ) ;
#1724 = CARTESIAN_POINT ( 'NONE',  ( -160.3527926973206661, -189.7472609257535510, -53.48161459190847467 ) ) ;
#1725 = ORIENTED_EDGE ( 'NONE', *, *, #20475, .F. ) ;
#1727 = ADVANCED_FACE ( 'NONE', ( #859 ), #9020, .T. ) ;
#1726 = CARTESIAN_POINT ( 'NONE',  ( -48.47912675150885065, -213.5000000000000000, 125.0000000000000568 ) ) ;
#1728 = ORIENTED_EDGE ( 'NONE', *, *, #38691, .F. ) ;
#1729 = ORIENTED_EDGE ( 'NONE', *, *, #7976, .F. ) ;
#1730 = CARTESIAN_POINT ( 'NONE',  ( 33.75048693540708911, -189.7472609257535510, 94.14505102712816154 ) ) ;
#1731 = AXIS2_PLACEMENT_3D ( 'NONE', #9393, #41436, #5458 ) ;
#1732 = EDGE_CURVE ( 'NONE', #23376, #3470, #13196, .T. ) ;
#1733 = PLANE ( 'NONE',  #18597 ) ;
#1734 = ORIENTED_EDGE ( 'NONE', *, *, #16599, .F. ) ;
#1735 = CARTESIAN_POINT ( 'NONE',  ( -87.28630321566652128, -177.1207230881787780, 118.8234112238818483 ) ) ;
#1736 = PLANE ( 'NONE',  #41465 ) ;
#1737 = CARTESIAN_POINT ( 'NONE',  ( -336.3521761649654422, -67.40061919120938683, 18.46045550523129819 ) ) ;
#1738 = LINE ( 'NONE', #45901, #51749 ) ;
#1739 = EDGE_CURVE ( 'NONE', #787, #51398, #33176, .T. ) ;
#1740 = CARTESIAN_POINT ( 'NONE',  ( -160.3527926973206945, -193.5000000000000000, -53.48161459190837519 ) ) ;
#1741 = DIRECTION ( 'NONE',  ( 0.000000000000000000, 0.000000000000000000, -1.000000000000000000 ) ) ;
#1742 = ORIENTED_EDGE ( 'NONE', *, *, #10900, .F. ) ;
#1743 = DIRECTION ( 'NONE',  ( 0.000000000000000000, -0.000000000000000000, -1.000000000000000000 ) ) ;
#1744 = ORIENTED_EDGE ( 'NONE', *, *, #17339, .T. ) ;
#1745 = VECTOR ( 'NONE', #50030, 1000.000000000000000 ) ;
#1746 = VERTEX_POINT ( 'NONE', #45540 ) ;
#1747 = CARTESIAN_POINT ( 'NONE',  ( -168.4003408533108086, -183.6283474603465606, -35.26900067126609173 ) ) ;
#1748 = EDGE_CURVE ( 'NONE', #24620, #11600, #35022, .T. ) ;
#1749 = ORIENTED_EDGE ( 'NONE', *, *, #19202, .F. ) ;
#1750 = ADVANCED_FACE ( 'NONE', ( #6121 ), #6370, .F. ) ;
#1751 = AXIS2_PLACEMENT_3D ( 'NONE', #32827, #1024, #48879 ) ;
#1752 = DIRECTION ( 'NONE',  ( 0.000000000000000000, -0.5680647467311626952, -0.8229838658936516893 ) ) ;
#1753 = ADVANCED_FACE ( 'NONE', ( #14258 ), #37651, .T. ) ;
#1754 = DIRECTION ( 'NONE',  ( -0.000000000000000000, 1.000000000000000000, -0.000000000000000000 ) ) ;
#1756 = EDGE_LOOP ( 'NONE', ( #15179, #20096, #4669, #44013 ) ) ;
#1755 = CARTESIAN_POINT ( 'NONE',  ( -48.47912675150885065, -175.3837268820161057, 6.938893903907228378E-15 ) ) ;
#1757 = CARTESIAN_POINT ( 'NONE',  ( 76.51419089073348800, -183.6283474603465606, -1.292495564988658030 ) ) ;
#1758 = VERTEX_POINT ( 'NONE', #22138 ) ;
#1759 = ORIENTED_EDGE ( 'NONE', *, *, #9446, .T. ) ;
#1760 = ORIENTED_EDGE ( 'NONE', *, *, #31097, .T. ) ;
#1761 = PLANE ( 'NONE',  #9145 ) ;
#1762 = LINE ( 'NONE', #12804, #36908 ) ;
#1763 = CIRCLE ( 'NONE', #43702, 125.0000000000000000 ) ;
#1764 = ADVANCED_FACE ( 'NONE', ( #25550 ), #13731, .F. ) ;
#1765 = DIRECTION ( 'NONE',  ( 0.000000000000000000, 0.4647231720437604574, -0.8854560256532141294 ) ) ;
#1766 = CARTESIAN_POINT ( 'NONE',  ( -305.0000000000000568, -63.99980407363855761, 7.728304129923848187 ) ) ;
#1767 = DIRECTION ( 'NONE',  ( -0.000000000000000000, -3.491481338843133355E-15, -1.000000000000000000 ) ) ;
#1768 = ORIENTED_EDGE ( 'NONE', *, *, #15904, .T. ) ;
#1769 = CARTESIAN_POINT ( 'NONE',  ( -336.3521761649654422, -148.5878911270064009, 53.46519113769075204 ) ) ;
#1770 = DIRECTION ( 'NONE',  ( 1.000000000000000000, 0.000000000000000000, 0.000000000000000000 ) ) ;
#1772 = VERTEX_POINT ( 'NONE', #33947 ) ;
#1771 = PLANE ( 'NONE',  #17215 ) ;
#1773 = VERTEX_POINT ( 'NONE', #2430 ) ;
#1774 = VERTEX_POINT ( 'NONE', #18201 ) ;
#1775 = DIRECTION ( 'NONE',  ( 0.000000000000000000, 0.000000000000000000, 1.000000000000000000 ) ) ;
#1776 = DIRECTION ( 'NONE',  ( -0.4677363560876381943, 0.000000000000000000, -0.8838680338115290080 ) ) ;
#1777 = CIRCLE ( 'NONE', #28590, 125.0000000000000000 ) ;
#1778 = EDGE_LOOP ( 'NONE', ( #14927, #1845, #30448, #207 ) ) ;
#1779 = CARTESIAN_POINT ( 'NONE',  ( -305.0000000000000568, -183.0001959263613855, 7.728304129924832289 ) ) ;
#1780 = CARTESIAN_POINT ( 'NONE',  ( -137.9639882952644712, -183.6283474603465606, 87.27805883780237650 ) ) ;
#1781 = VERTEX_POINT ( 'NONE', #5604 ) ;
#1782 = CARTESIAN_POINT ( 'NONE',  ( -166.1003692892502102, -183.6283474603465606, -42.31126686685032467 ) ) ;
#1783 = ORIENTED_EDGE ( 'NONE', *, *, #1517, .F. ) ;
#1784 = VECTOR ( 'NONE', #46616, 1000.000000000000000 ) ;
#1785 = ORIENTED_EDGE ( 'NONE', *, *, #48329, .T. ) ;
#1786 = CARTESIAN_POINT ( 'NONE',  ( 141.7825277784304205, -193.5000000000000000, 41.45482488023466772 ) ) ;
#1787 = DIRECTION ( 'NONE',  ( -0.000000000000000000, 1.000000000000000000, -0.000000000000000000 ) ) ;
#1788 = VECTOR ( 'NONE', #41619, 1000.000000000000000 ) ;
#1789 = LINE ( 'NONE', #50165, #49053 ) ;
#1790 = ORIENTED_EDGE ( 'NONE', *, *, #41593, .T. ) ;
#1791 = DIRECTION ( 'NONE',  ( 0.000000000000000000, 0.000000000000000000, 1.000000000000000000 ) ) ;
#1792 = DIRECTION ( 'NONE',  ( -0.000000000000000000, 1.000000000000000000, -0.000000000000000000 ) ) ;
#1793 = ADVANCED_FACE ( 'NONE', ( #42622 ), #49500, .T. ) ;
#1794 = EDGE_CURVE ( 'NONE', #46340, #41311, #39223, .T. ) ;
#1795 = PLANE ( 'NONE',  #271 ) ;
#1796 = DIRECTION ( 'NONE',  ( 0.000000000000000000, 0.000000000000000000, -1.000000000000000000 ) ) ;
#1797 = ORIENTED_EDGE ( 'NONE', *, *, #14382, .F. ) ;
#1798 = CARTESIAN_POINT ( 'NONE',  ( -172.4465090799742484, -175.3837268820161057, -2.844930291600662908 ) ) ;
#1799 = FACE_OUTER_BOUND ( 'NONE', #32616, .T. ) ;
#1800 = CARTESIAN_POINT ( 'NONE',  ( -49.08592689732745384, -175.3837268820161057, 0.7948544414133550395 ) ) ;
#1801 = ORIENTED_EDGE ( 'NONE', *, *, #43259, .F. ) ;
#1802 = AXIS2_PLACEMENT_3D ( 'NONE', #13725, #45792, #25814 ) ;
#1803 = DIRECTION ( 'NONE',  ( 0.000000000000000000, 1.000000000000000000, 0.000000000000000000 ) ) ;
#1804 = DIRECTION ( 'NONE',  ( -0.000000000000000000, -1.000000000000000000, 0.000000000000000000 ) ) ;
#1805 = CARTESIAN_POINT ( 'NONE',  ( -48.47912675150885065, -183.6283474603465606, 6.938893903907228378E-15 ) ) ;
#1806 = VERTEX_POINT ( 'NONE', #34472 ) ;
#1807 = VERTEX_POINT ( 'NONE', #30021 ) ;
#1808 = ADVANCED_FACE ( 'NONE', ( #17692 ), #10307, .T. ) ;
#1809 = ORIENTED_EDGE ( 'NONE', *, *, #19299, .F. ) ;
#1810 = EDGE_CURVE ( 'NONE', #4093, #30219, #10056, .T. ) ;
#1811 = CARTESIAN_POINT ( 'NONE',  ( 11.61413489515543418, -193.5000000000000000, -109.6074810615842381 ) ) ;
#1812 = EDGE_CURVE ( 'NONE', #51297, #50020, #30526, .T. ) ;
#1813 = CARTESIAN_POINT ( 'NONE',  ( -336.3521761649654422, -74.01670616005314685, 32.17247266903214609 ) ) ;
#1814 = FACE_OUTER_BOUND ( 'NONE', #30369, .T. ) ;
#1815 = AXIS2_PLACEMENT_3D ( 'NONE', #21198, #8582, #37481 ) ;
#1816 = ADVANCED_FACE ( 'NONE', ( #26588 ), #46575, .T. ) ;
#1817 = CARTESIAN_POINT ( 'NONE',  ( 11.52087324849114580, -173.5000000000000284, 60.00000000000002132 ) ) ;
#1818 = CIRCLE ( 'NONE', #21103, 125.0000000000000000 ) ;
#1819 = DIRECTION ( 'NONE',  ( -0.000000000000000000, 1.000000000000000000, -0.000000000000000000 ) ) ;
#1820 = ORIENTED_EDGE ( 'NONE', *, *, #1619, .F. ) ;
#1821 = AXIS2_PLACEMENT_3D ( 'NONE', #19278, #7447, #47383 ) ;
#1822 = FACE_OUTER_BOUND ( 'NONE', #37747, .T. ) ;
#1823 = ORIENTED_EDGE ( 'NONE', *, *, #22345, .F. ) ;
#1824 = EDGE_CURVE ( 'NONE', #48760, #20039, #27474, .T. ) ;
#1825 = CARTESIAN_POINT ( 'NONE',  ( -169.6719064342497916, -177.1207230881787780, 30.61552143554989414 ) ) ;
#1826 = ORIENTED_EDGE ( 'NONE', *, *, #21827, .F. ) ;
#1827 = DIRECTION ( 'NONE',  ( 0.000000000000000000, -1.000000000000000000, 0.000000000000000000 ) ) ;
#1828 = VERTEX_POINT ( 'NONE', #49740 ) ;
#1829 = VECTOR ( 'NONE', #24491, 1000.000000000000000 ) ;
#1830 = FACE_OUTER_BOUND ( 'NONE', #26391, .T. ) ;
#1831 = DIRECTION ( 'NONE',  ( -0.05924062789372142729, 0.000000000000000000, 0.9982437317643209074 ) ) ;
#1832 = EDGE_LOOP ( 'NONE', ( #9607, #5027, #18686, #29002 ) ) ;
#1835 = ORIENTED_EDGE ( 'NONE', *, *, #45833, .F. ) ;
#1834 = DIRECTION ( 'NONE',  ( 1.000000000000000000, -0.000000000000000000, -0.000000000000000000 ) ) ;
#1833 = CARTESIAN_POINT ( 'NONE',  ( 62.13187335169531877, -183.6283474603465606, -58.22548115875871844 ) ) ;
#1836 = VECTOR ( 'NONE', #25683, 1000.000000000000000 ) ;
#1837 = DIRECTION ( 'NONE',  ( 0.000000000000000000, -0.9709418174260553425, -0.2393156642875449158 ) ) ;
#1838 = ORIENTED_EDGE ( 'NONE', *, *, #18840, .T. ) ;
#1839 = CARTESIAN_POINT ( 'NONE',  ( -336.3521761649654422, -72.48138011061176655, -29.74944317415788930 ) ) ;
#1840 = ORIENTED_EDGE ( 'NONE', *, *, #43935, .F. ) ;
#1841 = DIRECTION ( 'NONE',  ( 1.000000000000000000, -0.000000000000000000, 0.000000000000000000 ) ) ;
#1844 = ORIENTED_EDGE ( 'NONE', *, *, #39099, .T. ) ;
#1843 = CARTESIAN_POINT ( 'NONE',  ( -47.87232660569026166, -193.5000000000000000, 0.7948544414133635883 ) ) ;
#1842 = CARTESIAN_POINT ( 'NONE',  ( -339.1964088526558498, -123.5000000000000284, 0.000000000000000000 ) ) ;
#1845 = ORIENTED_EDGE ( 'NONE', *, *, #15707, .T. ) ;
#1846 = CARTESIAN_POINT ( 'NONE',  ( -339.1964088526558498, -71.02573290043878274, -26.97593913775585506 ) ) ;
#1847 = ORIENTED_EDGE ( 'NONE', *, *, #37755, .T. ) ;
#1848 = FACE_OUTER_BOUND ( 'NONE', #42521, .T. ) ;
#1849 = CARTESIAN_POINT ( 'NONE',  ( -170.9948556092908518, -175.3837268820161057, 19.12855698118476511 ) ) ;
#1850 = ORIENTED_EDGE ( 'NONE', *, *, #38795, .F. ) ;
#1851 = DIRECTION ( 'NONE',  ( 1.000000000000000000, 0.000000000000000000, -1.043714542225393381E-14 ) ) ;
#1852 = PLANE ( 'NONE',  #43357 ) ;
#1853 = CARTESIAN_POINT ( 'NONE',  ( -126.8597349762179363, -183.6283474603465606, -96.08646119223961080 ) ) ;
#1854 = VECTOR ( 'NONE', #46525, 999.9999999999998863 ) ;
#1855 = LINE ( 'NONE', #17898, #8115 ) ;
#1856 = ADVANCED_FACE ( 'NONE', ( #21628 ), #1653, .F. ) ;
#1857 = EDGE_CURVE ( 'NONE', #27687, #15211, #7648, .T. ) ;
#1858 = ORIENTED_EDGE ( 'NONE', *, *, #14910, .T. ) ;
#1859 = ADVANCED_FACE ( 'NONE', ( #35241 ), #42873, .F. ) ;
#1860 = AXIS2_PLACEMENT_3D ( 'NONE', #20882, #362, #28732 ) ;
#1861 = DIRECTION ( 'NONE',  ( -1.000000000000000000, 0.000000000000000000, 0.000000000000000000 ) ) ;
#1862 = CARTESIAN_POINT ( 'NONE',  ( 30.05499637021958392, -177.1207230881787780, -97.24912084693205827 ) ) ;
#1863 = EDGE_CURVE ( 'NONE', #34248, #50432, #27093, .T. ) ;
#1864 = VECTOR ( 'NONE', #21546, 1000.000000000000000 ) ;
#1865 = DIRECTION ( 'NONE',  ( 0.000000000000000000, 0.8660254037844375974, 0.5000000000000018874 ) ) ;
#1866 = VERTEX_POINT ( 'NONE', #2929 ) ;
#1867 = CARTESIAN_POINT ( 'NONE',  ( -336.3521761649653854, -179.0013928959018301, 22.79463504017430253 ) ) ;
#1868 = ADVANCED_FACE ( 'NONE', ( #3439 ), #7408, .F. ) ;
#1869 = DIRECTION ( 'NONE',  ( 0.000000000000000000, 0.000000000000000000, -1.000000000000000000 ) ) ;
#1870 = CARTESIAN_POINT ( 'NONE',  ( -332.3517673607765914, -73.44864141332200802, 31.34948880313848107 ) ) ;
#1871 = CARTESIAN_POINT ( 'NONE',  ( -332.3517673607765914, -77.59233547837267508, 37.15394033962009246 ) ) ;
#1872 = EDGE_CURVE ( 'NONE', #18062, #31552, #18967, .T. ) ;
#1873 = VECTOR ( 'NONE', #24437, 1000.000000000000000 ) ;
#1874 = AXIS2_PLACEMENT_3D ( 'NONE', #3336, #35914, #19621 ) ;
#1875 = EDGE_CURVE ( 'NONE', #31640, #9002, #31299, .T. ) ;
#1876 = DIRECTION ( 'NONE',  ( 0.000000000000000000, 0.000000000000000000, 1.000000000000000000 ) ) ;
#1877 = AXIS2_PLACEMENT_3D ( 'NONE', #1277, #24674, #489 ) ;
#1878 = AXIS2_PLACEMENT_3D ( 'NONE', #2232, #25370, #49811 ) ;
#1879 = EDGE_CURVE ( 'NONE', #46919, #4457, #35494, .T. ) ;
#1880 = LINE ( 'NONE', #2407, #26158 ) ;
#1881 = DIRECTION ( 'NONE',  ( -0.9646355819083614058, 0.000000000000000000, 0.2635871660690581320 ) ) ;
#1883 = ORIENTED_EDGE ( 'NONE', *, *, #7669, .F. ) ;
#1882 = CARTESIAN_POINT ( 'NONE',  ( 71.44208735029287993, -193.5000000000000000, 35.26900067126700833 ) ) ;
#1884 = EDGE_CURVE ( 'NONE', #29517, #13511, #23667, .T. ) ;
#1885 = ORIENTED_EDGE ( 'NONE', *, *, #18794, .F. ) ;
#1886 = EDGE_CURVE ( 'NONE', #28559, #24027, #39439, .T. ) ;
#1887 = DIRECTION ( 'NONE',  ( 0.000000000000000000, 1.000000000000000000, 0.000000000000000000 ) ) ;
#1889 = ORIENTED_EDGE ( 'NONE', *, *, #2045, .T. ) ;
#1888 = DIRECTION ( 'NONE',  ( -0.1768902751225802927, 0.000000000000000000, 0.9842305779475953864 ) ) ;
#1890 = EDGE_LOOP ( 'NONE', ( #11084, #37044, #22681, #14693 ) ) ;
#1891 = VERTEX_POINT ( 'NONE', #22657 ) ;
#1892 = DIRECTION ( 'NONE',  ( 0.000000000000000000, -0.000000000000000000, -1.000000000000000000 ) ) ;
#1893 = CIRCLE ( 'NONE', #11110, 125.0000000000000000 ) ;
#1894 = FACE_OUTER_BOUND ( 'NONE', #25378, .T. ) ;
#1895 = LINE ( 'NONE', #6114, #25506 ) ;
#1896 = ORIENTED_EDGE ( 'NONE', *, *, #8682, .T. ) ;
#1897 = EDGE_CURVE ( 'NONE', #31784, #30580, #42556, .T. ) ;
#1898 = VECTOR ( 'NONE', #49414, 1000.000000000000000 ) ;
#1899 = CARTESIAN_POINT ( 'NONE',  ( -166.9790462269952229, -183.6283474603465606, 36.52255268223130713 ) ) ;
#1900 = DIRECTION ( 'NONE',  ( -1.000000000000000000, 0.000000000000000000, 0.000000000000000000 ) ) ;
#1901 = ORIENTED_EDGE ( 'NONE', *, *, #33781, .F. ) ;
#1902 = CARTESIAN_POINT ( 'NONE',  ( 43.57032560458359427, -175.3837268820161057, 83.08371579725745448 ) ) ;
#1903 = ORIENTED_EDGE ( 'NONE', *, *, #6379, .T. ) ;
#1904 = DIRECTION ( 'NONE',  ( -0.000000000000000000, 0.8854560256532157947, 0.4647231720437573488 ) ) ;
#1905 = ORIENTED_EDGE ( 'NONE', *, *, #46481, .T. ) ;
#1906 = DIRECTION ( 'NONE',  ( 0.000000000000000000, -1.000000000000000000, 0.000000000000000000 ) ) ;
#1907 = LINE ( 'NONE', #30284, #42263 ) ;
#1908 = CARTESIAN_POINT ( 'NONE',  ( -336.3521761649654422, -93.75055682584159911, 51.01861988938794923 ) ) ;
#1909 = VECTOR ( 'NONE', #42535, 1000.000000000000000 ) ;
#1910 = VECTOR ( 'NONE', #46145, 1000.000000000000000 ) ;
#1911 = EDGE_LOOP ( 'NONE', ( #49021, #35930, #48876, #34096 ) ) ;
#1912 = EDGE_CURVE ( 'NONE', #27843, #10230, #39684, .T. ) ;
#1913 = AXIS2_PLACEMENT_3D ( 'NONE', #1737, #10140, #42450 ) ;
#1914 = VERTEX_POINT ( 'NONE', #11065 ) ;
#1915 = AXIS2_PLACEMENT_3D ( 'NONE', #1931, #29773, #33730 ) ;
#1916 = CARTESIAN_POINT ( 'NONE',  ( -339.1964088526558498, -123.5000000000000284, 0.000000000000000000 ) ) ;
#1917 = CARTESIAN_POINT ( 'NONE',  ( 53.18081239921338721, -175.3837268820161057, -72.73415134495935774 ) ) ;
#1918 = VERTEX_POINT ( 'NONE', #34725 ) ;
#1919 = LINE ( 'NONE', #30290, #29956 ) ;
#1920 = EDGE_CURVE ( 'NONE', #17726, #14905, #18228, .T. ) ;
#1921 = EDGE_CURVE ( 'NONE', #24400, #35572, #31639, .T. ) ;
#1922 = ORIENTED_EDGE ( 'NONE', *, *, #5475, .T. ) ;
#1923 = LINE ( 'NONE', #21903, #35115 ) ;
#1924 = VECTOR ( 'NONE', #39357, 1000.000000000000000 ) ;
#1925 = FACE_OUTER_BOUND ( 'NONE', #13673, .T. ) ;
#1926 = EDGE_CURVE ( 'NONE', #44533, #27697, #19905, .T. ) ;
#1927 = EDGE_CURVE ( 'NONE', #47587, #12138, #10824, .T. ) ;
#1928 = ORIENTED_EDGE ( 'NONE', *, *, #26949, .T. ) ;
#1929 = DIRECTION ( 'NONE',  ( -1.000000000000000000, 0.000000000000000000, 0.000000000000000000 ) ) ;
#1930 = EDGE_LOOP ( 'NONE', ( #40310, #22970, #23601, #11830 ) ) ;
#1931 = CARTESIAN_POINT ( 'NONE',  ( 19.33815737959698566, -193.5000000000000000, 105.0038855142078233 ) ) ;
#1932 = CYLINDRICAL_SURFACE ( 'NONE', #30648, 124.9999999999999858 ) ;
#1933 = DIRECTION ( 'NONE',  ( 0.000000000000000000, 1.000000000000000000, -0.000000000000000000 ) ) ;
#1934 = VERTEX_POINT ( 'NONE', #43654 ) ;
#1935 = AXIS2_PLACEMENT_3D ( 'NONE', #1986, #6721, #18026 ) ;
#1936 = LINE ( 'NONE', #46607, #14327 ) ;
#1937 = DIRECTION ( 'NONE',  ( -0.000000000000000000, -0.000000000000000000, 1.000000000000000000 ) ) ;
#1938 = DIRECTION ( 'NONE',  ( -0.000000000000000000, 1.000000000000000000, -0.000000000000000000 ) ) ;
#1939 = LINE ( 'NONE', #2902, #37484 ) ;
#1940 = VECTOR ( 'NONE', #19020, 1000.000000000000000 ) ;
#1941 = ORIENTED_EDGE ( 'NONE', *, *, #32061, .F. ) ;
#1942 = LINE ( 'NONE', #42660, #19538 ) ;
#1943 = EDGE_LOOP ( 'NONE', ( #11528, #24173, #21189, #38544 ) ) ;
#1944 = ADVANCED_FACE ( 'NONE', ( #14779 ), #51815, .T. ) ;
#1945 = CARTESIAN_POINT ( 'NONE',  ( -48.47912675150885065, -183.6283474603465606, 6.938893903907228378E-15 ) ) ;
#1947 = VERTEX_POINT ( 'NONE', #15814 ) ;
#1946 = CARTESIAN_POINT ( 'NONE',  ( 1.352451982137498288, -175.3837268820161057, 113.5465278748097120 ) ) ;
#1948 = ADVANCED_FACE ( 'NONE', ( #34993 ), #19234, .T. ) ;
#1949 = ORIENTED_EDGE ( 'NONE', *, *, #19178, .F. ) ;
#1950 = AXIS2_PLACEMENT_3D ( 'NONE', #27832, #15510, #34947 ) ;
#1951 = CIRCLE ( 'NONE', #31311, 60.00000000000000000 ) ;
#1952 = ADVANCED_FACE ( 'NONE', ( #20507 ), #12362, .F. ) ;
#1953 = CARTESIAN_POINT ( 'NONE',  ( 0.000000000000000000, -157.0158200571384555, -48.55604808772557845 ) ) ;
#1954 = AXIS2_PLACEMENT_3D ( 'NONE', #18171, #34197, #50244 ) ;
#1955 = ORIENTED_EDGE ( 'NONE', *, *, #25292, .T. ) ;
#1956 = DIRECTION ( 'NONE',  ( 0.000000000000000000, -0.6631226582408016323, -0.7485107481710953081 ) ) ;
#1957 = ORIENTED_EDGE ( 'NONE', *, *, #24495, .F. ) ;
#1958 = CARTESIAN_POINT ( 'NONE',  ( 141.7825277784304205, -213.5000000000000000, -41.45482488023466061 ) ) ;
#1959 = FACE_OUTER_BOUND ( 'NONE', #33108, .T. ) ;
#1960 = CIRCLE ( 'NONE', #9507, 125.0000000000000000 ) ;
#1961 = CARTESIAN_POINT ( 'NONE',  ( -48.47912675150885065, -187.5000000000000284, 6.938893903907228378E-15 ) ) ;
#1962 = DIRECTION ( 'NONE',  ( 0.000000000000000000, -0.7485107481711069655, -0.6631226582407885317 ) ) ;
#1963 = ORIENTED_EDGE ( 'NONE', *, *, #18900, .T. ) ;
#1964 = ORIENTED_EDGE ( 'NONE', *, *, #34614, .F. ) ;
#1965 = ORIENTED_EDGE ( 'NONE', *, *, #42964, .T. ) ;
#1966 = CARTESIAN_POINT ( 'NONE',  ( 67.04262753014327814, -193.5000000000000000, -47.74645837849745078 ) ) ;
#1967 = LINE ( 'NONE', #41909, #51215 ) ;
#1968 = CARTESIAN_POINT ( 'NONE',  ( 46.00000000000000000, 20.00000000000000000, -4.999999999999997335 ) ) ;
#1969 = DIRECTION ( 'NONE',  ( 0.000000000000000000, 0.000000000000000000, -1.000000000000000000 ) ) ;
#1970 = VECTOR ( 'NONE', #18162, 1000.000000000000000 ) ;
#1971 = EDGE_LOOP ( 'NONE', ( #5226, #20764, #28467, #41892 ) ) ;
#1972 = VECTOR ( 'NONE', #21782, 999.9999999999998863 ) ;
#1973 = VERTEX_POINT ( 'NONE', #25 ) ;
#1975 = ORIENTED_EDGE ( 'NONE', *, *, #11541, .T. ) ;
#1974 = CARTESIAN_POINT ( 'NONE',  ( -332.3517673607765914, -155.3847370087607374, 50.82679948493869659 ) ) ;
#1976 = LINE ( 'NONE', #21175, #2305 ) ;
#1977 = PLANE ( 'NONE',  #35888 ) ;
#1978 = CARTESIAN_POINT ( 'NONE',  ( 70.20858612167234014, -193.5000000000000000, 35.90758392117750475 ) ) ;
#1979 = ADVANCED_FACE ( 'NONE', ( #44168 ), #48117, .F. ) ;
#1981 = EDGE_CURVE ( 'NONE', #42791, #45363, #44962, .T. ) ;
#1980 = LINE ( 'NONE', #18021, #12520 ) ;
#1982 = ORIENTED_EDGE ( 'NONE', *, *, #45039, .F. ) ;
#1983 = LINE ( 'NONE', #50091, #17513 ) ;
#1984 = ORIENTED_EDGE ( 'NONE', *, *, #32401, .F. ) ;
#1985 = EDGE_LOOP ( 'NONE', ( #5666, #21081, #8976, #23007 ) ) ;
#1986 = CARTESIAN_POINT ( 'NONE',  ( -48.47912675150885065, -177.1207230881787780, 6.938893903907228378E-15 ) ) ;
#1987 = VECTOR ( 'NONE', #34606, 1000.000000000000000 ) ;
#1988 = CARTESIAN_POINT ( 'NONE',  ( -37.67038537088846084, -193.5000000000000000, -124.5318076226586470 ) ) ;
#1989 = ORIENTED_EDGE ( 'NONE', *, *, #51641, .F. ) ;
#1990 = PLANE ( 'NONE',  #15601 ) ;
#1991 = LINE ( 'NONE', #24874, #37273 ) ;
#1992 = CARTESIAN_POINT ( 'NONE',  ( -77.03256798524175508, -193.5000000000000000, 121.6951149130964893 ) ) ;
#1993 = CARTESIAN_POINT ( 'NONE',  ( 60.00000000000001421, -173.5000000000000284, -60.00000000000001421 ) ) ;
#1994 = FACE_OUTER_BOUND ( 'NONE', #3922, .T. ) ;
#1995 = ORIENTED_EDGE ( 'NONE', *, *, #26288, .T. ) ;
#1996 = EDGE_CURVE ( 'NONE', #51184, #4175, #32076, .T. ) ;
#1997 = DIRECTION ( 'NONE',  ( -0.000000000000000000, 1.000000000000000000, -0.000000000000000000 ) ) ;
#1998 = EDGE_LOOP ( 'NONE', ( #183, #26411, #20566, #24622, #17383, #13588, #43539, #23784, #24926, #42730, #22517, #11040, #16486, #25501, #28493, #28545 ) ) ;
#1999 = AXIS2_PLACEMENT_3D ( 'NONE', #25208, #41218, #22033 ) ;
#2000 = ORIENTED_EDGE ( 'NONE', *, *, #44753, .F. ) ;
#2001 = DIRECTION ( 'NONE',  ( 0.3482016354344059095, 0.000000000000000000, -0.9374196611341183427 ) ) ;
#2002 = EDGE_LOOP ( 'NONE', ( #49489, #38026, #38115, #8416 ) ) ;
#2003 = VECTOR ( 'NONE', #50671, 1000.000000000000000 ) ;
#2004 = ADVANCED_FACE ( 'NONE', ( #8171 ), #21038, .T. ) ;
#2005 = CARTESIAN_POINT ( 'NONE',  ( -336.3521761649654422, -148.5878911270064009, 53.46519113769075204 ) ) ;
#2006 = DIRECTION ( 'NONE',  ( -0.9027978299657387629, 0.000000000000000000, -0.4300652022765304450 ) ) ;
#2008 = VERTEX_POINT ( 'NONE', #24990 ) ;
#2007 = CARTESIAN_POINT ( 'NONE',  ( -305.0000000000000568, -73.21199843436539823, 32.72792230702599170 ) ) ;
#2009 = CARTESIAN_POINT ( 'NONE',  ( -336.3521761649654422, -123.5000000000000284, 0.000000000000000000 ) ) ;
#2010 = EDGE_CURVE ( 'NONE', #11472, #15531, #36026, .T. ) ;
#2012 = VECTOR ( 'NONE', #17562, 1000.000000000000114 ) ;
#2011 = DIRECTION ( 'NONE',  ( -1.000000000000000000, -0.000000000000000000, -0.000000000000000000 ) ) ;
#2013 = DIRECTION ( 'NONE',  ( -0.000000000000000000, 0.8854560256532093554, -0.4647231720437695057 ) ) ;
#2014 = ORIENTED_EDGE ( 'NONE', *, *, #47509, .F. ) ;
#2015 = ORIENTED_EDGE ( 'NONE', *, *, #42050, .T. ) ;
#2016 = ORIENTED_EDGE ( 'NONE', *, *, #51904, .F. ) ;
#2017 = DIRECTION ( 'NONE',  ( -0.000000000000000000, 1.000000000000000000, 0.000000000000000000 ) ) ;
#2018 = DIRECTION ( 'NONE',  ( -0.9995608365087946812, 0.000000000000000000, 0.02963332782254913048 ) ) ;
#2019 = PLANE ( 'NONE',  #17588 ) ;
#2020 = CARTESIAN_POINT ( 'NONE',  ( -120.5074237604784315, -177.1207230881787780, 100.9358816284415781 ) ) ;
#2021 = DIRECTION ( 'NONE',  ( 0.000000000000000000, 0.000000000000000000, -1.000000000000000000 ) ) ;
#2022 = ORIENTED_EDGE ( 'NONE', *, *, #31396, .T. ) ;
#2023 = EDGE_CURVE ( 'NONE', #10439, #23203, #48650, .T. ) ;
#2024 = CARTESIAN_POINT ( 'NONE',  ( -141.2664123866436512, -189.7472609257535510, -83.75869879877495805 ) ) ;
#2025 = ORIENTED_EDGE ( 'NONE', *, *, #35634, .T. ) ;
#2027 = VERTEX_POINT ( 'NONE', #3973 ) ;
#2026 = CARTESIAN_POINT ( 'NONE',  ( -48.47912675150885065, -189.7472609257535510, 6.938893903907228378E-15 ) ) ;
#2028 = ORIENTED_EDGE ( 'NONE', *, *, #12541, .F. ) ;
#2029 = DIRECTION ( 'NONE',  ( 1.000000000000000000, 0.000000000000000000, -0.000000000000000000 ) ) ;
#2030 = EDGE_LOOP ( 'NONE', ( #1657, #44514, #47588, #33493 ) ) ;
#2031 = DIRECTION ( 'NONE',  ( -0.000000000000000000, 1.000000000000000000, -0.000000000000000000 ) ) ;
#2032 = VECTOR ( 'NONE', #85, 1000.000000000000000 ) ;
#2033 = ORIENTED_EDGE ( 'NONE', *, *, #3479, .F. ) ;
#2034 = VECTOR ( 'NONE', #30484, 1000.000000000000000 ) ;
#2035 = FACE_OUTER_BOUND ( 'NONE', #23237, .T. ) ;
#2036 = EDGE_CURVE ( 'NONE', #28777, #33835, #10716, .T. ) ;
#2037 = DIRECTION ( 'NONE',  ( -0.4031234292879792847, 0.000000000000000000, 0.9151456172430153524 ) ) ;
#2038 = ORIENTED_EDGE ( 'NONE', *, *, #26229, .T. ) ;
#2039 = EDGE_CURVE ( 'NONE', #24589, #21989, #4230, .T. ) ;
#2040 = DIRECTION ( 'NONE',  ( 0.000000000000000000, -1.000000000000000000, 0.000000000000000000 ) ) ;
#2041 = ORIENTED_EDGE ( 'NONE', *, *, #7479, .F. ) ;
#2042 = CIRCLE ( 'NONE', #39797, 125.0000000000000000 ) ;
#2043 = ORIENTED_EDGE ( 'NONE', *, *, #3488, .T. ) ;
#2044 = CARTESIAN_POINT ( 'NONE',  ( -88.23625491228469286, -177.1207230881787780, 118.5089480183148254 ) ) ;
#2045 = EDGE_CURVE ( 'NONE', #33001, #21060, #49330, .T. ) ;
#2046 = DIRECTION ( 'NONE',  ( -0.000000000000000000, 1.000000000000000000, -0.000000000000000000 ) ) ;
#2047 = ORIENTED_EDGE ( 'NONE', *, *, #28252, .T. ) ;
#2048 = DIRECTION ( 'NONE',  ( -0.000000000000000000, 0.4647231720437755564, 0.8854560256532062468 ) ) ;
#2049 = DIRECTION ( 'NONE',  ( 0.000000000000000000, -1.000000000000000000, 0.000000000000000000 ) ) ;
#2050 = CONTEXT_DEPENDENT_SHAPE_REPRESENTATION ( #36732, #33558 ) ;
#2051 = CARTESIAN_POINT ( 'NONE',  ( -111.3295483157475445, -175.3837268820161057, 108.0501018472332504 ) ) ;
#2052 = DIRECTION ( 'NONE',  ( -0.000000000000000000, -1.000000000000000000, -0.000000000000000000 ) ) ;
#2053 = ORIENTED_EDGE ( 'NONE', *, *, #17300, .F. ) ;
#2054 = AXIS2_PLACEMENT_3D ( 'NONE', #46645, #14851, #6948 ) ;
#2055 = DIRECTION ( 'NONE',  ( 0.000000000000000000, -0.000000000000000000, -1.000000000000000000 ) ) ;
#2056 = DIRECTION ( 'NONE',  ( 0.000000000000000000, -1.000000000000000000, -1.156482317317871232E-16 ) ) ;
#2057 = DIRECTION ( 'NONE',  ( -1.000000000000000000, 0.000000000000000000, 0.000000000000000000 ) ) ;
#2058 = ORIENTED_EDGE ( 'NONE', *, *, #5070, .T. ) ;
#2059 = EDGE_CURVE ( 'NONE', #15758, #21929, #28386, .T. ) ;
#2060 = DIRECTION ( 'NONE',  ( -1.000000000000000000, 0.000000000000000000, 0.000000000000000000 ) ) ;
#2061 = DIRECTION ( 'NONE',  ( 0.000000000000000000, 0.000000000000000000, -1.000000000000000000 ) ) ;
#2062 = EDGE_LOOP ( 'NONE', ( #4658, #12449, #38211, #24993 ) ) ;
#2063 = CARTESIAN_POINT ( 'NONE',  ( -163.3245969606054473, -175.3837268820161057, -46.76022031560624015 ) ) ;
#2064 = VERTEX_POINT ( 'NONE', #8952 ) ;
#2065 = DIRECTION ( 'NONE',  ( 0.000000000000000000, 0.000000000000000000, 1.000000000000000000 ) ) ;
#2066 = CARTESIAN_POINT ( 'NONE',  ( 70.98542830588607444, -177.1207230881787780, -36.78613984829961936 ) ) ;
#2067 = DIRECTION ( 'NONE',  ( 0.000000000000000000, 1.000000000000000000, 0.000000000000000000 ) ) ;
#2068 = CIRCLE ( 'NONE', #22220, 125.0000000000000000 ) ;
#2069 = AXIS2_PLACEMENT_3D ( 'NONE', #33598, #33076, #49122 ) ;
#2070 = CARTESIAN_POINT ( 'NONE',  ( -135.4449840867448813, -175.3837268820161057, -88.39086586114741806 ) ) ;
#2071 = DIRECTION ( 'NONE',  ( 0.000000000000000000, 0.000000000000000000, 1.000000000000000000 ) ) ;
#2072 = ORIENTED_EDGE ( 'NONE', *, *, #42858, .T. ) ;
#2073 = AXIS2_PLACEMENT_3D ( 'NONE', #8206, #4261, #7684 ) ;
#2074 = PLANE ( 'NONE',  #46633 ) ;
#2075 = ORIENTED_EDGE ( 'NONE', *, *, #7715, .F. ) ;
#2076 = DIRECTION ( 'NONE',  ( -0.000000000000000000, 1.000000000000000000, -0.000000000000000000 ) ) ;
#2077 = VERTEX_POINT ( 'NONE', #36808 ) ;
#2078 = STYLED_ITEM ( 'NONE', ( #51484 ), #2369 ) ;
#2079 = DIRECTION ( 'NONE',  ( 0.9929810960135178055, 0.000000000000000000, -0.1182731709213592358 ) ) ;
#2080 = EDGE_CURVE ( 'NONE', #11778, #9277, #42598, .T. ) ;
#2081 = CIRCLE ( 'NONE', #7973, 125.0000000000000000 ) ;
#2082 = PLANE ( 'NONE',  #36811 ) ;
#2083 = PRODUCT_DEFINITION_SHAPE ( 'NONE', 'NONE',  #38299 ) ;
#2084 = DIRECTION ( 'NONE',  ( 0.000000000000000000, 0.000000000000000000, -1.000000000000000000 ) ) ;
#2085 = VERTEX_POINT ( 'NONE', #4491 ) ;
#2088 = VERTEX_POINT ( 'NONE', #36530 ) ;
#2087 = DIRECTION ( 'NONE',  ( 0.000000000000000000, 0.000000000000000000, -1.000000000000000000 ) ) ;
#2086 = LINE ( 'NONE', #14200, #33435 ) ;
#2089 = DIRECTION ( 'NONE',  ( 0.1182731709213523247, 0.000000000000000000, 0.9929810960135185827 ) ) ;
#2090 = ORIENTED_EDGE ( 'NONE', *, *, #48491, .F. ) ;
#2091 = DIRECTION ( 'NONE',  ( 0.000000000000000000, 0.000000000000000000, -1.000000000000000000 ) ) ;
#2092 = ORIENTED_EDGE ( 'NONE', *, *, #21148, .F. ) ;
#2093 = EDGE_CURVE ( 'NONE', #37313, #33085, #526, .T. ) ;
#2094 = CARTESIAN_POINT ( 'NONE',  ( 43.18784210722336780, -193.5000000000000000, -84.98333260264752198 ) ) ;
#2097 = ORIENTED_EDGE ( 'NONE', *, *, #23885, .F. ) ;
#2096 = DIRECTION ( 'NONE',  ( 0.000000000000000000, -1.000000000000000000, 0.000000000000000000 ) ) ;
#2095 = CARTESIAN_POINT ( 'NONE',  ( -330.4913330509368166, -71.49045607248213230, 27.86139516340826461 ) ) ;
#2098 = ORIENTED_EDGE ( 'NONE', *, *, #36008, .T. ) ;
#2099 = EDGE_CURVE ( 'NONE', #40342, #34406, #37057, .T. ) ;
#2100 = DIRECTION ( 'NONE',  ( 0.000000000000000000, 0.000000000000000000, -1.000000000000000000 ) ) ;
#2101 = VERTEX_POINT ( 'NONE', #805 ) ;
#2102 = CARTESIAN_POINT ( 'NONE',  ( -45.12595152424214717, -177.1207230881787780, -123.9551692589637355 ) ) ;
#2103 = EDGE_CURVE ( 'NONE', #5601, #15102, #31679, .T. ) ;
#2104 = AXIS2_PLACEMENT_3D ( 'NONE', #5999, #22023, #30171 ) ;
#2105 = DIRECTION ( 'NONE',  ( -0.1768902751225802927, 0.000000000000000000, 0.9842305779475953864 ) ) ;
#2106 = ORIENTED_EDGE ( 'NONE', *, *, #22584, .F. ) ;
#2107 = CARTESIAN_POINT ( 'NONE',  ( 76.43863189440992301, -193.5000000000000000, -4.533605064403313456 ) ) ;
#2108 = DIRECTION ( 'NONE',  ( 0.000000000000000000, 0.000000000000000000, 1.000000000000000000 ) ) ;
#2109 = DIRECTION ( 'NONE',  ( 0.000000000000000000, -1.000000000000000000, -0.000000000000000000 ) ) ;
#2110 = CARTESIAN_POINT ( 'NONE',  ( -162.7543581613524282, -177.1207230881787780, 50.65739320402010293 ) ) ;
#2111 = VECTOR ( 'NONE', #28589, 1000.000000000000000 ) ;
#2112 = LINE ( 'NONE', #34687, #2235 ) ;
#2113 = VECTOR ( 'NONE', #18607, 1000.000000000000000 ) ;
#2114 = ORIENTED_EDGE ( 'NONE', *, *, #17253, .F. ) ;
#2115 = LINE ( 'NONE', #17402, #1970 ) ;
#2117 = VECTOR ( 'NONE', #32241, 1000.000000000000000 ) ;
#2116 = CARTESIAN_POINT ( 'NONE',  ( 71.44208735029287993, -193.5000000000000000, 35.26900067126700833 ) ) ;
#2118 = DIRECTION ( 'NONE',  ( 0.000000000000000000, -0.000000000000000000, -1.000000000000000000 ) ) ;
#2119 = EDGE_LOOP ( 'NONE', ( #36419, #24935 ) ) ;
#2120 = PLANE ( 'NONE',  #5513 ) ;
#2121 = DIRECTION ( 'NONE',  ( 0.000000000000000000, 3.491481338843133355E-15, 1.000000000000000000 ) ) ;
#2122 = AXIS2_PLACEMENT_3D ( 'NONE', #25183, #5984, #17568 ) ;
#2123 = AXIS2_PLACEMENT_3D ( 'NONE', #17491, #1699, #2212 ) ;
#2124 = CARTESIAN_POINT ( 'NONE',  ( -76.79768193946081567, -189.7472609257535510, 120.7230919990160629 ) ) ;
#2125 = DIRECTION ( 'NONE',  ( -0.8455960035018272869, 0.000000000000000000, 0.5338233779647886257 ) ) ;
#2126 = CIRCLE ( 'NONE', #11346, 124.9999999999999858 ) ;
#2127 = FACE_OUTER_BOUND ( 'NONE', #46157, .T. ) ;
#2128 = CIRCLE ( 'NONE', #24792, 125.0000000000000000 ) ;
#2129 = CARTESIAN_POINT ( 'NONE',  ( -129.4514457347087273, -189.7472609257535510, 95.22858582633115532 ) ) ;
#2130 = DIRECTION ( 'NONE',  ( 0.000000000000000000, -0.000000000000000000, 1.000000000000000000 ) ) ;
#2131 = DIRECTION ( 'NONE',  ( 0.000000000000000000, 1.000000000000000000, 0.000000000000000000 ) ) ;
#2132 = EDGE_LOOP ( 'NONE', ( #33701, #19771, #39541, #1015 ) ) ;
#2133 = CARTESIAN_POINT ( 'NONE',  ( -336.3521761649654422, -66.60506506233235768, -15.70448169564047092 ) ) ;
#2134 = CARTESIAN_POINT ( 'NONE',  ( -48.47912675150885065, -177.1207230881787780, 6.938893903907228378E-15 ) ) ;
#2136 = ORIENTED_EDGE ( 'NONE', *, *, #14737, .T. ) ;
#2135 = LINE ( 'NONE', #5331, #21984 ) ;
#2137 = EDGE_LOOP ( 'NONE', ( #2561, #78, #22612, #13279 ) ) ;
#2138 = AXIS2_PLACEMENT_3D ( 'NONE', #39710, #3723, #28411 ) ;
#2139 = ORIENTED_EDGE ( 'NONE', *, *, #42202, .F. ) ;
#2140 = LINE ( 'NONE', #26062, #48572 ) ;
#2141 = AXIS2_PLACEMENT_3D ( 'NONE', #4836, #36098, #32677 ) ;
#2142 = VECTOR ( 'NONE', #41033, 1000.000000000000000 ) ;
#2143 = EDGE_CURVE ( 'NONE', #31995, #28202, #33114, .T. ) ;
#2144 = ADVANCED_FACE ( 'NONE', ( #13154 ), #49936, .T. ) ;
#2145 = EDGE_CURVE ( 'NONE', #34105, #6023, #6050, .T. ) ;
#2146 = DIRECTION ( 'NONE',  ( 0.000000000000000000, 0.000000000000000000, -1.000000000000000000 ) ) ;
#2147 = CARTESIAN_POINT ( 'NONE',  ( -47.50057025920934706, -193.5000000000000000, 0.2059786187411091207 ) ) ;
#2148 = ORIENTED_EDGE ( 'NONE', *, *, #17541, .T. ) ;
#2149 = EDGE_CURVE ( 'NONE', #35111, #467, #45480, .T. ) ;
#2150 = PLANE ( 'NONE',  #41044 ) ;
#2151 = CARTESIAN_POINT ( 'NONE',  ( -18.54723674587610560, -175.3837268820161057, 120.3332351033025702 ) ) ;
#2154 = ORIENTED_EDGE ( 'NONE', *, *, #14509, .T. ) ;
#2153 = DIRECTION ( 'NONE',  ( 0.000000000000000000, 0.000000000000000000, 1.000000000000000000 ) ) ;
#2152 = DIRECTION ( 'NONE',  ( -0.000000000000000000, 1.000000000000000000, -0.000000000000000000 ) ) ;
#2155 = EDGE_CURVE ( 'NONE', #39056, #30801, #46817, .T. ) ;
#2156 = AXIS2_PLACEMENT_3D ( 'NONE', #1843, #26531, #17388 ) ;
#2157 = EDGE_CURVE ( 'NONE', #34413, #28554, #5812, .T. ) ;
#2158 = CIRCLE ( 'NONE', #26462, 125.0000000000000000 ) ;
#2159 = DIRECTION ( 'NONE',  ( -1.000000000000000000, 0.000000000000000000, 0.000000000000000000 ) ) ;
#2160 = ORIENTED_EDGE ( 'NONE', *, *, #11113, .T. ) ;
#2161 = CARTESIAN_POINT ( 'NONE',  ( -330.4913330509368166, -63.50208336950359467, -0.4999999999999549249 ) ) ;
#2162 = ORIENTED_EDGE ( 'NONE', *, *, #16135, .T. ) ;
#2163 = CARTESIAN_POINT ( 'NONE',  ( -339.1964088526558498, -66.33409060400650503, 14.60509510167813474 ) ) ;
#2164 = ADVANCED_FACE ( 'NONE', ( #21825 ), #9473, .F. ) ;
#2165 = AXIS2_PLACEMENT_3D ( 'NONE', #19048, #2497, #27168 ) ;
#2166 = DIRECTION ( 'NONE',  ( 0.000000000000000000, 0.000000000000000000, 1.000000000000000000 ) ) ;
#2167 = PLANE ( 'NONE',  #13173 ) ;
#2168 = ADVANCED_FACE ( 'NONE', ( #26260 ), #45735, .F. ) ;
#2169 = AXIS2_PLACEMENT_3D ( 'NONE', #27163, #26913, #21756 ) ;
#2170 = DIRECTION ( 'NONE',  ( 1.000000000000000000, -0.000000000000000000, 0.000000000000000000 ) ) ;
#2171 = VERTEX_POINT ( 'NONE', #49677 ) ;
#2172 = DIRECTION ( 'NONE',  ( 0.000000000000000000, -1.000000000000000000, 0.000000000000000000 ) ) ;
#2173 = EDGE_CURVE ( 'NONE', #23894, #7466, #29954, .T. ) ;
#2174 = LINE ( 'NONE', #6137, #44325 ) ;
#2175 = VERTEX_POINT ( 'NONE', #14201 ) ;
#2176 = LINE ( 'NONE', #34241, #43353 ) ;
#2177 = ADVANCED_FACE ( 'NONE', ( #25759 ), #22068, .T. ) ;
#2178 = ORIENTED_EDGE ( 'NONE', *, *, #4779, .F. ) ;
#2179 = FACE_BOUND ( 'NONE', #2531, .T. ) ;
#2180 = LINE ( 'NONE', #50541, #3794 ) ;
#2181 = ORIENTED_EDGE ( 'NONE', *, *, #15241, .F. ) ;
#2182 = DIRECTION ( 'NONE',  ( 0.000000000000000000, 1.000000000000000000, 0.000000000000000000 ) ) ;
#2183 = ORIENTED_EDGE ( 'NONE', *, *, #5257, .T. ) ;
#2184 = CIRCLE ( 'NONE', #42431, 125.0000000000000000 ) ;
#2185 = VECTOR ( 'NONE', #26743, 1000.000000000000000 ) ;
#2186 = DIRECTION ( 'NONE',  ( 0.05924062789372142729, 0.000000000000000000, -0.9982437317643209074 ) ) ;
#2187 = DIRECTION ( 'NONE',  ( 1.000000000000000000, 0.000000000000000000, -0.000000000000000000 ) ) ;
#2188 = ORIENTED_EDGE ( 'NONE', *, *, #47808, .F. ) ;
#2189 = AXIS2_PLACEMENT_3D ( 'NONE', #51766, #24168, #16022 ) ;
#2190 = AXIS2_PLACEMENT_3D ( 'NONE', #2950, #14798, #2446 ) ;
#2191 = LINE ( 'NONE', #19002, #2203 ) ;
#2192 = DIRECTION ( 'NONE',  ( 0.000000000000000000, 0.000000000000000000, 1.000000000000000000 ) ) ;
#2193 = DIRECTION ( 'NONE',  ( -0.000000000000000000, 1.000000000000000000, -0.000000000000000000 ) ) ;
#2194 = ADVANCED_FACE ( 'NONE', ( #17875 ), #34415, .F. ) ;
#2195 = EDGE_LOOP ( 'NONE', ( #8009, #47301, #15968, #2015 ) ) ;
#2196 = DIRECTION ( 'NONE',  ( -0.000000000000000000, -0.2393156642875516049, 0.9709418174260534551 ) ) ;
#2197 = ORIENTED_EDGE ( 'NONE', *, *, #48323, .T. ) ;
#2198 = CIRCLE ( 'NONE', #4753, 125.0000000000000000 ) ;
#2199 = CARTESIAN_POINT ( 'NONE',  ( -180.0000000000000568, -108.2550424820446295, 0.000000000000000000 ) ) ;
#2200 = CARTESIAN_POINT ( 'NONE',  ( -339.1964088526558498, -68.51134412508183402, -21.38919645685240312 ) ) ;
#2202 = ORIENTED_EDGE ( 'NONE', *, *, #39930, .F. ) ;
#2201 = DIRECTION ( 'NONE',  ( 1.000000000000000000, 0.000000000000000000, 0.000000000000000000 ) ) ;
#2203 = VECTOR ( 'NONE', #18484, 1000.000000000000000 ) ;
#2204 = CIRCLE ( 'NONE', #11538, 125.0000000000000000 ) ;
#2205 = ORIENTED_EDGE ( 'NONE', *, *, #34534, .F. ) ;
#2206 = DIRECTION ( 'NONE',  ( -0.9646355819083556327, 0.000000000000000000, -0.2635871660690782825 ) ) ;
#2207 = AXIS2_PLACEMENT_3D ( 'NONE', #30730, #26794, #13685 ) ;
#2208 = VECTOR ( 'NONE', #14856, 1000.000000000000000 ) ;
#2209 = EDGE_CURVE ( 'NONE', #47040, #41966, #11300, .T. ) ;
#2210 = CARTESIAN_POINT ( 'NONE',  ( -336.3521761649653854, -69.63373947859463442, 26.42775013958025454 ) ) ;
#2211 = ORIENTED_EDGE ( 'NONE', *, *, #30393, .T. ) ;
#2212 = DIRECTION ( 'NONE',  ( -1.000000000000000000, 0.000000000000000000, 0.000000000000000000 ) ) ;
#2213 = ORIENTED_EDGE ( 'NONE', *, *, #24726, .T. ) ;
#2214 = DIRECTION ( 'NONE',  ( 0.000000000000000000, 1.000000000000000000, 0.000000000000000000 ) ) ;
#2215 = CARTESIAN_POINT ( 'NONE',  ( 72.89680503569744019, -189.7472609257535510, -25.37485791684303393 ) ) ;
#2216 = EDGE_CURVE ( 'NONE', #24027, #4633, #37320, .T. ) ;
#2217 = EDGE_CURVE ( 'NONE', #46918, #35839, #50792, .T. ) ;
#2218 = EDGE_CURVE ( 'NONE', #10123, #9353, #50208, .T. ) ;
#2219 = EDGE_CURVE ( 'NONE', #24784, #51869, #10240, .T. ) ;
#2220 = DIRECTION ( 'NONE',  ( 0.000000000000000000, 1.000000000000000000, -0.000000000000000000 ) ) ;
#2221 = DIRECTION ( 'NONE',  ( -8.718379230999705894E-17, 0.1205366802553233113, 0.9927088740980539727 ) ) ;
#2222 = VERTEX_POINT ( 'NONE', #6304 ) ;
#2223 = EDGE_LOOP ( 'NONE', ( #35752, #2510, #22672, #6847 ) ) ;
#2224 = EDGE_CURVE ( 'NONE', #47240, #1828, #23907, .T. ) ;
#2225 = VERTEX_POINT ( 'NONE', #45231 ) ;
#2226 = LINE ( 'NONE', #18267, #50162 ) ;
#2227 = LINE ( 'NONE', #14318, #31906 ) ;
#2228 = AXIS2_PLACEMENT_3D ( 'NONE', #10978, #49900, #2056 ) ;
#2229 = VECTOR ( 'NONE', #51703, 999.9999999999998863 ) ;
#2230 = EDGE_CURVE ( 'NONE', #41581, #27267, #31452, .T. ) ;
#2231 = EDGE_CURVE ( 'NONE', #3375, #11938, #14976, .T. ) ;
#2232 = CARTESIAN_POINT ( 'NONE',  ( -336.3521761649654422, -123.5000000000000284, 0.000000000000000000 ) ) ;
#2233 = CARTESIAN_POINT ( 'NONE',  ( -330.4913330509368166, -171.7720157143599238, 33.92731199008539278 ) ) ;
#2234 = ORIENTED_EDGE ( 'NONE', *, *, #2553, .T. ) ;
#2235 = VECTOR ( 'NONE', #22867, 999.9999999999998863 ) ;
#2236 = EDGE_CURVE ( 'NONE', #20990, #18846, #14455, .T. ) ;
#2237 = PLANE ( 'NONE',  #6429 ) ;
#2238 = EDGE_CURVE ( 'NONE', #49593, #17654, #22597, .T. ) ;
#2239 = ORIENTED_EDGE ( 'NONE', *, *, #33660, .T. ) ;
#2241 = VERTEX_POINT ( 'NONE', #14708 ) ;
#2240 = DIRECTION ( 'NONE',  ( -0.000000000000000000, 0.8854560256532141294, 0.4647231720437604574 ) ) ;
#2242 = AXIS2_PLACEMENT_3D ( 'NONE', #9038, #24282, #12444 ) ;
#2243 = EDGE_CURVE ( 'NONE', #38668, #12031, #16385, .T. ) ;
#2244 = DIRECTION ( 'NONE',  ( -0.05924062789372142729, 0.000000000000000000, 0.9982437317643209074 ) ) ;
#2245 = VECTOR ( 'NONE', #49696, 1000.000000000000000 ) ;
#2246 = DIRECTION ( 'NONE',  ( 0.000000000000000000, 1.000000000000000000, -0.000000000000000000 ) ) ;
#2247 = AXIS2_PLACEMENT_3D ( 'NONE', #18861, #2837, #43043 ) ;
#2248 = CIRCLE ( 'NONE', #8958, 125.0000000000000000 ) ;
#2249 = EDGE_CURVE ( 'NONE', #15667, #19112, #3129, .T. ) ;
#2250 = CARTESIAN_POINT ( 'NONE',  ( -330.4913330509368166, -74.65991953890876687, -33.10432812419148263 ) ) ;
#2251 = DIRECTION ( 'NONE',  ( 0.000000000000000000, 0.000000000000000000, 1.000000000000000000 ) ) ;
#2252 = ORIENTED_EDGE ( 'NONE', *, *, #23754, .F. ) ;
#2253 = CARTESIAN_POINT ( 'NONE',  ( -163.4524646452521210, -189.7472609257535510, 46.44493303993096589 ) ) ;
#2254 = AXIS2_PLACEMENT_3D ( 'NONE', #31687, #44306, #15153 ) ;
#2255 = ORIENTED_EDGE ( 'NONE', *, *, #31948, .T. ) ;
#2256 = ADVANCED_FACE ( 'NONE', ( #39376 ), #26517, .T. ) ;
#2257 = AXIS2_PLACEMENT_3D ( 'NONE', #20316, #616, #24522 ) ;
#2258 = ORIENTED_EDGE ( 'NONE', *, *, #635, .T. ) ;
#2259 = CARTESIAN_POINT ( 'NONE',  ( -48.71401279728984690, -193.5000000000000000, 0.9720229140804159673 ) ) ;
#2260 = DIRECTION ( 'NONE',  ( 1.000000000000000000, -0.000000000000000000, -0.000000000000000000 ) ) ;
#2261 = ORIENTED_EDGE ( 'NONE', *, *, #14771, .F. ) ;
#2262 = CARTESIAN_POINT ( 'NONE',  ( 11.61413489515541997, -183.6283474603465606, -109.6074810615842381 ) ) ;
#2263 = CARTESIAN_POINT ( 'NONE',  ( -47.63353074800702558, -193.5000000000000000, -0.5338233779647817423 ) ) ;
#2264 = PLANE ( 'NONE',  #5271 ) ;
#2265 = CARTESIAN_POINT ( 'NONE',  ( -336.3521761649654422, -65.12692710742291524, -8.732051761643681687 ) ) ;
#2266 = EDGE_CURVE ( 'NONE', #39640, #346, #7965, .T. ) ;
#2267 = CARTESIAN_POINT ( 'NONE',  ( 38.01517884164422867, -189.7472609257535510, -88.85232316304832523 ) ) ;
#2268 = ORIENTED_EDGE ( 'NONE', *, *, #32272, .F. ) ;
#2269 = AXIS2_PLACEMENT_3D ( 'NONE', #44005, #40052, #10918 ) ;
#2270 = VECTOR ( 'NONE', #4526, 1000.000000000000000 ) ;
#2271 = LINE ( 'NONE', #34324, #9966 ) ;
#2272 = ORIENTED_EDGE ( 'NONE', *, *, #7273, .F. ) ;
#2273 = VECTOR ( 'NONE', #50562, 999.9999999999998863 ) ;
#2274 = VERTEX_POINT ( 'NONE', #19166 ) ;
#2275 = CARTESIAN_POINT ( 'NONE',  ( -1.079983486989452192E-15, 45.00000000000000000, 0.000000000000000000 ) ) ;
#2276 = ORIENTED_EDGE ( 'NONE', *, *, #44355, .T. ) ;
#2277 = CYLINDRICAL_SURFACE ( 'NONE', #18436, 125.0000000000000000 ) ;
#2278 = VECTOR ( 'NONE', #33516, 1000.000000000000114 ) ;
#2279 = FACE_OUTER_BOUND ( 'NONE', #45736, .T. ) ;
#2280 = VECTOR ( 'NONE', #39192, 1000.000000000000227 ) ;
#2281 = LINE ( 'NONE', #22767, #40526 ) ;
#2282 = VERTEX_POINT ( 'NONE', #51234 ) ;
#2283 = CARTESIAN_POINT ( 'NONE',  ( -339.1964088526558498, -181.8741440471348483, -13.87297036558331520 ) ) ;
#2284 = AXIS2_PLACEMENT_3D ( 'NONE', #9800, #38156, #25827 ) ;
#2285 = CIRCLE ( 'NONE', #30784, 125.0000000000000000 ) ;
#2286 = ADVANCED_FACE ( 'NONE', ( #31495 ), #6574, .F. ) ;
#2287 = EDGE_CURVE ( 'NONE', #31475, #39687, #7343, .T. ) ;
#2288 = AXIS2_PLACEMENT_3D ( 'NONE', #31879, #16117, #32132 ) ;
#2289 = CARTESIAN_POINT ( 'NONE',  ( -336.3521761649654422, -126.1322888500942270, -59.00000000000001421 ) ) ;
#2290 = DIRECTION ( 'NONE',  ( 0.000000000000000000, 0.000000000000000000, 1.000000000000000000 ) ) ;
#2291 = EDGE_LOOP ( 'NONE', ( #40818, #35669, #44827, #5786 ) ) ;
#2292 = EDGE_LOOP ( 'NONE', ( #29245, #12023, #38810, #31381 ) ) ;
#2293 = ORIENTED_EDGE ( 'NONE', *, *, #29216, .T. ) ;
#2294 = VECTOR ( 'NONE', #6582, 1000.000000000000114 ) ;
#2295 = DIRECTION ( 'NONE',  ( 0.000000000000000000, 1.000000000000000000, -0.000000000000000000 ) ) ;
#2296 = DIRECTION ( 'NONE',  ( 0.000000000000000000, 0.000000000000000000, 1.000000000000000000 ) ) ;
#2297 = LINE ( 'NONE', #45937, #22604 ) ;
#2298 = LINE ( 'NONE', #18060, #28679 ) ;
#2299 = DIRECTION ( 'NONE',  ( 0.000000000000000000, -0.000000000000000000, -1.000000000000000000 ) ) ;
#2300 = ORIENTED_EDGE ( 'NONE', *, *, #37534, .T. ) ;
#2301 = FACE_OUTER_BOUND ( 'NONE', #27373, .T. ) ;
#2302 = ORIENTED_EDGE ( 'NONE', *, *, #8732, .T. ) ;
#2304 = ORIENTED_EDGE ( 'NONE', *, *, #9191, .T. ) ;
#2303 = CARTESIAN_POINT ( 'NONE',  ( -213.8817838414232426, -213.5000000000000000, 2.819679052520814125E-14 ) ) ;
#2305 = VECTOR ( 'NONE', #5936, 1000.000000000000227 ) ;
#2306 = ORIENTED_EDGE ( 'NONE', *, *, #30099, .F. ) ;
#2307 = VECTOR ( 'NONE', #39160, 1000.000000000000000 ) ;
#2308 = FACE_OUTER_BOUND ( 'NONE', #28245, .T. ) ;
#2309 = EDGE_CURVE ( 'NONE', #3221, #17784, #23371, .T. ) ;
#2310 = VERTEX_POINT ( 'NONE', #38610 ) ;
#2311 = PLANE ( 'NONE',  #21612 ) ;
#2312 = VERTEX_POINT ( 'NONE', #11002 ) ;
#2313 = AXIS2_PLACEMENT_3D ( 'NONE', #18632, #34644, #50691 ) ;
#2314 = FACE_OUTER_BOUND ( 'NONE', #26511, .T. ) ;
#2315 = CARTESIAN_POINT ( 'NONE',  ( -336.3521761649654422, -182.5000000000000568, 2.632288850093980503 ) ) ;
#2316 = VERTEX_POINT ( 'NONE', #31235 ) ;
#2317 = DIRECTION ( 'NONE',  ( -0.9473263538541899509, 0.000000000000000000, -0.3202698538628415692 ) ) ;
#2318 = EDGE_LOOP ( 'NONE', ( #43891, #46362, #7589, #50847 ) ) ;
#2319 = EDGE_CURVE ( 'NONE', #23283, #13008, #37350, .T. ) ;
#2320 = EDGE_LOOP ( 'NONE', ( #363, #35446, #1659, #50731 ) ) ;
#2321 = CARTESIAN_POINT ( 'NONE',  ( -159.0901268547125653, -177.1207230881787780, 58.22548115875957109 ) ) ;
#2322 = VECTOR ( 'NONE', #598, 1000.000000000000000 ) ;
#2323 = LINE ( 'NONE', #26474, #22249 ) ;
#2324 = VECTOR ( 'NONE', #28642, 1000.000000000000000 ) ;
#2325 = CARTESIAN_POINT ( 'NONE',  ( -55.05561436132770581, -193.5000000000000000, 124.8268793598474105 ) ) ;
#2326 = DIRECTION ( 'NONE',  ( 1.000000000000000000, -0.000000000000000000, -0.000000000000000000 ) ) ;
#2327 = EDGE_LOOP ( 'NONE', ( #48897, #47615, #28463, #49873 ) ) ;
#2328 = VECTOR ( 'NONE', #22791, 1000.000000000000227 ) ;
#2329 = CARTESIAN_POINT ( 'NONE',  ( -330.4913330509368166, -175.5095439275173419, 27.86139516340933042 ) ) ;
#2330 = CARTESIAN_POINT ( 'NONE',  ( -336.3521761649654422, -182.5000000000000568, 1.632288850093980725 ) ) ;
#2331 = CARTESIAN_POINT ( 'NONE',  ( -336.3521761649654422, -65.58448481710581746, 11.56382487286456140 ) ) ;
#2332 = CARTESIAN_POINT ( 'NONE',  ( 0.000000000000000000, -53.50000000000000000, -16.00000000000000000 ) ) ;
#2333 = AXIS2_PLACEMENT_3D ( 'NONE', #48336, #4193, #32029 ) ;
#2334 = ORIENTED_EDGE ( 'NONE', *, *, #40185, .T. ) ;
#2335 = LINE ( 'NONE', #18363, #24656 ) ;
#2336 = DIRECTION ( 'NONE',  ( -0.9027978299657446470, 0.000000000000000000, 0.4300652022765183435 ) ) ;
#2337 = CIRCLE ( 'NONE', #31691, 125.0000000000000000 ) ;
#2338 = CARTESIAN_POINT ( 'NONE',  ( -48.47912675150885065, -183.6283474603465606, 6.938893903907228378E-15 ) ) ;
#2339 = ORIENTED_EDGE ( 'NONE', *, *, #30188, .T. ) ;
#2340 = DIRECTION ( 'NONE',  ( 0.000000000000000000, 0.000000000000000000, 1.000000000000000000 ) ) ;
#2341 = CARTESIAN_POINT ( 'NONE',  ( -49.08592689732743963, -193.5000000000000000, -0.7948544414133539293 ) ) ;
#2342 = VERTEX_POINT ( 'NONE', #11259 ) ;
#2343 = DIRECTION ( 'NONE',  ( -0.000000000000000000, 1.000000000000000000, -0.000000000000000000 ) ) ;
#2344 = VERTEX_POINT ( 'NONE', #27292 ) ;
#2345 = VECTOR ( 'NONE', #42432, 1000.000000000000000 ) ;
#2346 = CARTESIAN_POINT ( 'NONE',  ( 0.000000000000000000, -79.33786585790510060, -39.12423683620700388 ) ) ;
#2347 = VECTOR ( 'NONE', #35707, 1000.000000000000000 ) ;
#2348 = DIRECTION ( 'NONE',  ( -0.9374196611341254481, 0.000000000000000000, 0.3482016354343867026 ) ) ;
#2349 = DIRECTION ( 'NONE',  ( -0.000000000000000000, -0.7485107481711046340, -0.6631226582407911962 ) ) ;
#2350 = AXIS2_PLACEMENT_3D ( 'NONE', #11123, #46898, #50569 ) ;
#2351 = DIRECTION ( 'NONE',  ( -0.000000000000000000, 0.000000000000000000, -1.000000000000000000 ) ) ;
#2352 = EDGE_CURVE ( 'NONE', #2690, #11626, #43071, .T. ) ;
#2353 = DIRECTION ( 'NONE',  ( -1.000000000000000000, -4.850383327711956209E-15, -9.241633304753555563E-15 ) ) ;
#2354 = ORIENTED_EDGE ( 'NONE', *, *, #19015, .F. ) ;
#2355 = DIRECTION ( 'NONE',  ( 0.000000000000000000, 0.7485107481711046340, 0.6631226582407911962 ) ) ;
#2356 = ORIENTED_EDGE ( 'NONE', *, *, #41519, .F. ) ;
#2357 = DIRECTION ( 'NONE',  ( 0.000000000000000000, -0.5680647467311540355, 0.8229838658936575735 ) ) ;
#2358 = VECTOR ( 'NONE', #40582, 1000.000000000000000 ) ;
#2359 = ORIENTED_EDGE ( 'NONE', *, *, #51003, .T. ) ;
#2360 = CARTESIAN_POINT ( 'NONE',  ( -117.6201219941651601, -189.7472609257535510, 104.1370384486469902 ) ) ;
#2361 = VECTOR ( 'NONE', #24717, 1000.000000000000000 ) ;
#2362 = CARTESIAN_POINT ( 'NONE',  ( -332.3517673607765914, -182.5000000000000568, 1.632288850093980725 ) ) ;
#2363 = DIRECTION ( 'NONE',  ( 0.000000000000000000, 0.000000000000000000, -1.000000000000000000 ) ) ;
#2364 = ORIENTED_EDGE ( 'NONE', *, *, #28169, .F. ) ;
#2367 = ORIENTED_EDGE ( 'NONE', *, *, #31110, .T. ) ;
#2366 = DIRECTION ( 'NONE',  ( 0.000000000000000000, 0.000000000000000000, 1.000000000000000000 ) ) ;
#2365 = CARTESIAN_POINT ( 'NONE',  ( -0.5864338395290236150, 50.61667155555193887, -21.34634502027464364 ) ) ;
#2368 = EDGE_CURVE ( 'NONE', #27409, #46293, #27248, .T. ) ;
#2369 = MANIFOLD_SOLID_BREP ( 'CirPattern2', #43848 ) ;
#2370 = DIRECTION ( 'NONE',  ( -0.000000000000000000, 1.000000000000000000, -0.000000000000000000 ) ) ;
#2371 = ORIENTED_EDGE ( 'NONE', *, *, #35913, .T. ) ;
#2372 = DIRECTION ( 'NONE',  ( 0.000000000000000000, -1.000000000000000000, 0.000000000000000000 ) ) ;
#2373 = ORIENTED_EDGE ( 'NONE', *, *, #28707, .F. ) ;
#2374 = LINE ( 'NONE', #50719, #16669 ) ;
#2377 = EDGE_LOOP ( 'NONE', ( #25299, #3325, #5231, #11655 ) ) ;
#2376 = CARTESIAN_POINT ( 'NONE',  ( -47.74129347246712740, -193.5000000000000000, -0.6749830015182022303 ) ) ;
#2375 = DIRECTION ( 'NONE',  ( 0.000000000000000000, 0.3546048870425267951, -0.9350162426854181641 ) ) ;
#2378 = VERTEX_POINT ( 'NONE', #24649 ) ;
#2379 = DIRECTION ( 'NONE',  ( -0.000000000000000000, 0.8854560256532093554, -0.4647231720437695057 ) ) ;
#2380 =( GEOMETRIC_REPRESENTATION_CONTEXT ( 3 ) GLOBAL_UNCERTAINTY_ASSIGNED_CONTEXT ( ( #14323 ) ) GLOBAL_UNIT_ASSIGNED_CONTEXT ( ( #38381, #17900, #46534 ) ) REPRESENTATION_CONTEXT ( 'NONE', 'WORKASPACE' ) );
#2381 = ORIENTED_EDGE ( 'NONE', *, *, #926, .F. ) ;
#2382 = FACE_OUTER_BOUND ( 'NONE', #48470, .T. ) ;
#2383 = VECTOR ( 'NONE', #39835, 1000.000000000000114 ) ;
#2384 = LINE ( 'NONE', #10505, #39086 ) ;
#2385 = ORIENTED_EDGE ( 'NONE', *, *, #50042, .F. ) ;
#2386 = CARTESIAN_POINT ( 'NONE',  ( -332.3517673607765914, -142.8954717479169574, 55.74477592174805096 ) ) ;
#2387 = FACE_OUTER_BOUND ( 'NONE', #33565, .T. ) ;
#2388 = FACE_OUTER_BOUND ( 'NONE', #37197, .T. ) ;
#2389 = DIRECTION ( 'NONE',  ( 0.000000000000000000, 0.000000000000000000, 1.000000000000000000 ) ) ;
#2390 = VECTOR ( 'NONE', #35749, 1000.000000000000114 ) ;
#2391 = DIRECTION ( 'NONE',  ( 0.05924062789370006937, 0.000000000000000000, 0.9982437317643222396 ) ) ;
#2392 = ORIENTED_EDGE ( 'NONE', *, *, #3355, .T. ) ;
#2393 = CARTESIAN_POINT ( 'NONE',  ( -47.97059563285962724, -193.5000000000000000, -0.8610436117673480050 ) ) ;
#2394 = FACE_OUTER_BOUND ( 'NONE', #9117, .T. ) ;
#2395 = FACE_OUTER_BOUND ( 'NONE', #31810, .T. ) ;
#2396 = ORIENTED_EDGE ( 'NONE', *, *, #26685, .F. ) ;
#2397 = VECTOR ( 'NONE', #6564, 1000.000000000000000 ) ;
#2398 = DIRECTION ( 'NONE',  ( 0.000000000000000000, -0.000000000000000000, -1.000000000000000000 ) ) ;
#2399 = CARTESIAN_POINT ( 'NONE',  ( -339.1964088526558498, -172.3400804610910200, 33.10432812419180948 ) ) ;
#2400 = CARTESIAN_POINT ( 'NONE',  ( -330.4913330509368166, -96.06030588028409056, 53.35787839313353231 ) ) ;
#2401 = EDGE_CURVE ( 'NONE', #5376, #7178, #22844, .T. ) ;
#2402 = CARTESIAN_POINT ( 'NONE',  ( -48.07600332222087758, -193.5000000000000000, -0.9151456172430111335 ) ) ;
#2403 = ORIENTED_EDGE ( 'NONE', *, *, #46389, .F. ) ;
#2405 = VECTOR ( 'NONE', #32806, 1000.000000000000000 ) ;
#2404 = DIRECTION ( 'NONE',  ( 0.000000000000000000, -1.000000000000000000, 0.000000000000000000 ) ) ;
#2406 = ADVANCED_FACE ( 'NONE', ( #24150 ), #28328, .F. ) ;
#2407 = CARTESIAN_POINT ( 'NONE',  ( 75.27070168362158142, -189.7472609257535510, 17.63462396184792524 ) ) ;
#2408 = CARTESIAN_POINT ( 'NONE',  ( -339.1964088526558498, -123.5000000000000284, 0.000000000000000000 ) ) ;
#2409 = CARTESIAN_POINT ( 'NONE',  ( -164.0008810331606526, -175.3837268820161057, 47.74645837849825369 ) ) ;
#2410 = EDGE_LOOP ( 'NONE', ( #3687, #37134, #46087, #48529 ) ) ;
#2411 = EDGE_CURVE ( 'NONE', #44450, #14966, #12990, .T. ) ;
#2412 = DIRECTION ( 'NONE',  ( -0.000000000000000000, 0.9709418174260519008, -0.2393156642875582940 ) ) ;
#2413 = ADVANCED_FACE ( 'NONE', ( #20189 ), #44382, .F. ) ;
#2414 = DIRECTION ( 'NONE',  ( -0.000000000000000000, 1.000000000000000000, -0.000000000000000000 ) ) ;
#2415 = ORIENTED_EDGE ( 'NONE', *, *, #3504, .T. ) ;
#2416 = VECTOR ( 'NONE', #22994, 1000.000000000000000 ) ;
#2417 = ORIENTED_EDGE ( 'NONE', *, *, #27189, .T. ) ;
#2418 = EDGE_CURVE ( 'NONE', #24544, #32491, #3911, .T. ) ;
#2419 = VECTOR ( 'NONE', #49094, 1000.000000000000000 ) ;
#2420 = VERTEX_POINT ( 'NONE', #36213 ) ;
#2421 = CARTESIAN_POINT ( 'NONE',  ( -158.0280232639029236, -193.5000000000000000, 60.19999396110247147 ) ) ;
#2422 = VECTOR ( 'NONE', #45411, 1000.000000000000000 ) ;
#2423 = DIRECTION ( 'NONE',  ( 0.000000000000000000, 0.000000000000000000, 1.000000000000000000 ) ) ;
#2424 = PLANE ( 'NONE',  #5374 ) ;
#2425 = ORIENTED_EDGE ( 'NONE', *, *, #7091, .T. ) ;
#2426 = CARTESIAN_POINT ( 'NONE',  ( 46.00000000000000000, 20.00000000000000000, 0.000000000000000000 ) ) ;
#2427 = DIRECTION ( 'NONE',  ( 0.000000000000000000, 0.000000000000000000, 1.000000000000000000 ) ) ;
#2428 = VECTOR ( 'NONE', #37249, 1000.000000000000114 ) ;
#2431 = VERTEX_POINT ( 'NONE', #52017 ) ;
#2430 = CARTESIAN_POINT ( 'NONE',  ( -150.5215542367829755, -189.7472609257535510, -72.19655804061973470 ) ) ;
#2429 = CARTESIAN_POINT ( 'NONE',  ( -48.47912675150885065, -189.7472609257535510, 6.938893903907228378E-15 ) ) ;
#2432 = EDGE_CURVE ( 'NONE', #13215, #8540, #31769, .T. ) ;
#2433 = DIRECTION ( 'NONE',  ( 0.9960498426152165630, 0.000000000000000000, 0.08879589532293852283 ) ) ;
#2434 = ORIENTED_EDGE ( 'NONE', *, *, #47338, .T. ) ;
#2435 = PLANE ( 'NONE',  #3718 ) ;
#2436 = ORIENTED_EDGE ( 'NONE', *, *, #40280, .T. ) ;
#2437 = DIRECTION ( 'NONE',  ( 0.000000000000000000, -1.000000000000000000, -0.000000000000000000 ) ) ;
#2438 = LINE ( 'NONE', #50784, #43914 ) ;
#2439 = DIRECTION ( 'NONE',  ( 0.000000000000000000, -1.000000000000000000, -0.000000000000000000 ) ) ;
#2440 = AXIS2_PLACEMENT_3D ( 'NONE', #20656, #695, #36165 ) ;
#2441 = ORIENTED_EDGE ( 'NONE', *, *, #7273, .T. ) ;
#2442 = CARTESIAN_POINT ( 'NONE',  ( -162.7543581613524282, -193.5000000000000000, 50.65739320402010293 ) ) ;
#2443 = LINE ( 'NONE', #10574, #12410 ) ;
#2444 = ORIENTED_EDGE ( 'NONE', *, *, #2059, .F. ) ;
#2445 = CARTESIAN_POINT ( 'NONE',  ( -112.1919339979530150, -189.7472609257535510, 107.5438431188761825 ) ) ;
#2446 = DIRECTION ( 'NONE',  ( 0.3482016354344059095, 0.000000000000000000, -0.9374196611341183427 ) ) ;
#2447 = ORIENTED_EDGE ( 'NONE', *, *, #9720, .T. ) ;
#2448 = FACE_BOUND ( 'NONE', #44907, .T. ) ;
#2449 = CARTESIAN_POINT ( 'NONE',  ( 32.59960422616970988, -193.5000000000000000, -93.82025162277999186 ) ) ;
#2450 = ORIENTED_EDGE ( 'NONE', *, *, #21802, .T. ) ;
#2451 = DIRECTION ( 'NONE',  ( -0.000000000000000000, -1.000000000000000000, 0.000000000000000000 ) ) ;
#2452 = EDGE_LOOP ( 'NONE', ( #5930, #14011, #3673, #38104 ) ) ;
#2453 = VECTOR ( 'NONE', #3108, 1000.000000000000000 ) ;
#2454 = CARTESIAN_POINT ( 'NONE',  ( -168.1141659785444915, -183.6283474603465606, -36.22785377503947046 ) ) ;
#2455 = CARTESIAN_POINT ( 'NONE',  ( -305.0000000000000568, -177.7994952405510389, -25.52576769896207409 ) ) ;
#2456 = ORIENTED_EDGE ( 'NONE', *, *, #39642, .F. ) ;
#2457 = MECHANICAL_DESIGN_GEOMETRIC_PRESENTATION_REPRESENTATION (  '', ( #36817 ), #33523 ) ;
#2458 = LINE ( 'NONE', #26361, #47528 ) ;
#2459 = ADVANCED_FACE ( 'NONE', ( #32011 ), #39883, .T. ) ;
#2460 = CARTESIAN_POINT ( 'NONE',  ( -66.64622755927952369, -183.6283474603465606, 123.6727797384707372 ) ) ;
#2461 = DIRECTION ( 'NONE',  ( -0.000000000000000000, 0.8229838658936556861, -0.5680647467311569221 ) ) ;
#2462 = EDGE_CURVE ( 'NONE', #3624, #9307, #32539, .T. ) ;
#2463 = ORIENTED_EDGE ( 'NONE', *, *, #47204, .F. ) ;
#2464 = CARTESIAN_POINT ( 'NONE',  ( -124.9871112439422092, -189.7472609257535510, -98.85104101073275729 ) ) ;
#2465 = ORIENTED_EDGE ( 'NONE', *, *, #39109, .F. ) ;
#2466 = DIRECTION ( 'NONE',  ( 0.3482016354343995812, 0.000000000000000000, -0.9374196611341205632 ) ) ;
#2467 = DIRECTION ( 'NONE',  ( -0.000000000000000000, 1.000000000000000000, -0.000000000000000000 ) ) ;
#2469 = EDGE_LOOP ( 'NONE', ( #25496, #25820, #13141, #4705 ) ) ;
#2468 = CARTESIAN_POINT ( 'NONE',  ( -365.0000000000001137, -78.50000000000002842, 10.00000000000000711 ) ) ;
#2470 = ORIENTED_EDGE ( 'NONE', *, *, #37212, .F. ) ;
#2471 = DIRECTION ( 'NONE',  ( -0.8757349421956310831, 0.000000000000000000, -0.4827922027307550712 ) ) ;
#2472 = ADVANCED_FACE ( 'NONE', ( #44104 ), #40404, .T. ) ;
#2473 = ADVANCED_FACE ( 'NONE', ( #8618 ), #40662, .F. ) ;
#2474 = CIRCLE ( 'NONE', #15910, 125.0000000000000000 ) ;
#2475 = LINE ( 'NONE', #10869, #39680 ) ;
#2476 = ORIENTED_EDGE ( 'NONE', *, *, #18009, .F. ) ;
#2477 = EDGE_CURVE ( 'NONE', #17289, #7125, #26422, .T. ) ;
#2478 = LINE ( 'NONE', #3492, #22267 ) ;
#2479 = ORIENTED_EDGE ( 'NONE', *, *, #18877, .F. ) ;
#2480 = CARTESIAN_POINT ( 'NONE',  ( -105.4063847101409692, -193.5000000000000000, -111.2847127925096231 ) ) ;
#2481 = LINE ( 'NONE', #51111, #38427 ) ;
#2482 = ADVANCED_FACE ( 'NONE', ( #12815 ), #27803, .T. ) ;
#2483 = CARTESIAN_POINT ( 'NONE',  ( -48.47912675150885065, -175.3837268820161057, 6.938893903907228378E-15 ) ) ;
#2484 = CARTESIAN_POINT ( 'NONE',  ( -332.3517673607765914, -153.2494431741581025, -51.01861988938816950 ) ) ;
#2485 = VERTEX_POINT ( 'NONE', #24920 ) ;
#2486 = ORIENTED_EDGE ( 'NONE', *, *, #26176, .T. ) ;
#2487 = ORIENTED_EDGE ( 'NONE', *, *, #30184, .F. ) ;
#2488 = FACE_OUTER_BOUND ( 'NONE', #4253, .T. ) ;
#2489 = CARTESIAN_POINT ( 'NONE',  ( -140.8230258362169707, -193.5000000000000000, 84.24728067916045404 ) ) ;
#2490 = AXIS2_PLACEMENT_3D ( 'NONE', #7512, #26951, #23532 ) ;
#2491 = DIRECTION ( 'NONE',  ( -1.000000000000000000, 0.000000000000000000, 0.000000000000000000 ) ) ;
#2492 = CARTESIAN_POINT ( 'NONE',  ( -48.47912675150885065, -183.6283474603465606, 6.938893903907228378E-15 ) ) ;
#2493 = ORIENTED_EDGE ( 'NONE', *, *, #18568, .T. ) ;
#2494 = CIRCLE ( 'NONE', #9212, 4.999999999999997335 ) ;
#2495 = VERTEX_POINT ( 'NONE', #7839 ) ;
#2496 = ORIENTED_EDGE ( 'NONE', *, *, #2352, .F. ) ;
#2497 = DIRECTION ( 'NONE',  ( 1.000000000000000000, 0.000000000000000000, -0.000000000000000000 ) ) ;
#2498 = LINE ( 'NONE', #6957, #12376 ) ;
#2499 = DIRECTION ( 'NONE',  ( 0.000000000000000000, 0.000000000000000000, 1.000000000000000000 ) ) ;
#2500 = DIRECTION ( 'NONE',  ( -1.000000000000000000, -0.000000000000000000, 0.000000000000000000 ) ) ;
#2501 = PLANE ( 'NONE',  #37696 ) ;
#2502 = EDGE_LOOP ( 'NONE', ( #48239, #12553, #26115, #45439 ) ) ;
#2503 = DIRECTION ( 'NONE',  ( -1.000000000000000000, 0.000000000000000000, 0.000000000000000000 ) ) ;
#2504 = VECTOR ( 'NONE', #19863, 1000.000000000000000 ) ;
#2505 = EDGE_CURVE ( 'NONE', #14785, #35111, #40937, .T. ) ;
#2506 = APPLICATION_CONTEXT ( 'automotive_design' ) ;
#2507 = VERTEX_POINT ( 'NONE', #4961 ) ;
#2508 = LINE ( 'NONE', #42958, #48072 ) ;
#2509 = CARTESIAN_POINT ( 'NONE',  ( 41.41233698655026529, -177.1207230881787780, 86.85922373029363541 ) ) ;
#2510 = ORIENTED_EDGE ( 'NONE', *, *, #44355, .F. ) ;
#2511 = EDGE_CURVE ( 'NONE', #29270, #18052, #20980, .T. ) ;
#2512 = DIRECTION ( 'NONE',  ( -0.000000000000000000, 1.000000000000000000, -0.000000000000000000 ) ) ;
#2513 = ADVANCED_FACE ( 'NONE', ( #22007 ), #1771, .T. ) ;
#2514 = PLANE ( 'NONE',  #44018 ) ;
#2515 = DIRECTION ( 'NONE',  ( 0.000000000000000000, -0.000000000000000000, -1.000000000000000000 ) ) ;
#2516 = EDGE_CURVE ( 'NONE', #23682, #37758, #30616, .T. ) ;
#2517 = DIRECTION ( 'NONE',  ( 0.000000000000000000, -1.000000000000000000, 0.000000000000000000 ) ) ;
#2518 = ADVANCED_FACE ( 'NONE', ( #33831 ), #25949, .F. ) ;
#2519 = CARTESIAN_POINT ( 'NONE',  ( -336.3521761649654422, -181.1761995186066088, -12.53476669029101842 ) ) ;
#2520 = EDGE_LOOP ( 'NONE', ( #49314, #26680, #12572, #49787 ) ) ;
#2521 = AXIS2_PLACEMENT_3D ( 'NONE', #48638, #40455, #32587 ) ;
#2522 = EDGE_CURVE ( 'NONE', #28521, #34600, #21239, .T. ) ;
#2523 = CARTESIAN_POINT ( 'NONE',  ( 76.47090317495664635, -175.3837268820161057, -3.534122433557446374 ) ) ;
#2524 = ORIENTED_EDGE ( 'NONE', *, *, #17558, .T. ) ;
#2525 = ORIENTED_EDGE ( 'NONE', *, *, #11768, .T. ) ;
#2526 = DIRECTION ( 'NONE',  ( 0.000000000000000000, 1.000000000000000000, -0.000000000000000000 ) ) ;
#2527 = EDGE_CURVE ( 'NONE', #44388, #35955, #51650, .T. ) ;
#2528 = ORIENTED_EDGE ( 'NONE', *, *, #33555, .F. ) ;
#2529 = ADVANCED_FACE ( 'NONE', ( #45172 ), #5742, .F. ) ;
#2530 = CARTESIAN_POINT ( 'NONE',  ( -339.1964088526558498, -123.5000000000000284, 0.000000000000000000 ) ) ;
#2531 = EDGE_LOOP ( 'NONE', ( #1201, #45244, #13783, #20748 ) ) ;
#2532 = EDGE_CURVE ( 'NONE', #25859, #10098, #455, .T. ) ;
#2533 = CARTESIAN_POINT ( 'NONE',  ( -49.38192458147459263, -193.5000000000000000, -0.4300652022765235616 ) ) ;
#2534 = PLANE ( 'NONE',  #11165 ) ;
#2535 = ORIENTED_EDGE ( 'NONE', *, *, #8208, .F. ) ;
#2536 = DIRECTION ( 'NONE',  ( 0.000000000000000000, -1.000000000000000000, 0.000000000000000000 ) ) ;
#2537 = ADVANCED_FACE ( 'NONE', ( #49871 ), #18068, .F. ) ;
#2538 = LINE ( 'NONE', #43246, #5122 ) ;
#2539 = DIRECTION ( 'NONE',  ( 0.000000000000000000, 0.000000000000000000, -1.000000000000000000 ) ) ;
#2540 = ORIENTED_EDGE ( 'NONE', *, *, #21536, .F. ) ;
#2541 = EDGE_LOOP ( 'NONE', ( #42345, #44908, #36123, #29624 ) ) ;
#2542 = EDGE_CURVE ( 'NONE', #39427, #44067, #45945, .T. ) ;
#2543 = VECTOR ( 'NONE', #46906, 1000.000000000000000 ) ;
#2545 = VERTEX_POINT ( 'NONE', #29107 ) ;
#2544 = AXIS2_PLACEMENT_3D ( 'NONE', #5844, #10530, #13704 ) ;
#2546 = EDGE_CURVE ( 'NONE', #46197, #47219, #50829, .T. ) ;
#2547 = DIRECTION ( 'NONE',  ( -0.000000000000000000, 1.000000000000000000, -0.000000000000000000 ) ) ;
#2548 = DIRECTION ( 'NONE',  ( 0.8124868780056825335, 0.000000000000000000, -0.5829794791144703447 ) ) ;
#2549 = DIRECTION ( 'NONE',  ( 0.000000000000000000, 0.5680647467311510379, -0.8229838658936596829 ) ) ;
#2550 = DIRECTION ( 'NONE',  ( 0.000000000000000000, 0.000000000000000000, 1.000000000000000000 ) ) ;
#2551 = CARTESIAN_POINT ( 'NONE',  ( -173.0003472773501301, -193.5000000000000000, 10.93003379476953363 ) ) ;
#2552 = VERTEX_POINT ( 'NONE', #37773 ) ;
#2553 = EDGE_CURVE ( 'NONE', #37393, #9572, #24779, .T. ) ;
#2554 = DIRECTION ( 'NONE',  ( 0.000000000000000000, 0.000000000000000000, 1.000000000000000000 ) ) ;
#2555 = ORIENTED_EDGE ( 'NONE', *, *, #23636, .T. ) ;
#2557 = ORIENTED_EDGE ( 'NONE', *, *, #32057, .F. ) ;
#2556 = CARTESIAN_POINT ( 'NONE',  ( -330.4913330509368166, -116.8846903019842927, 58.63009191191280678 ) ) ;
#2558 = ORIENTED_EDGE ( 'NONE', *, *, #42644, .F. ) ;
#2559 = AXIS2_PLACEMENT_3D ( 'NONE', #25166, #40920, #28315 ) ;
#2560 = DIRECTION ( 'NONE',  ( -0.000000000000000000, 1.000000000000000000, -0.000000000000000000 ) ) ;
#2561 = ORIENTED_EDGE ( 'NONE', *, *, #40726, .F. ) ;
#2562 = LINE ( 'NONE', #50400, #3133 ) ;
#2563 = LINE ( 'NONE', #30161, #47203 ) ;
#2564 = FACE_OUTER_BOUND ( 'NONE', #15807, .T. ) ;
#2565 = ORIENTED_EDGE ( 'NONE', *, *, #37242, .T. ) ;
#2566 = DIRECTION ( 'NONE',  ( 0.000000000000000000, -1.000000000000000000, -0.000000000000000000 ) ) ;
#2567 = ORIENTED_EDGE ( 'NONE', *, *, #23366, .F. ) ;
#2568 = ORIENTED_EDGE ( 'NONE', *, *, #36896, .T. ) ;
#2569 = CARTESIAN_POINT ( 'NONE',  ( 45.24245851652180761, -177.1207230881787780, -81.19354792697733103 ) ) ;
#2570 = CARTESIAN_POINT ( 'NONE',  ( -173.3968853974275817, -189.7472609257535510, 4.533605064404172325 ) ) ;
#2571 = FACE_OUTER_BOUND ( 'NONE', #38785, .T. ) ;
#2572 = ORIENTED_EDGE ( 'NONE', *, *, #5502, .T. ) ;
#2573 = LINE ( 'NONE', #2329, #4743 ) ;
#2574 = DIRECTION ( 'NONE',  ( -0.000000000000000000, -1.000000000000000000, -0.000000000000000000 ) ) ;
#2575 = EDGE_CURVE ( 'NONE', #11294, #18907, #49367, .T. ) ;
#2576 = EDGE_CURVE ( 'NONE', #32690, #4224, #9411, .T. ) ;
#2577 = LINE ( 'NONE', #30677, #17965 ) ;
#2578 = DIRECTION ( 'NONE',  ( 0.000000000000000000, 0.9350162426854107256, -0.3546048870425463906 ) ) ;
#2579 = VERTEX_POINT ( 'NONE', #42225 ) ;
#2580 = LINE ( 'NONE', #26748, #34707 ) ;
#2581 = FACE_OUTER_BOUND ( 'NONE', #41266, .T. ) ;
#2582 = VECTOR ( 'NONE', #32320, 1000.000000000000000 ) ;
#2583 = EDGE_CURVE ( 'NONE', #35261, #563, #6240, .T. ) ;
#2584 = AXIS2_PLACEMENT_3D ( 'NONE', #9700, #14426, #14179 ) ;
#2585 = EDGE_CURVE ( 'NONE', #48198, #41229, #13603, .T. ) ;
#2586 = FACE_OUTER_BOUND ( 'NONE', #750, .T. ) ;
#2587 = ORIENTED_EDGE ( 'NONE', *, *, #23706, .F. ) ;
#2588 = CARTESIAN_POINT ( 'NONE',  ( -339.1964088526558498, -175.9742670995610752, 26.97593913775620678 ) ) ;
#2589 = CARTESIAN_POINT ( 'NONE',  ( 0.000000000000000000, 0.000000000000000000, 0.000000000000000000 ) ) ;
#2590 = ORIENTED_EDGE ( 'NONE', *, *, #36258, .T. ) ;
#2591 = DIRECTION ( 'NONE',  ( 0.7378332790417189146, 0.000000000000000000, 0.6749830015182196608 ) ) ;
#2592 = VERTEX_POINT ( 'NONE', #46198 ) ;
#2593 = DIRECTION ( 'NONE',  ( -0.000000000000000000, 1.000000000000000000, -0.000000000000000000 ) ) ;
#2594 = AXIS2_PLACEMENT_3D ( 'NONE', #32463, #36929, #16183 ) ;
#2595 = EDGE_CURVE ( 'NONE', #32858, #10769, #10175, .T. ) ;
#2596 = CARTESIAN_POINT ( 'NONE',  ( -48.98765787015808115, -177.1207230881787780, 0.8610436117673582190 ) ) ;
#2597 = LINE ( 'NONE', #42796, #48093 ) ;
#2598 = CARTESIAN_POINT ( 'NONE',  ( 76.52053249983504202, -177.1207230881787780, -0.2918682030015415929 ) ) ;
#2599 = LINE ( 'NONE', #25996, #3345 ) ;
#2600 = EDGE_LOOP ( 'NONE', ( #29938, #35646, #9190, #20573 ) ) ;
#2601 = EDGE_CURVE ( 'NONE', #25289, #18828, #36550, .T. ) ;
#2602 = CARTESIAN_POINT ( 'NONE',  ( -336.3521761649654422, -168.7445418633863596, -37.90245108779149064 ) ) ;
#2603 = ORIENTED_EDGE ( 'NONE', *, *, #4774, .T. ) ;
#2604 = DIRECTION ( 'NONE',  ( -1.000000000000000000, 0.000000000000000000, 0.000000000000000000 ) ) ;
#2605 = ORIENTED_EDGE ( 'NONE', *, *, #15077, .T. ) ;
#2606 = LINE ( 'NONE', #2360, #6627 ) ;
#2607 = CIRCLE ( 'NONE', #31972, 125.0000000000000000 ) ;
#2608 = VECTOR ( 'NONE', #8345, 1000.000000000000000 ) ;
#2609 = LINE ( 'NONE', #18393, #50257 ) ;
#2610 = LINE ( 'NONE', #46507, #25614 ) ;
#2611 = ORIENTED_EDGE ( 'NONE', *, *, #31301, .T. ) ;
#2614 = ORIENTED_EDGE ( 'NONE', *, *, #31482, .F. ) ;
#2613 = DIRECTION ( 'NONE',  ( 0.000000000000000000, -1.000000000000000000, 0.000000000000000000 ) ) ;
#2612 = CARTESIAN_POINT ( 'NONE',  ( -1.230335819511603423, -177.1207230881787780, 115.7261930397108216 ) ) ;
#2615 = LINE ( 'NONE', #18652, #31489 ) ;
#2616 = ORIENTED_EDGE ( 'NONE', *, *, #33444, .F. ) ;
#2617 = DIRECTION ( 'NONE',  ( 0.000000000000000000, 0.000000000000000000, 1.000000000000000000 ) ) ;
#2618 = ORIENTED_EDGE ( 'NONE', *, *, #38250, .F. ) ;
#2619 = CYLINDRICAL_SURFACE ( 'NONE', #46048, 125.0000000000000000 ) ;
#2622 = VERTEX_POINT ( 'NONE', #10697 ) ;
#2621 = DIRECTION ( 'NONE',  ( -0.000000000000000000, 1.000000000000000000, -0.000000000000000000 ) ) ;
#2620 = DIRECTION ( 'NONE',  ( 0.000000000000000000, 1.000000000000000000, 0.000000000000000000 ) ) ;
#2623 = ORIENTED_EDGE ( 'NONE', *, *, #43907, .T. ) ;
#2624 = CARTESIAN_POINT ( 'NONE',  ( -165.7578939544008847, -177.1207230881787780, -43.25148278810627289 ) ) ;
#2625 = ORIENTED_EDGE ( 'NONE', *, *, #34946, .T. ) ;
#2626 = CYLINDRICAL_SURFACE ( 'NONE', #30391, 125.0000000000000000 ) ;
#2628 = CIRCLE ( 'NONE', #24452, 125.0000000000000000 ) ;
#2627 = CARTESIAN_POINT ( 'NONE',  ( -48.47912675150885065, -183.6283474603465606, 6.938893903907228378E-15 ) ) ;
#2629 = VERTEX_POINT ( 'NONE', #26977 ) ;
#2630 = CARTESIAN_POINT ( 'NONE',  ( -48.82732838694323618, -193.5000000000000000, -0.9374196611341184537 ) ) ;
#2631 = CARTESIAN_POINT ( 'NONE',  ( -48.47912675150885065, -175.3837268820161057, 6.938893903907228378E-15 ) ) ;
#2632 = CARTESIAN_POINT ( 'NONE',  ( -173.2765435274470178, -177.1207230881787780, -7.113702696401505321 ) ) ;
#2633 = LINE ( 'NONE', #10265, #5839 ) ;
#2634 = DIRECTION ( 'NONE',  ( 0.9995608365087940150, 0.000000000000000000, 0.02963332782257007206 ) ) ;
#2635 = VERTEX_POINT ( 'NONE', #26455 ) ;
#2636 = ADVANCED_FACE ( 'NONE', ( #42492 ), #26724, .T. ) ;
#2637 = FACE_OUTER_BOUND ( 'NONE', #47312, .T. ) ;
#2638 = DIRECTION ( 'NONE',  ( 0.000000000000000000, 1.000000000000000000, -0.000000000000000000 ) ) ;
#2639 = CARTESIAN_POINT ( 'NONE',  ( -336.3521761649654422, -178.6135371030394481, 23.71704087764532431 ) ) ;
#2640 = EDGE_LOOP ( 'NONE', ( #1975, #28396, #14696, #2611 ) ) ;
#2641 = FACE_OUTER_BOUND ( 'NONE', #17449, .T. ) ;
#2642 = CARTESIAN_POINT ( 'NONE',  ( -142.6204786402482512, -193.5000000000000000, -80.70646587903381430 ) ) ;
#2643 = AXIS2_PLACEMENT_3D ( 'NONE', #9378, #17008, #13042 ) ;
#2644 = FACE_OUTER_BOUND ( 'NONE', #5378, .T. ) ;
#2645 = DIRECTION ( 'NONE',  ( -0.000000000000000000, 1.000000000000000000, -0.000000000000000000 ) ) ;
#2646 = VERTEX_POINT ( 'NONE', #50648 ) ;
#2647 = AXIS2_PLACEMENT_3D ( 'NONE', #50867, #22499, #38513 ) ;
#2648 = VECTOR ( 'NONE', #51030, 1000.000000000000114 ) ;
#2649 = DIRECTION ( 'NONE',  ( 0.000000000000000000, 0.000000000000000000, 1.000000000000000000 ) ) ;
#2650 = EDGE_CURVE ( 'NONE', #23558, #3648, #13912, .T. ) ;
#2651 = DIRECTION ( 'NONE',  ( 0.000000000000000000, -0.000000000000000000, -1.000000000000000000 ) ) ;
#2652 = PLANE ( 'NONE',  #17006 ) ;
#2653 = VERTEX_POINT ( 'NONE', #50394 ) ;
#2654 = DIRECTION ( 'NONE',  ( -0.9473263538541946138, 0.000000000000000000, 0.3202698538628279690 ) ) ;
#2655 = VECTOR ( 'NONE', #16564, 1000.000000000000000 ) ;
#2656 = EDGE_CURVE ( 'NONE', #14204, #8140, #22541, .T. ) ;
#2657 = DIRECTION ( 'NONE',  ( 0.000000000000000000, 1.000000000000000000, -3.491481338843133355E-15 ) ) ;
#2658 = ORIENTED_EDGE ( 'NONE', *, *, #8920, .T. ) ;
#2659 = VERTEX_POINT ( 'NONE', #47233 ) ;
#2660 = AXIS2_PLACEMENT_3D ( 'NONE', #15162, #50910, #22781 ) ;
#2661 = EDGE_LOOP ( 'NONE', ( #31636, #28193, #50067, #25252 ) ) ;
#2662 = CARTESIAN_POINT ( 'NONE',  ( -330.4913330509368166, -131.1080185721124849, 58.50955523165764305 ) ) ;
#2663 = EDGE_CURVE ( 'NONE', #45569, #15488, #18072, .T. ) ;
#2664 = PLANE ( 'NONE',  #31209 ) ;
#2665 = DIRECTION ( 'NONE',  ( -0.7948544414133523750, 0.000000000000000000, -0.6068001458185945385 ) ) ;
#2666 = ORIENTED_EDGE ( 'NONE', *, *, #21957, .F. ) ;
#2667 = CARTESIAN_POINT ( 'NONE',  ( -48.47912675150885065, -177.1207230881787780, 6.938893903907228378E-15 ) ) ;
#2668 = DIRECTION ( 'NONE',  ( 0.000000000000000000, 0.000000000000000000, 1.000000000000000000 ) ) ;
#2671 = ORIENTED_EDGE ( 'NONE', *, *, #13934, .T. ) ;
#2670 = DIRECTION ( 'NONE',  ( 1.000000000000000000, 0.000000000000000000, -0.000000000000000000 ) ) ;
#2669 = CARTESIAN_POINT ( 'NONE',  ( -109.9568094315246327, -193.5000000000000000, -108.8370090194290611 ) ) ;
#2672 = LINE ( 'NONE', #10058, #24754 ) ;
#2673 = ORIENTED_EDGE ( 'NONE', *, *, #29493, .F. ) ;
#2674 = DIRECTION ( 'NONE',  ( 0.9995608365087944591, 0.000000000000000000, -0.02963332782255633305 ) ) ;
#2675 = VECTOR ( 'NONE', #3987, 1000.000000000000000 ) ;
#2676 = VERTEX_POINT ( 'NONE', #27498 ) ;
#2677 = CARTESIAN_POINT ( 'NONE',  ( -48.47912675150885065, -177.1207230881787780, 6.938893903907228378E-15 ) ) ;
#2678 = CARTESIAN_POINT ( 'NONE',  ( -46.00000000000000711, 0.000000000000000000, 51.00000000000000000 ) ) ;
#2679 = CIRCLE ( 'NONE', #162, 125.0000000000000000 ) ;
#2680 = FACE_OUTER_BOUND ( 'NONE', #16960, .T. ) ;
#2681 = ORIENTED_EDGE ( 'NONE', *, *, #31985, .T. ) ;
#2682 = VECTOR ( 'NONE', #38905, 1000.000000000000000 ) ;
#2683 = EDGE_CURVE ( 'NONE', #25185, #3968, #40708, .T. ) ;
#2684 = ORIENTED_EDGE ( 'NONE', *, *, #21170, .F. ) ;
#2685 = CARTESIAN_POINT ( 'NONE',  ( -305.0000000000000568, -123.5000000000000284, 15.24495751795539000 ) ) ;
#2686 = DIRECTION ( 'NONE',  ( 0.1768902751225733261, 0.000000000000000000, -0.9842305779475966077 ) ) ;
#2687 = ORIENTED_EDGE ( 'NONE', *, *, #25384, .F. ) ;
#2688 = DIRECTION ( 'NONE',  ( -0.000000000000000000, -0.3546048870425363986, -0.9350162426854146114 ) ) ;
#2689 = DIRECTION ( 'NONE',  ( 0.000000000000000000, 0.3546048870425300148, -0.9350162426854169428 ) ) ;
#2690 = VERTEX_POINT ( 'NONE', #38557 ) ;
#2691 = ADVANCED_FACE ( 'NONE', ( #46448 ), #14644, .F. ) ;
#2692 = FACE_BOUND ( 'NONE', #13303, .T. ) ;
#2693 = VECTOR ( 'NONE', #29787, 1000.000000000000000 ) ;
#2694 = CARTESIAN_POINT ( 'NONE',  ( 56.46549106873199975, -193.5000000000000000, -66.05018866041275771 ) ) ;
#2695 = ORIENTED_EDGE ( 'NONE', *, *, #19894, .T. ) ;
#2696 = DIRECTION ( 'NONE',  ( -0.7765238627180482966, 0.000000000000000000, 0.6300878435817038881 ) ) ;
#2697 = ORIENTED_EDGE ( 'NONE', *, *, #48030, .T. ) ;
#2698 = VECTOR ( 'NONE', #20468, 1000.000000000000227 ) ;
#2699 = EDGE_CURVE ( 'NONE', #32359, #21474, #10428, .T. ) ;
#2700 = VECTOR ( 'NONE', #15612, 999.9999999999998863 ) ;
#2701 = FACE_OUTER_BOUND ( 'NONE', #12692, .T. ) ;
#2702 = CARTESIAN_POINT ( 'NONE',  ( -332.3517673607765914, -104.1045282520827300, -55.74477592174792306 ) ) ;
#2703 = ORIENTED_EDGE ( 'NONE', *, *, #43271, .F. ) ;
#2704 = CARTESIAN_POINT ( 'NONE',  ( 72.31641062551800303, -175.3837268820161057, 32.14713283941990341 ) ) ;
#2705 = EDGE_CURVE ( 'NONE', #38799, #6533, #30656, .T. ) ;
#2706 = DIRECTION ( 'NONE',  ( -0.000000000000000000, -0.9709418174260502354, 0.2393156642875652051 ) ) ;
#2707 = FACE_OUTER_BOUND ( 'NONE', #37893, .T. ) ;
#2708 = VERTEX_POINT ( 'NONE', #11205 ) ;
#2709 = DIRECTION ( 'NONE',  ( 0.000000000000000000, 0.000000000000000000, 1.000000000000000000 ) ) ;
#2710 = DIRECTION ( 'NONE',  ( -0.000000000000000000, 1.000000000000000000, -0.000000000000000000 ) ) ;
#2711 = ADVANCED_FACE ( 'NONE', ( #6766 ), #50917, .F. ) ;
#2712 = DIRECTION ( 'NONE',  ( -0.000000000000000000, -1.000000000000000000, 0.000000000000000000 ) ) ;
#2714 = ORIENTED_EDGE ( 'NONE', *, *, #182, .F. ) ;
#2713 = CARTESIAN_POINT ( 'NONE',  ( -47.51449116960048968, -175.3837268820161057, -0.2635871660690578544 ) ) ;
#2715 = AXIS2_PLACEMENT_3D ( 'NONE', #26473, #6527, #22557 ) ;
#2716 = ORIENTED_EDGE ( 'NONE', *, *, #33376, .T. ) ;
#2717 = CARTESIAN_POINT ( 'NONE',  ( -330.4913330509368166, -130.1153096980145563, 58.63009191191294178 ) ) ;
#2718 = VECTOR ( 'NONE', #45275, 1000.000000000000114 ) ;
#2719 = LINE ( 'NONE', #15092, #1940 ) ;
#2720 = ORIENTED_EDGE ( 'NONE', *, *, #17747, .T. ) ;
#2721 = DIRECTION ( 'NONE',  ( -0.000000000000000000, 1.000000000000000000, -0.000000000000000000 ) ) ;
#2722 = ORIENTED_EDGE ( 'NONE', *, *, #49646, .F. ) ;
#2723 = DIRECTION ( 'NONE',  ( 0.000000000000000000, 0.000000000000000000, -1.000000000000000000 ) ) ;
#2724 = DIRECTION ( 'NONE',  ( -0.000000000000000000, 1.000000000000000000, -0.000000000000000000 ) ) ;
#2725 = CARTESIAN_POINT ( 'NONE',  ( -12.42681898335384894, -175.3837268820161057, 118.6432945265039365 ) ) ;
#2726 = FACE_OUTER_BOUND ( 'NONE', #33811, .T. ) ;
#2727 = ORIENTED_EDGE ( 'NONE', *, *, #17980, .F. ) ;
#2728 = AXIS2_PLACEMENT_3D ( 'NONE', #8668, #20762, #36793 ) ;
#2729 = ORIENTED_EDGE ( 'NONE', *, *, #49819, .F. ) ;
#2730 = CIRCLE ( 'NONE', #21197, 60.00000000000000000 ) ;
#2731 = EDGE_LOOP ( 'NONE', ( #36758, #38492, #14858, #19836 ) ) ;
#2732 = PLANE ( 'NONE',  #45962 ) ;
#2733 = DIRECTION ( 'NONE',  ( 0.5586467658036476935, 0.000000000000000000, 0.8294056854502049880 ) ) ;
#2734 = VECTOR ( 'NONE', #46732, 999.9999999999998863 ) ;
#2735 = VECTOR ( 'NONE', #3422, 1000.000000000000000 ) ;
#2736 = LINE ( 'NONE', #3508, #15313 ) ;
#2737 = LINE ( 'NONE', #18274, #6269 ) ;
#2738 = ORIENTED_EDGE ( 'NONE', *, *, #39768, .T. ) ;
#2739 = EDGE_CURVE ( 'NONE', #38573, #25631, #20615, .T. ) ;
#2740 = UNCERTAINTY_MEASURE_WITH_UNIT (LENGTH_MEASURE( 1.000000000000000082E-05 ), #29982, 'distance_accuracy_value', 'NONE');
#2741 = EDGE_CURVE ( 'NONE', #44939, #32649, #46975, .T. ) ;
#2742 = DIRECTION ( 'NONE',  ( -0.000000000000000000, 1.000000000000000000, -0.000000000000000000 ) ) ;
#2743 = CARTESIAN_POINT ( 'NONE',  ( -336.3521761649653854, -75.06648993880729392, -35.41461708323759439 ) ) ;
#2744 = ORIENTED_EDGE ( 'NONE', *, *, #51706, .T. ) ;
#2745 = ORIENTED_EDGE ( 'NONE', *, *, #39538, .T. ) ;
#2746 = DIRECTION ( 'NONE',  ( 0.000000000000000000, -0.2393156642875449158, 0.9709418174260553425 ) ) ;
#2747 = CARTESIAN_POINT ( 'NONE',  ( -339.1964088526558498, -71.49045607248255862, -27.86139516340906397 ) ) ;
#2748 = PLANE ( 'NONE',  #38418 ) ;
#2749 = DIRECTION ( 'NONE',  ( 1.000000000000000000, 0.000000000000000000, -0.000000000000000000 ) ) ;
#2750 = AXIS2_PLACEMENT_3D ( 'NONE', #2259, #50351, #46404 ) ;
#2751 = CARTESIAN_POINT ( 'NONE',  ( -149.9407190013152160, -175.3837268820161057, -73.01058346660458653 ) ) ;
#2752 = CARTESIAN_POINT ( 'NONE',  ( -72.96029774493612763, -183.6283474603465606, 122.5792489240759551 ) ) ;
#2753 = ORIENTED_EDGE ( 'NONE', *, *, #51082, .T. ) ;
#2754 = EDGE_CURVE ( 'NONE', #11828, #31627, #7016, .T. ) ;
#2755 = DIRECTION ( 'NONE',  ( 0.1476465640024851034, 0.000000000000000000, -0.9890401873221634776 ) ) ;
#2756 = EDGE_CURVE ( 'NONE', #23765, #23329, #39055, .T. ) ;
#2757 = VECTOR ( 'NONE', #51275, 1000.000000000000114 ) ;
#2758 = VERTEX_POINT ( 'NONE', #39328 ) ;
#2759 = DIRECTION ( 'NONE',  ( -0.000000000000000000, 1.000000000000000000, -0.000000000000000000 ) ) ;
#2760 = EDGE_CURVE ( 'NONE', #39742, #26732, #3330, .T. ) ;
#2761 = DIRECTION ( 'NONE',  ( 0.000000000000000000, 1.000000000000000000, -3.491481338843133355E-15 ) ) ;
#2762 = EDGE_LOOP ( 'NONE', ( #32489, #11370, #14078, #37120 ) ) ;
#2763 = FACE_OUTER_BOUND ( 'NONE', #10866, .T. ) ;
#2764 = FACE_OUTER_BOUND ( 'NONE', #6925, .T. ) ;
#2765 = DIRECTION ( 'NONE',  ( 0.000000000000000000, 0.000000000000000000, 1.000000000000000000 ) ) ;
#2766 = VECTOR ( 'NONE', #31801, 1000.000000000000000 ) ;
#2767 = CARTESIAN_POINT ( 'NONE',  ( -336.3521761649654422, -132.2320517616439020, -58.37307289257706344 ) ) ;
#2768 = AXIS2_PLACEMENT_3D ( 'NONE', #11508, #44083, #43820 ) ;
#2769 = DIRECTION ( 'NONE',  ( 0.000000000000000000, 0.000000000000000000, 1.000000000000000000 ) ) ;
#2770 = ORIENTED_EDGE ( 'NONE', *, *, #43974, .T. ) ;
#2771 = VECTOR ( 'NONE', #46047, 1000.000000000000000 ) ;
#2772 = CARTESIAN_POINT ( 'NONE',  ( -48.30223647638628393, -177.1207230881787780, 0.9842305779476049343 ) ) ;
#2774 = ORIENTED_EDGE ( 'NONE', *, *, #45659, .F. ) ;
#2773 = LINE ( 'NONE', #19839, #47981 ) ;
#2775 = ORIENTED_EDGE ( 'NONE', *, *, #16233, .F. ) ;
#2776 = LINE ( 'NONE', #39301, #47285 ) ;
#2777 = CIRCLE ( 'NONE', #49803, 125.0000000000000000 ) ;
#2778 = ORIENTED_EDGE ( 'NONE', *, *, #22631, .F. ) ;
#2779 = CARTESIAN_POINT ( 'NONE',  ( -332.3517673607765914, -181.4155151828941825, -11.56382487286496463 ) ) ;
#2780 = EDGE_LOOP ( 'NONE', ( #20754, #6754, #3639, #10849 ) ) ;
#2781 = FACE_BOUND ( 'NONE', #44782, .T. ) ;
#2782 = FACE_OUTER_BOUND ( 'NONE', #43636, .T. ) ;
#2783 = ORIENTED_EDGE ( 'NONE', *, *, #39292, .F. ) ;
#2784 = CARTESIAN_POINT ( 'NONE',  ( -305.0000000000000568, -138.3439121830091665, 58.13482838284733845 ) ) ;
#2785 = VECTOR ( 'NONE', #43097, 999.9999999999998863 ) ;
#2786 = DIRECTION ( 'NONE',  ( 0.000000000000000000, 0.000000000000000000, 1.000000000000000000 ) ) ;
#2787 = LINE ( 'NONE', #42474, #39957 ) ;
#2788 = ORIENTED_EDGE ( 'NONE', *, *, #21136, .T. ) ;
#2789 = ORIENTED_EDGE ( 'NONE', *, *, #28552, .T. ) ;
#2790 = CIRCLE ( 'NONE', #9518, 125.0000000000000000 ) ;
#2791 = ORIENTED_EDGE ( 'NONE', *, *, #22489, .F. ) ;
#2792 = DIRECTION ( 'NONE',  ( 1.000000000000000000, 0.000000000000000000, -0.000000000000000000 ) ) ;
#2793 = CARTESIAN_POINT ( 'NONE',  ( -330.4913330509368166, -71.02573290043841325, 26.97593913775512320 ) ) ;
#2794 = CARTESIAN_POINT ( 'NONE',  ( -30.31202594373736403, -183.6283474603465606, -123.6727797384705951 ) ) ;
#2795 = DIRECTION ( 'NONE',  ( 0.000000000000000000, -0.000000000000000000, 1.000000000000000000 ) ) ;
#2796 = CARTESIAN_POINT ( 'NONE',  ( -53.47502265695599277, -183.6283474603465606, -123.9001241957025883 ) ) ;
#2797 = ORIENTED_EDGE ( 'NONE', *, *, #15728, .F. ) ;
#2798 = EDGE_CURVE ( 'NONE', #22576, #12684, #35686, .T. ) ;
#2799 = EDGE_CURVE ( 'NONE', #6394, #32153, #22260, .T. ) ;
#2800 = EDGE_CURVE ( 'NONE', #875, #23517, #12747, .T. ) ;
#2801 = VECTOR ( 'NONE', #39200, 1000.000000000000000 ) ;
#2802 = EDGE_CURVE ( 'NONE', #50437, #895, #27749, .T. ) ;
#2803 = CARTESIAN_POINT ( 'NONE',  ( 36.19006208304271155, -183.6283474603465606, 90.59430563621340582 ) ) ;
#2804 = VERTEX_POINT ( 'NONE', #31955 ) ;
#2806 = ORIENTED_EDGE ( 'NONE', *, *, #30325, .T. ) ;
#2805 = DIRECTION ( 'NONE',  ( 0.9564009842765244240, 0.000000000000000000, -0.2920567706369695538 ) ) ;
#2807 = CIRCLE ( 'NONE', #7828, 60.00000000000000000 ) ;
#2808 = ORIENTED_EDGE ( 'NONE', *, *, #15183, .F. ) ;
#2809 = ADVANCED_FACE ( 'NONE', ( #23556 ), #12237, .T. ) ;
#2810 = CARTESIAN_POINT ( 'NONE',  ( -48.82732838694325750, -175.3837268820161057, 0.9374196611341252261 ) ) ;
#2811 = ADVANCED_FACE ( 'NONE', ( #7537 ), #11726, .T. ) ;
#2812 = DIRECTION ( 'NONE',  ( -0.000000000000000000, 1.000000000000000000, 0.000000000000000000 ) ) ;
#2813 = PLANE ( 'NONE',  #4386 ) ;
#2814 = DIRECTION ( 'NONE',  ( 0.000000000000000000, -0.000000000000000000, 1.000000000000000000 ) ) ;
#2815 = EDGE_LOOP ( 'NONE', ( #38971, #23611, #27214, #47047 ) ) ;
#2816 = EDGE_CURVE ( 'NONE', #20677, #44868, #51959, .T. ) ;
#2817 = CARTESIAN_POINT ( 'NONE',  ( -332.3517673607765914, -81.78065195202965754, 43.12187378178632002 ) ) ;
#2818 = ORIENTED_EDGE ( 'NONE', *, *, #42612, .T. ) ;
#2819 = EDGE_CURVE ( 'NONE', #31354, #6533, #39569, .T. ) ;
#2820 = EDGE_LOOP ( 'NONE', ( #11563, #23286, #40592, #821 ) ) ;
#2821 = CARTESIAN_POINT ( 'NONE',  ( 69.66827051661184100, -189.7472609257535510, -40.81902153125259503 ) ) ;
#2822 = CARTESIAN_POINT ( 'NONE',  ( -118.4510020108455137, -193.5000000000000000, 103.5805805771131674 ) ) ;
#2823 = ADVANCED_FACE ( 'NONE', ( #3582 ), #36685, .F. ) ;
#2824 = CARTESIAN_POINT ( 'NONE',  ( -49.47868758801764955, -183.6283474603465606, -0.02963332782256313663 ) ) ;
#2825 = DIRECTION ( 'NONE',  ( 0.000000000000000000, 1.000000000000000000, 0.000000000000000000 ) ) ;
#2826 = ORIENTED_EDGE ( 'NONE', *, *, #19915, .F. ) ;
#2827 = DIRECTION ( 'NONE',  ( -0.05924062789370006937, 0.000000000000000000, -0.9982437317643222396 ) ) ;
#2828 = VECTOR ( 'NONE', #40963, 1000.000000000000114 ) ;
#2829 = DIRECTION ( 'NONE',  ( -0.000000000000000000, 1.000000000000000000, 0.000000000000000000 ) ) ;
#2830 = ADVANCED_FACE ( 'NONE', ( #19614 ), #28007, .F. ) ;
#2831 = DIRECTION ( 'NONE',  ( 0.000000000000000000, 0.000000000000000000, 1.000000000000000000 ) ) ;
#2832 = CARTESIAN_POINT ( 'NONE',  ( -339.1964088526558498, -123.5000000000000284, 0.000000000000000000 ) ) ;
#2833 = VERTEX_POINT ( 'NONE', #8047 ) ;
#2834 = DIRECTION ( 'NONE',  ( -0.000000000000000000, 1.000000000000000000, -0.000000000000000000 ) ) ;
#2835 = DIRECTION ( 'NONE',  ( 0.000000000000000000, 0.000000000000000000, 1.000000000000000000 ) ) ;
#2836 = VECTOR ( 'NONE', #47077, 1000.000000000000000 ) ;
#2837 = DIRECTION ( 'NONE',  ( -0.9564009842765264224, 0.000000000000000000, 0.2920567706369628924 ) ) ;
#2838 = EDGE_LOOP ( 'NONE', ( #36866, #51259, #46977, #20278 ) ) ;
#2839 = DIRECTION ( 'NONE',  ( 0.000000000000000000, 0.000000000000000000, 1.000000000000000000 ) ) ;
#2840 = LINE ( 'NONE', #50952, #5182 ) ;
#2841 = ORIENTED_EDGE ( 'NONE', *, *, #31650, .F. ) ;
#2842 = LINE ( 'NONE', #43569, #1924 ) ;
#2843 = VECTOR ( 'NONE', #42616, 1000.000000000000000 ) ;
#2844 = ORIENTED_EDGE ( 'NONE', *, *, #27890, .T. ) ;
#2845 = ADVANCED_FACE ( 'NONE', ( #24588 ), #51689, .T. ) ;
#2846 = DIRECTION ( 'NONE',  ( 0.9374196611341183427, 0.000000000000000000, 0.3482016354344059095 ) ) ;
#2847 = FACE_BOUND ( 'NONE', #3385, .T. ) ;
#2848 = DIRECTION ( 'NONE',  ( -1.000000000000000000, 0.000000000000000000, 0.000000000000000000 ) ) ;
#2849 = CARTESIAN_POINT ( 'NONE',  ( -336.3521761649654422, -141.9604555052315220, 56.09938080879057765 ) ) ;
#2850 = VERTEX_POINT ( 'NONE', #35905 ) ;
#2851 = ORIENTED_EDGE ( 'NONE', *, *, #33148, .F. ) ;
#2852 = ADVANCED_FACE ( 'NONE', ( #15948 ), #36157, .T. ) ;
#2853 = DIRECTION ( 'NONE',  ( -1.000000000000000000, 0.000000000000000000, 0.000000000000000000 ) ) ;
#2854 = ORIENTED_EDGE ( 'NONE', *, *, #33907, .F. ) ;
#2855 = CARTESIAN_POINT ( 'NONE',  ( -47.53180039765465636, -193.5000000000000000, -0.3202698538628280800 ) ) ;
#2856 = VECTOR ( 'NONE', #32400, 1000.000000000000000 ) ;
#2857 = CIRCLE ( 'NONE', #35600, 125.0000000000000000 ) ;
#2858 = EDGE_CURVE ( 'NONE', #12202, #25229, #23144, .T. ) ;
#2859 = ADVANCED_FACE ( 'NONE', ( #16198 ), #32214, .F. ) ;
#2860 = EDGE_CURVE ( 'NONE', #33085, #41706, #44322, .T. ) ;
#2861 = AXIS2_PLACEMENT_3D ( 'NONE', #30360, #6475, #34315 ) ;
#2862 = ADVANCED_FACE ( 'NONE', ( #48779 ), #8312, .T. ) ;
#2863 = CARTESIAN_POINT ( 'NONE',  ( -330.4913330509368166, -64.99044476834247064, -7.608018572113060429 ) ) ;
#2864 = CARTESIAN_POINT ( 'NONE',  ( 62.59443091842027940, -183.6283474603465606, -57.33816169485142211 ) ) ;
#2865 = ORIENTED_EDGE ( 'NONE', *, *, #40463, .T. ) ;
#2868 = VERTEX_POINT ( 'NONE', #684 ) ;
#2867 = FILL_AREA_STYLE ('',( #38863 ) ) ;
#2866 = CARTESIAN_POINT ( 'NONE',  ( -47.97059563285963435, -183.6283474603465606, 0.8610436117673654355 ) ) ;
#2869 = CARTESIAN_POINT ( 'NONE',  ( 9.518239912201957864, -213.5000000000000000, -110.7307791902283043 ) ) ;
#2870 = VERTEX_POINT ( 'NONE', #12507 ) ;
#2871 = DIRECTION ( 'NONE',  ( -0.4566292373937018145, 0.000000000000000000, -0.8896570909947529859 ) ) ;
#2872 = ORIENTED_EDGE ( 'NONE', *, *, #6919, .F. ) ;
#2873 = DIRECTION ( 'NONE',  ( 0.000000000000000000, 0.000000000000000000, 1.000000000000000000 ) ) ;
#2874 = ORIENTED_EDGE ( 'NONE', *, *, #6026, .T. ) ;
#2875 = EDGE_CURVE ( 'NONE', #25045, #32314, #22264, .T. ) ;
#2878 = ORIENTED_EDGE ( 'NONE', *, *, #23932, .T. ) ;
#2877 = FACE_OUTER_BOUND ( 'NONE', #9899, .T. ) ;
#2876 = CARTESIAN_POINT ( 'NONE',  ( -339.1964088526558498, -79.66942718702493664, 39.49849221029193558 ) ) ;
#2879 = AXIS2_PLACEMENT_3D ( 'NONE', #4892, #20919, #8809 ) ;
#2880 = ORIENTED_EDGE ( 'NONE', *, *, #42682, .T. ) ;
#2881 = LINE ( 'NONE', #18913, #13957 ) ;
#2882 = EDGE_LOOP ( 'NONE', ( #45557, #45621, #1268, #44318 ) ) ;
#2883 = CARTESIAN_POINT ( 'NONE',  ( -47.78257572244585560, -193.5000000000000000, -0.7175072570443230546 ) ) ;
#2884 = PLANE ( 'NONE',  #25669 ) ;
#2885 = ADVANCED_FACE ( 'NONE', ( #5413 ), #49565, .F. ) ;
#2886 = EDGE_LOOP ( 'NONE', ( #13, #47836, #40281, #29504 ) ) ;
#2887 = CYLINDRICAL_SURFACE ( 'NONE', #23860, 125.0000000000000000 ) ;
#2888 = PLANE ( 'NONE',  #9864 ) ;
#2889 = CARTESIAN_POINT ( 'NONE',  ( -165.6791976657750354, -193.5000000000000000, 40.49875167739066484 ) ) ;
#2890 = SHAPE_REPRESENTATION ( 'Angle Mounting Base', ( #31742 ), #46023 ) ;
#2891 = PLANE ( 'NONE',  #28210 ) ;
#2892 = EDGE_CURVE ( 'NONE', #30709, #13937, #25888, .T. ) ;
#2893 = EDGE_LOOP ( 'NONE', ( #13406, #34994, #35244, #25037 ) ) ;
#2894 = LINE ( 'NONE', #10269, #38868 ) ;
#2895 = DIRECTION ( 'NONE',  ( -0.000000000000000000, 1.000000000000000000, -0.000000000000000000 ) ) ;
#2896 = EDGE_CURVE ( 'NONE', #39380, #11174, #39873, .T. ) ;
#2897 = CARTESIAN_POINT ( 'NONE',  ( 71.44208735029287993, -183.6283474603465606, 35.26900067126700833 ) ) ;
#2898 = VERTEX_POINT ( 'NONE', #21425 ) ;
#2899 = DIRECTION ( 'NONE',  ( -0.000000000000000000, 1.047444401652940007E-14, 1.000000000000000000 ) ) ;
#2900 = DIRECTION ( 'NONE',  ( 0.000000000000000000, 0.000000000000000000, 1.000000000000000000 ) ) ;
#2901 = AXIS2_PLACEMENT_3D ( 'NONE', #3705, #31833, #19474 ) ;
#2902 = CARTESIAN_POINT ( 'NONE',  ( -339.1964088526558498, -95.63860483659040312, 52.00954392751717847 ) ) ;
#2903 = AXIS2_PLACEMENT_3D ( 'NONE', #29131, #37549, #37280 ) ;
#2904 = PLANE ( 'NONE',  #6793 ) ;
#2905 = FACE_OUTER_BOUND ( 'NONE', #6954, .T. ) ;
#2906 = EDGE_LOOP ( 'NONE', ( #26695, #12208, #32985, #5534, #29970 ) ) ;
#2907 = VECTOR ( 'NONE', #5897, 1000.000000000000000 ) ;
#2908 = ADVANCED_FACE ( 'NONE', ( #9350 ), #25376, .T. ) ;
#2909 = DIRECTION ( 'NONE',  ( 0.1182731709213523247, 0.000000000000000000, 0.9929810960135185827 ) ) ;
#2910 = DIRECTION ( 'NONE',  ( -0.000000000000000000, -1.000000000000000000, 0.000000000000000000 ) ) ;
#2911 = CARTESIAN_POINT ( 'NONE',  ( -339.1964088526558498, -103.0458197858333165, -55.34326076196084188 ) ) ;
#2912 = CARTESIAN_POINT ( 'NONE',  ( -164.2512865680372727, -193.5000000000000000, -47.13604789772046644 ) ) ;
#2913 = CARTESIAN_POINT ( 'NONE',  ( -170.9669310976187830, -193.5000000000000000, -24.93467037017130394 ) ) ;
#2914 = ORIENTED_EDGE ( 'NONE', *, *, #26626, .F. ) ;
#2915 = AXIS2_PLACEMENT_3D ( 'NONE', #4289, #20311, #40535 ) ;
#2916 = CARTESIAN_POINT ( 'NONE',  ( 4.017037286467739499, 55.83657353238506005, -17.50344790800143358 ) ) ;
#2917 = CYLINDRICAL_SURFACE ( 'NONE', #1135, 125.0000000000000000 ) ;
#2918 = ORIENTED_EDGE ( 'NONE', *, *, #27844, .F. ) ;
#2919 = ORIENTED_EDGE ( 'NONE', *, *, #23417, .F. ) ;
#2920 = EDGE_LOOP ( 'NONE', ( #46963, #47101, #2188, #41222 ) ) ;
#2921 = DIRECTION ( 'NONE',  ( 1.000000000000000000, 0.000000000000000000, 0.000000000000000000 ) ) ;
#2922 = EDGE_CURVE ( 'NONE', #24837, #50461, #41647, .T. ) ;
#2923 = EDGE_CURVE ( 'NONE', #25127, #43983, #33772, .T. ) ;
#2924 = DIRECTION ( 'NONE',  ( 0.05924062789370748011, 0.000000000000000000, 0.9982437317643217956 ) ) ;
#2925 = VERTEX_POINT ( 'NONE', #37971 ) ;
#2926 = DIRECTION ( 'NONE',  ( -0.000000000000000000, 1.000000000000000000, -0.000000000000000000 ) ) ;
#2927 = DIRECTION ( 'NONE',  ( -0.000000000000000000, 0.9709418174260492362, -0.2393156642875685636 ) ) ;
#2930 = ORIENTED_EDGE ( 'NONE', *, *, #39774, .F. ) ;
#2929 = CARTESIAN_POINT ( 'NONE',  ( -164.6073096293132494, -177.1207230881787780, 43.47841891815208726 ) ) ;
#2928 = LINE ( 'NONE', #18966, #28309 ) ;
#2931 = LINE ( 'NONE', #23933, #8839 ) ;
#2932 = AXIS2_PLACEMENT_3D ( 'NONE', #1000, #49620, #17055 ) ;
#2933 = VERTEX_POINT ( 'NONE', #36944 ) ;
#2934 = LINE ( 'NONE', #6376, #35599 ) ;
#2935 = VERTEX_POINT ( 'NONE', #50080 ) ;
#2936 = VECTOR ( 'NONE', #7553, 1000.000000000000000 ) ;
#2937 = CARTESIAN_POINT ( 'NONE',  ( -37.67038537088847505, -183.6283474603465606, -124.5318076226586470 ) ) ;
#2938 = FACE_OUTER_BOUND ( 'NONE', #31043, .T. ) ;
#2939 = DIRECTION ( 'NONE',  ( 0.000000000000000000, -1.000000000000000000, -0.000000000000000000 ) ) ;
#2940 = VECTOR ( 'NONE', #26490, 999.9999999999998863 ) ;
#2941 = EDGE_LOOP ( 'NONE', ( #10313, #30842, #37717, #37536 ) ) ;
#2942 = ORIENTED_EDGE ( 'NONE', *, *, #20563, .F. ) ;
#2943 = DIRECTION ( 'NONE',  ( -0.000000000000000000, 1.000000000000000000, -0.000000000000000000 ) ) ;
#2944 = DIRECTION ( 'NONE',  ( 0.000000000000000000, 0.000000000000000000, 1.000000000000000000 ) ) ;
#2945 = ORIENTED_EDGE ( 'NONE', *, *, #37713, .F. ) ;
#2947 = EDGE_CURVE ( 'NONE', #48835, #49515, #19779, .T. ) ;
#2946 = AXIS2_PLACEMENT_3D ( 'NONE', #746, #12029, #48846 ) ;
#2948 = CARTESIAN_POINT ( 'NONE',  ( -29.85296035031868911, -177.1207230881787780, 122.5936119678275844 ) ) ;
#2949 = CIRCLE ( 'NONE', #2123, 25.00456841203572722 ) ;
#2950 = CARTESIAN_POINT ( 'NONE',  ( -4.794493649713349015, -193.5000000000000000, -117.1181148702518726 ) ) ;
#2951 = ORIENTED_EDGE ( 'NONE', *, *, #48129, .T. ) ;
#2952 = FACE_BOUND ( 'NONE', #22178, .T. ) ;
#2953 = AXIS2_PLACEMENT_3D ( 'NONE', #41258, #5284, #5543 ) ;
#2954 = LINE ( 'NONE', #18734, #18101 ) ;
#2955 = EDGE_CURVE ( 'NONE', #44801, #16051, #10562, .T. ) ;
#2956 = VECTOR ( 'NONE', #9154, 1000.000000000000000 ) ;
#2957 = ORIENTED_EDGE ( 'NONE', *, *, #8334, .F. ) ;
#2958 = LINE ( 'NONE', #18994, #12322 ) ;
#2959 = VERTEX_POINT ( 'NONE', #1183 ) ;
#2960 = PLANE ( 'NONE',  #14770 ) ;
#2961 = CARTESIAN_POINT ( 'NONE',  ( -170.6250538923603131, -189.7472609257535510, 26.55884942729649723 ) ) ;
#2962 = ORIENTED_EDGE ( 'NONE', *, *, #49101, .T. ) ;
#2963 = CARTESIAN_POINT ( 'NONE',  ( -49.47868758801764955, -177.1207230881787780, -0.02963332782256313663 ) ) ;
#2964 = PLANE ( 'NONE',  #28054 ) ;
#2965 = CARTESIAN_POINT ( 'NONE',  ( -103.4012653778457462, -183.6283474603465606, -112.2878385610366649 ) ) ;
#2966 = ORIENTED_EDGE ( 'NONE', *, *, #30159, .T. ) ;
#2967 = CARTESIAN_POINT ( 'NONE',  ( -109.5001801941309196, -183.6283474603465606, -107.9473519284343297 ) ) ;
#2968 = VECTOR ( 'NONE', #11030, 1000.000000000000000 ) ;
#2969 = DIRECTION ( 'NONE',  ( 0.000000000000000000, -1.000000000000000000, 0.000000000000000000 ) ) ;
#2970 = CARTESIAN_POINT ( 'NONE',  ( 43.57032560458359427, -193.5000000000000000, 83.08371579725746869 ) ) ;
#2972 = VERTEX_POINT ( 'NONE', #1974 ) ;
#2971 = DIRECTION ( 'NONE',  ( 0.000000000000000000, 0.2393156642875652051, 0.9709418174260502354 ) ) ;
#2973 = VECTOR ( 'NONE', #14794, 1000.000000000000000 ) ;
#2974 = AXIS2_PLACEMENT_3D ( 'NONE', #47893, #24748, #16346 ) ;
#2975 = ORIENTED_EDGE ( 'NONE', *, *, #31753, .F. ) ;
#2976 = DIRECTION ( 'NONE',  ( 0.000000000000000000, 0.000000000000000000, 1.000000000000000000 ) ) ;
#2977 = PLANE ( 'NONE',  #48113 ) ;
#2978 = ORIENTED_EDGE ( 'NONE', *, *, #37892, .F. ) ;
#2979 = ORIENTED_EDGE ( 'NONE', *, *, #51076, .F. ) ;
#2980 = DIRECTION ( 'NONE',  ( -0.9374196611341206742, 0.000000000000000000, -0.3482016354343996367 ) ) ;
#2981 = VECTOR ( 'NONE', #18582, 1000.000000000000114 ) ;
#2982 = EDGE_LOOP ( 'NONE', ( #34516, #40352, #15843, #39033 ) ) ;
#2983 = CARTESIAN_POINT ( 'NONE',  ( -332.3517673607765914, -64.50000000000000000, -2.632288850093980503 ) ) ;
#2984 = DIRECTION ( 'NONE',  ( 0.000000000000000000, 0.000000000000000000, -1.000000000000000000 ) ) ;
#2985 = VECTOR ( 'NONE', #49150, 1000.000000000000000 ) ;
#2986 = EDGE_CURVE ( 'NONE', #10698, #24816, #16980, .T. ) ;
#2988 = VECTOR ( 'NONE', #2170, 1000.000000000000000 ) ;
#2987 = DIRECTION ( 'NONE',  ( -0.4566292373937200777, 0.000000000000000000, 0.8896570909947436601 ) ) ;
#2989 = LINE ( 'NONE', #43463, #43400 ) ;
#2990 = ORIENTED_EDGE ( 'NONE', *, *, #34656, .F. ) ;
#2991 = ORIENTED_EDGE ( 'NONE', *, *, #23932, .F. ) ;
#2992 = ORIENTED_EDGE ( 'NONE', *, *, #24458, .F. ) ;
#2993 = CIRCLE ( 'NONE', #32357, 125.0000000000000000 ) ;
#2994 = CARTESIAN_POINT ( 'NONE',  ( 15.23368049493604381, -175.3837268820161057, -107.5438431188757420 ) ) ;
#2995 = CARTESIAN_POINT ( 'NONE',  ( -339.1964088526558498, -156.6043281241909426, 48.84008046109164525 ) ) ;
#2996 = DIRECTION ( 'NONE',  ( -0.9151456172430181280, 0.000000000000000000, -0.4031234292879730674 ) ) ;
#2997 = CARTESIAN_POINT ( 'NONE',  ( -170.0000000000000284, -123.5000000000000284, -41.63467731922663972 ) ) ;
#2998 = CARTESIAN_POINT ( 'NONE',  ( -96.65280530915691770, -177.1207230881787780, -115.3442529744087324 ) ) ;
#2999 = ORIENTED_EDGE ( 'NONE', *, *, #10007, .F. ) ;
#3000 = ADVANCED_FACE ( 'NONE', ( #37720 ), #5154, .F. ) ;
#3001 = CARTESIAN_POINT ( 'NONE',  ( -339.1964088526558498, -79.00630452878414189, 38.74998146212082162 ) ) ;
#3002 = ORIENTED_EDGE ( 'NONE', *, *, #25192, .T. ) ;
#3003 = ORIENTED_EDGE ( 'NONE', *, *, #37644, .F. ) ;
#3004 = AXIS2_PLACEMENT_3D ( 'NONE', #32821, #20744, #45447 ) ;
#3005 = CARTESIAN_POINT ( 'NONE',  ( 66.42899531795131907, -177.1207230881787780, 49.20491319441622124 ) ) ;
#3006 = DIRECTION ( 'NONE',  ( -0.1182731709213523247, 0.000000000000000000, -0.9929810960135185827 ) ) ;
#3007 = ADVANCED_FACE ( 'NONE', ( #13808 ), #18015, .F. ) ;
#3008 = DIRECTION ( 'NONE',  ( -0.000000000000000000, 0.4647231720437664526, -0.8854560256532110207 ) ) ;
#3009 = VECTOR ( 'NONE', #26277, 1000.000000000000114 ) ;
#3010 = VECTOR ( 'NONE', #24179, 1000.000000000000000 ) ;
#3011 = ADVANCED_FACE ( 'NONE', ( #21172 ), #41397, .T. ) ;
#3012 = CARTESIAN_POINT ( 'NONE',  ( -70.75782287548091176, -193.5000000000000000, 122.9986166548864901 ) ) ;
#3013 = CARTESIAN_POINT ( 'NONE',  ( -139.4082623311987277, -175.3837268820161057, 84.30834960113001841 ) ) ;
#3014 = ORIENTED_EDGE ( 'NONE', *, *, #49400, .T. ) ;
#3015 = CARTESIAN_POINT ( 'NONE',  ( -339.1964088526558498, -144.8891964568517778, 54.98865587491845730 ) ) ;
#3016 = VERTEX_POINT ( 'NONE', #5934 ) ;
#3017 = FACE_OUTER_BOUND ( 'NONE', #25613, .T. ) ;
#3018 = VECTOR ( 'NONE', #35769, 1000.000000000000000 ) ;
#3019 = PLANE ( 'NONE',  #44621 ) ;
#3020 = VERTEX_POINT ( 'NONE', #29824 ) ;
#3021 = AXIS2_PLACEMENT_3D ( 'NONE', #42183, #18796, #50100 ) ;
#3022 = CYLINDRICAL_SURFACE ( 'NONE', #14781, 125.0000000000000000 ) ;
#3023 = DIRECTION ( 'NONE',  ( 0.6965510290629882695, 0.000000000000000000, 0.7175072570443395970 ) ) ;
#3024 = DIRECTION ( 'NONE',  ( -0.5829794791144820021, 0.000000000000000000, 0.8124868780056742068 ) ) ;
#3025 = AXIS2_PLACEMENT_3D ( 'NONE', #14367, #25930, #18321 ) ;
#3026 = CARTESIAN_POINT ( 'NONE',  ( -118.1688136093591908, -193.5000000000000000, -103.7706487676296661 ) ) ;
#3028 = VECTOR ( 'NONE', #25182, 1000.000000000000227 ) ;
#3027 = LINE ( 'NONE', #42189, #16908 ) ;
#3029 = VERTEX_POINT ( 'NONE', #34032 ) ;
#3030 = DIRECTION ( 'NONE',  ( 0.000000000000000000, 1.000000000000000000, 0.000000000000000000 ) ) ;
#3032 = EDGE_LOOP ( 'NONE', ( #2625, #17208, #41097, #37453 ) ) ;
#3031 = CARTESIAN_POINT ( 'NONE',  ( -48.07600332222088468, -183.6283474603465606, 0.9151456172430280089 ) ) ;
#3033 = EDGE_CURVE ( 'NONE', #43448, #13360, #9867, .T. ) ;
#3034 = VERTEX_POINT ( 'NONE', #8812 ) ;
#3035 = DIRECTION ( 'NONE',  ( 0.000000000000000000, 0.000000000000000000, 1.000000000000000000 ) ) ;
#3036 = EDGE_LOOP ( 'NONE', ( #29313, #32102, #4306, #26916 ) ) ;
#3037 = EDGE_CURVE ( 'NONE', #14966, #49846, #4895, .T. ) ;
#3038 = PLANE ( 'NONE',  #41079 ) ;
#3039 = AXIS2_PLACEMENT_3D ( 'NONE', #40366, #33015, #32504 ) ;
#3040 = AXIS2_PLACEMENT_3D ( 'NONE', #8328, #24354, #704 ) ;
#3041 = VERTEX_POINT ( 'NONE', #7658 ) ;
#3042 = FACE_BOUND ( 'NONE', #22300, .T. ) ;
#3043 = DIRECTION ( 'NONE',  ( -0.000000000000000000, -0.4647231720437604574, 0.8854560256532141294 ) ) ;
#3044 = VERTEX_POINT ( 'NONE', #3983 ) ;
#3045 = CARTESIAN_POINT ( 'NONE',  ( -332.3517673607765914, -107.5615171630107056, 57.84431488793861575 ) ) ;
#3046 = AXIS2_PLACEMENT_3D ( 'NONE', #50143, #42223, #22005 ) ;
#3047 = EDGE_CURVE ( 'NONE', #43162, #44157, #43415, .T. ) ;
#3048 = CARTESIAN_POINT ( 'NONE',  ( -305.0000000000000568, -140.4009141470556870, -57.57047073799078873 ) ) ;
#3049 = LINE ( 'NONE', #34835, #29053 ) ;
#3050 = ORIENTED_EDGE ( 'NONE', *, *, #20215, .F. ) ;
#3051 = ORIENTED_EDGE ( 'NONE', *, *, #800, .T. ) ;
#3052 = EDGE_CURVE ( 'NONE', #24818, #177, #30697, .T. ) ;
#3053 = ORIENTED_EDGE ( 'NONE', *, *, #4211, .F. ) ;
#3054 = PLANE ( 'NONE',  #30107 ) ;
#3055 = CARTESIAN_POINT ( 'NONE',  ( -23.01747912075234836, -177.1207230881787780, -122.3793467049370776 ) ) ;
#3056 = VECTOR ( 'NONE', #23259, 1000.000000000000000 ) ;
#3057 = EDGE_CURVE ( 'NONE', #5120, #41700, #23681, .T. ) ;
#3058 = CARTESIAN_POINT ( 'NONE',  ( -156.7610986364826999, -183.6283474603465606, -62.45009659481509345 ) ) ;
#3059 = AXIS2_PLACEMENT_3D ( 'NONE', #27944, #4046, #12435 ) ;
#3061 = AXIS2_PLACEMENT_3D ( 'NONE', #18088, #17832, #5240 ) ;
#3060 = DIRECTION ( 'NONE',  ( 0.000000000000000000, -1.000000000000000000, 0.000000000000000000 ) ) ;
#3062 = CYLINDRICAL_SURFACE ( 'NONE', #20469, 125.0000000000000000 ) ;
#3063 = ORIENTED_EDGE ( 'NONE', *, *, #46846, .F. ) ;
#3064 = CIRCLE ( 'NONE', #49224, 125.0000000000000000 ) ;
#3065 = PLANE ( 'NONE',  #19855 ) ;
#3066 = ORIENTED_EDGE ( 'NONE', *, *, #38478, .F. ) ;
#3068 = VERTEX_POINT ( 'NONE', #7423 ) ;
#3067 = DIRECTION ( 'NONE',  ( 0.000000000000000000, 0.000000000000000000, 1.000000000000000000 ) ) ;
#3069 = VERTEX_POINT ( 'NONE', #47100 ) ;
#3070 = DIRECTION ( 'NONE',  ( 0.000000000000000000, -1.000000000000000000, 0.000000000000000000 ) ) ;
#3071 = AXIS2_PLACEMENT_3D ( 'NONE', #45732, #46260, #18129 ) ;
#3072 = ADVANCED_FACE ( 'NONE', ( #23444 ), #18980, .T. ) ;
#3073 = DIRECTION ( 'NONE',  ( 0.000000000000000000, -0.000000000000000000, -1.000000000000000000 ) ) ;
#3074 = DIRECTION ( 'NONE',  ( -0.1768902751225666370, 0.000000000000000000, -0.9842305779475979399 ) ) ;
#3075 = DIRECTION ( 'NONE',  ( 0.6300878435817148793, 0.000000000000000000, -0.7765238627180394149 ) ) ;
#3076 = ORIENTED_EDGE ( 'NONE', *, *, #47711, .T. ) ;
#3077 = FACE_OUTER_BOUND ( 'NONE', #12073, .T. ) ;
#3078 = VERTEX_POINT ( 'NONE', #34 ) ;
#3079 = ORIENTED_EDGE ( 'NONE', *, *, #4152, .T. ) ;
#3080 = CARTESIAN_POINT ( 'NONE',  ( 11.10560377650620012, -177.1207230881787780, -108.7464374498168951 ) ) ;
#3081 = AXIS2_PLACEMENT_3D ( 'NONE', #13770, #38898, #15013 ) ;
#3082 = CARTESIAN_POINT ( 'NONE',  ( 46.01898237923986557, -193.5000000000000000, -81.82363577055902226 ) ) ;
#3083 = VECTOR ( 'NONE', #40563, 1000.000000000000000 ) ;
#3084 = CARTESIAN_POINT ( 'NONE',  ( -339.1964088526558498, -137.1341532842523065, 57.40522506028101901 ) ) ;
#3085 = ORIENTED_EDGE ( 'NONE', *, *, #25013, .F. ) ;
#3086 = CARTESIAN_POINT ( 'NONE',  ( -332.3517673607765914, -94.63601285149479736, 51.48334306143172512 ) ) ;
#3087 = CARTESIAN_POINT ( 'NONE',  ( -129.9529520667707914, -175.3837268820161057, -94.79987230211959570 ) ) ;
#3088 = VECTOR ( 'NONE', #45524, 1000.000000000000000 ) ;
#3089 = DIRECTION ( 'NONE',  ( 0.000000000000000000, 0.2393156642875449158, -0.9709418174260553425 ) ) ;
#3090 = CARTESIAN_POINT ( 'NONE',  ( -49.47517659412406488, -177.1207230881787780, -0.08879589532293878651 ) ) ;
#3091 = ORIENTED_EDGE ( 'NONE', *, *, #39404, .T. ) ;
#3092 = CARTESIAN_POINT ( 'NONE',  ( -99.22478721462988460, -193.5000000000000000, -113.1409892739921901 ) ) ;
#3093 = PLANE ( 'NONE',  #8942 ) ;
#3094 = PLANE ( 'NONE',  #22383 ) ;
#3095 = ORIENTED_EDGE ( 'NONE', *, *, #6975, .T. ) ;
#3096 = CONICAL_SURFACE ( 'NONE', #32470, 25.00456841203573077, 0.5765357807043077765 ) ;
#3097 = AXIS2_PLACEMENT_3D ( 'NONE', #45252, #17896, #49183 ) ;
#3098 = PLANE ( 'NONE',  #40657 ) ;
#3099 = VECTOR ( 'NONE', #34479, 1000.000000000000000 ) ;
#3100 = VECTOR ( 'NONE', #26864, 1000.000000000000000 ) ;
#3101 = CARTESIAN_POINT ( 'NONE',  ( 31.28129687248616619, -183.6283474603465606, 96.24590808611479531 ) ) ;
#3102 = EDGE_CURVE ( 'NONE', #15715, #19072, #27102, .T. ) ;
#3103 = ORIENTED_EDGE ( 'NONE', *, *, #44152, .F. ) ;
#3104 = EDGE_CURVE ( 'NONE', #47705, #1934, #47877, .T. ) ;
#3105 = FACE_OUTER_BOUND ( 'NONE', #21896, .T. ) ;
#3106 = ORIENTED_EDGE ( 'NONE', *, *, #33863, .F. ) ;
#3107 = VECTOR ( 'NONE', #25503, 1000.000000000000000 ) ;
#3108 = DIRECTION ( 'NONE',  ( -0.000000000000000000, 0.4647231720437664526, -0.8854560256532110207 ) ) ;
#3109 = FACE_BOUND ( 'NONE', #5872, .T. ) ;
#3110 = DIRECTION ( 'NONE',  ( 0.000000000000000000, 1.000000000000000000, 0.000000000000000000 ) ) ;
#3111 = ADVANCED_FACE ( 'NONE', ( #35001 ), #35505, .T. ) ;
#3112 = EDGE_CURVE ( 'NONE', #41165, #35901, #7227, .T. ) ;
#3113 = PLANE ( 'NONE',  #19333 ) ;
#3114 = ORIENTED_EDGE ( 'NONE', *, *, #18878, .F. ) ;
#3115 = EDGE_CURVE ( 'NONE', #7946, #37313, #3452, .T. ) ;
#3116 = ORIENTED_EDGE ( 'NONE', *, *, #22392, .F. ) ;
#3117 = DIRECTION ( 'NONE',  ( 0.000000000000000000, 1.000000000000000000, 0.000000000000000000 ) ) ;
#3118 = AXIS2_PLACEMENT_3D ( 'NONE', #4623, #48537, #24855 ) ;
#3119 = VECTOR ( 'NONE', #28363, 1000.000000000000000 ) ;
#3120 = ADVANCED_FACE ( 'NONE', ( #15052 ), #51302, .F. ) ;
#3121 = EDGE_LOOP ( 'NONE', ( #15323, #40152, #28164, #32190 ) ) ;
#3122 = DIRECTION ( 'NONE',  ( -0.000000000000000000, -1.000000000000000000, 0.000000000000000000 ) ) ;
#3123 = AXIS2_PLACEMENT_3D ( 'NONE', #668, #4342, #27991 ) ;
#3124 = ADVANCED_FACE ( 'NONE', ( #11077 ), #43139, .T. ) ;
#3125 = CARTESIAN_POINT ( 'NONE',  ( -330.4913330509368166, -150.4759391377553186, 52.47426709956150859 ) ) ;
#3126 = CARTESIAN_POINT ( 'NONE',  ( -48.47912675150885065, -117.5479369270332057, 6.938893903907228378E-15 ) ) ;
#3127 = ORIENTED_EDGE ( 'NONE', *, *, #18949, .T. ) ;
#3130 = ORIENTED_EDGE ( 'NONE', *, *, #18472, .F. ) ;
#3129 = LINE ( 'NONE', #30715, #7153 ) ;
#3128 = CARTESIAN_POINT ( 'NONE',  ( -3.363028148951364926, 51.75966409074786867, -20.33422011939856944 ) ) ;
#3131 = VECTOR ( 'NONE', #15151, 1000.000000000000000 ) ;
#3132 = AXIS2_PLACEMENT_3D ( 'NONE', #26330, #21355, #13998 ) ;
#3133 = VECTOR ( 'NONE', #14392, 1000.000000000000000 ) ;
#3134 = CARTESIAN_POINT ( 'NONE',  ( -167.9436818089035626, -183.6283474603465606, 36.78613984830037253 ) ) ;
#3135 = ORIENTED_EDGE ( 'NONE', *, *, #15115, .F. ) ;
#3136 = CARTESIAN_POINT ( 'NONE',  ( 72.14504940832446778, -175.3837268820161057, -32.78426643622660208 ) ) ;
#3137 = ORIENTED_EDGE ( 'NONE', *, *, #21168, .T. ) ;
#3138 = AXIS2_PLACEMENT_3D ( 'NONE', #20212, #28603, #28349 ) ;
#3139 = LINE ( 'NONE', #11784, #27555 ) ;
#3140 = VERTEX_POINT ( 'NONE', #19736 ) ;
#3142 = DIRECTION ( 'NONE',  ( 0.000000000000000000, 0.000000000000000000, 1.000000000000000000 ) ) ;
#3141 = LINE ( 'NONE', #2095, #48429 ) ;
#3143 = ORIENTED_EDGE ( 'NONE', *, *, #36585, .F. ) ;
#3144 = CIRCLE ( 'NONE', #32518, 125.0000000000000000 ) ;
#3145 = LINE ( 'NONE', #43604, #15646 ) ;
#3146 = EDGE_CURVE ( 'NONE', #16791, #46777, #7146, .T. ) ;
#3147 = VERTEX_POINT ( 'NONE', #23186 ) ;
#3148 = CARTESIAN_POINT ( 'NONE',  ( -336.3521761649653854, -73.21199843436539823, 32.72792230702599170 ) ) ;
#3149 = FACE_OUTER_BOUND ( 'NONE', #40264, .T. ) ;
#3150 = EDGE_LOOP ( 'NONE', ( #32702, #7727, #10320, #4760 ) ) ;
#3151 = DIRECTION ( 'NONE',  ( -0.9842305779475992722, 0.000000000000000000, 0.1768902751225592818 ) ) ;
#3152 = CARTESIAN_POINT ( 'NONE',  ( 17.15229921100054611, -193.5000000000000000, -106.3838142112212921 ) ) ;
#3153 = DIRECTION ( 'NONE',  ( 1.000000000000000000, 0.000000000000000000, -0.000000000000000000 ) ) ;
#3154 = CARTESIAN_POINT ( 'NONE',  ( -332.3517673607765914, -107.7955183043589500, 56.89493493766750731 ) ) ;
#3155 = VERTEX_POINT ( 'NONE', #10122 ) ;
#3156 = DIRECTION ( 'NONE',  ( 1.000000000000000000, 0.000000000000000000, 0.000000000000000000 ) ) ;
#3157 = CARTESIAN_POINT ( 'NONE',  ( 72.89680503569744019, -175.3837268820161057, -25.37485791684304104 ) ) ;
#3158 = DIRECTION ( 'NONE',  ( 0.000000000000000000, -0.000000000000000000, -1.000000000000000000 ) ) ;
#3159 = EDGE_CURVE ( 'NONE', #47840, #4101, #20007, .T. ) ;
#3160 = DIRECTION ( 'NONE',  ( 0.000000000000000000, 0.000000000000000000, -1.000000000000000000 ) ) ;
#3161 = ORIENTED_EDGE ( 'NONE', *, *, #35392, .F. ) ;
#3162 = CIRCLE ( 'NONE', #36734, 125.0000000000000000 ) ;
#3163 = VECTOR ( 'NONE', #33338, 1000.000000000000114 ) ;
#3164 = CARTESIAN_POINT ( 'NONE',  ( -157.5429198988176438, -175.3837268820161057, 61.07445476073478829 ) ) ;
#3165 = CARTESIAN_POINT ( 'NONE',  ( -332.3517673607765914, -104.7054247829104270, -56.98038208374144631 ) ) ;
#3167 = CIRCLE ( 'NONE', #16614, 125.0000000000000000 ) ;
#3166 = DIRECTION ( 'NONE',  ( 0.7765238627180393038, 0.000000000000000000, 0.6300878435817147682 ) ) ;
#3168 = ADVANCED_FACE ( 'NONE', ( #51824 ), #15827, .F. ) ;
#3169 = CARTESIAN_POINT ( 'NONE',  ( -9.070200226166578616, -183.6283474603465606, -117.5715283571803980 ) ) ;
#3170 = EDGE_CURVE ( 'NONE', #41712, #41605, #3212, .T. ) ;
#3172 = EDGE_LOOP ( 'NONE', ( #6180, #10770, #244, #46153 ) ) ;
#3171 = CARTESIAN_POINT ( 'NONE',  ( -336.3521761649654422, -152.3639871485048900, -51.48334306143194539 ) ) ;
#3173 = EDGE_CURVE ( 'NONE', #28688, #50802, #8052, .T. ) ;
#3174 = EDGE_CURVE ( 'NONE', #172, #14931, #16075, .T. ) ;
#3175 = EDGE_CURVE ( 'NONE', #22773, #77, #32382, .T. ) ;
#3176 = AXIS2_PLACEMENT_3D ( 'NONE', #45599, #21409, #49549 ) ;
#3177 = CARTESIAN_POINT ( 'NONE',  ( -336.3521761649654422, -121.8677111499054320, 59.00000000000001421 ) ) ;
#3178 = EDGE_CURVE ( 'NONE', #45491, #50412, #37419, .T. ) ;
#3179 = PLANE ( 'NONE',  #51395 ) ;
#3180 = DIRECTION ( 'NONE',  ( 0.000000000000000000, 1.000000000000000000, 0.000000000000000000 ) ) ;
#3181 = DIRECTION ( 'NONE',  ( 0.000000000000000000, 0.8229838658936556861, -0.5680647467311569221 ) ) ;
#3182 = AXIS2_PLACEMENT_3D ( 'NONE', #14593, #2749, #7219 ) ;
#3183 = VERTEX_POINT ( 'NONE', #36286 ) ;
#3184 = EDGE_CURVE ( 'NONE', #13909, #51040, #17118, .T. ) ;
#3185 = FACE_OUTER_BOUND ( 'NONE', #37672, .T. ) ;
#3186 = EDGE_CURVE ( 'NONE', #41791, #50590, #40225, .T. ) ;
#3187 = AXIS2_PLACEMENT_3D ( 'NONE', #17874, #21564, #37593 ) ;
#3188 = EDGE_LOOP ( 'NONE', ( #1250, #23013, #46451, #42945 ) ) ;
#3189 = ORIENTED_EDGE ( 'NONE', *, *, #22689, .F. ) ;
#3190 = EDGE_CURVE ( 'NONE', #39518, #23810, #284, .T. ) ;
#3191 = ORIENTED_EDGE ( 'NONE', *, *, #24243, .F. ) ;
#3192 = CARTESIAN_POINT ( 'NONE',  ( -332.3517673607765914, -119.0014323656137947, -58.88711093124865670 ) ) ;
#3193 = ADVANCED_FACE ( 'NONE', ( #4503 ), #28915, .T. ) ;
#3194 = CARTESIAN_POINT ( 'NONE',  ( -71.22983192549011733, -193.5000000000000000, -121.8950816227732759 ) ) ;
#3195 = ORIENTED_EDGE ( 'NONE', *, *, #34838, .T. ) ;
#3196 = EDGE_CURVE ( 'NONE', #2898, #19322, #17290, .T. ) ;
#3197 = DIRECTION ( 'NONE',  ( -1.000000000000000000, 0.000000000000000000, 0.000000000000000000 ) ) ;
#3198 = PLANE ( 'NONE',  #46230 ) ;
#3199 =( GEOMETRIC_REPRESENTATION_CONTEXT ( 3 ) GLOBAL_UNCERTAINTY_ASSIGNED_CONTEXT ( ( #15360 ) ) GLOBAL_UNIT_ASSIGNED_CONTEXT ( ( #35774, #38, #28405 ) ) REPRESENTATION_CONTEXT ( 'NONE', 'WORKASPACE' ) );
#3202 = VERTEX_POINT ( 'NONE', #44706 ) ;
#3201 = CARTESIAN_POINT ( 'NONE',  ( -339.1964088526558498, -156.6043281241916816, -48.84008046109114076 ) ) ;
#3200 = CARTESIAN_POINT ( 'NONE',  ( -330.4913330509368166, -103.0458197858332312, -55.34326076196081345 ) ) ;
#3203 = VECTOR ( 'NONE', #38566, 1000.000000000000000 ) ;
#3204 = DIRECTION ( 'NONE',  ( -0.000000000000000000, 1.000000000000000000, -0.000000000000000000 ) ) ;
#3205 = ORIENTED_EDGE ( 'NONE', *, *, #15658, .F. ) ;
#3206 = DIRECTION ( 'NONE',  ( -0.000000000000000000, 1.000000000000000000, -0.000000000000000000 ) ) ;
#3207 = AXIS2_PLACEMENT_3D ( 'NONE', #40724, #13407, #49155 ) ;
#3208 = EDGE_LOOP ( 'NONE', ( #33028, #12217, #24797, #7841 ) ) ;
#3209 = LINE ( 'NONE', #43136, #41701 ) ;
#3210 = LINE ( 'NONE', #36284, #21274 ) ;
#3212 = LINE ( 'NONE', #43913, #15596 ) ;
#3211 = DIRECTION ( 'NONE',  ( 1.000000000000000000, 0.000000000000000000, 0.000000000000000000 ) ) ;
#3213 = EDGE_CURVE ( 'NONE', #15652, #2485, #44976, .T. ) ;
#3214 = ORIENTED_EDGE ( 'NONE', *, *, #14447, .F. ) ;
#3215 = ADVANCED_FACE ( 'NONE', ( #16322 ), #44183, .T. ) ;
#3216 = CIRCLE ( 'NONE', #39296, 10.00000000000000000 ) ;
#3217 = DIRECTION ( 'NONE',  ( -0.8896570909947530970, 0.000000000000000000, 0.4566292373937018700 ) ) ;
#3218 = EDGE_LOOP ( 'NONE', ( #25213, #23302, #5416, #36452 ) ) ;
#3219 = DIRECTION ( 'NONE',  ( -1.000000000000000000, 0.000000000000000000, 0.000000000000000000 ) ) ;
#3220 = FACE_OUTER_BOUND ( 'NONE', #22079, .T. ) ;
#3221 = VERTEX_POINT ( 'NONE', #37067 ) ;
#3222 = CARTESIAN_POINT ( 'NONE',  ( -44.48323084606168720, -183.6283474603465606, 124.9361149384469769 ) ) ;
#3223 = CARTESIAN_POINT ( 'NONE',  ( -160.0666658415768211, -189.7472609257535510, 54.07611884703388228 ) ) ;
#3224 = ORIENTED_EDGE ( 'NONE', *, *, #49030, .F. ) ;
#3225 = FACE_BOUND ( 'NONE', #17860, .T. ) ;
#3226 = CARTESIAN_POINT ( 'NONE',  ( -339.1964088526558498, -68.15673923803898049, 20.45418021416614351 ) ) ;
#3227 = VECTOR ( 'NONE', #30725, 1000.000000000000114 ) ;
#3228 = VERTEX_POINT ( 'NONE', #40481 ) ;
#3229 = DIRECTION ( 'NONE',  ( -0.9995608365087946812, 0.000000000000000000, 0.02963332782254913048 ) ) ;
#3230 = VERTEX_POINT ( 'NONE', #5292 ) ;
#3231 = CARTESIAN_POINT ( 'NONE',  ( -32.87124591993210743, -189.7472609257535510, 124.0217483183788119 ) ) ;
#3232 = DIRECTION ( 'NONE',  ( -0.4216675885939772384, 0.4327645661435913227, -0.7968131995768452658 ) ) ;
#3233 = ORIENTED_EDGE ( 'NONE', *, *, #42858, .F. ) ;
#3234 = EDGE_CURVE ( 'NONE', #31475, #44335, #32337, .T. ) ;
#3235 = DIRECTION ( 'NONE',  ( 0.000000000000000000, -1.000000000000000000, 0.000000000000000000 ) ) ;
#3236 = FACE_OUTER_BOUND ( 'NONE', #16434, .T. ) ;
#3237 = LINE ( 'NONE', #11103, #27422 ) ;
#3238 = ADVANCED_FACE ( 'NONE', ( #21308 ), #28653, .T. ) ;
#3239 = EDGE_CURVE ( 'NONE', #42978, #2870, #16859, .T. ) ;
#3240 = DIRECTION ( 'NONE',  ( 0.000000000000000000, -1.000000000000000000, 0.000000000000000000 ) ) ;
#3241 = EDGE_CURVE ( 'NONE', #33090, #39789, #12099, .T. ) ;
#3242 = PRODUCT_DEFINITION_FORMATION_WITH_SPECIFIED_SOURCE ( 'ANY', '', #30214, .NOT_KNOWN. ) ;
#3243 = CIRCLE ( 'NONE', #27576, 125.0000000000000000 ) ;
#3244 = CIRCLE ( 'NONE', #11634, 125.0000000000000000 ) ;
#3245 = FACE_OUTER_BOUND ( 'NONE', #3352, .T. ) ;
#3246 = LINE ( 'NONE', #2970, #39435 ) ;
#3248 = EDGE_LOOP ( 'NONE', ( #17782, #36932, #27312, #37146 ) ) ;
#3247 = DIRECTION ( 'NONE',  ( 0.000000000000000000, 0.000000000000000000, -1.000000000000000000 ) ) ;
#3249 = CIRCLE ( 'NONE', #41845, 60.00000000000000000 ) ;
#3250 = ORIENTED_EDGE ( 'NONE', *, *, #19208, .F. ) ;
#3251 = FACE_OUTER_BOUND ( 'NONE', #51139, .T. ) ;
#3252 = DIRECTION ( 'NONE',  ( 0.000000000000000000, -0.5680647467311596976, -0.8229838658936536877 ) ) ;
#3253 = ORIENTED_EDGE ( 'NONE', *, *, #9309, .F. ) ;
#3254 = CIRCLE ( 'NONE', #29282, 15.24495751795539000 ) ;
#3255 = EDGE_LOOP ( 'NONE', ( #32611, #29820, #3806, #22783 ) ) ;
#3256 = LINE ( 'NONE', #31353, #44938 ) ;
#3257 = EDGE_LOOP ( 'NONE', ( #43605, #39198, #6591, #16806 ) ) ;
#3258 = CARTESIAN_POINT ( 'NONE',  ( -47.48307690889363641, -193.5000000000000000, 0.08879589532294547560 ) ) ;
#3259 = DIRECTION ( 'NONE',  ( 0.000000000000000000, -1.000000000000000000, -0.000000000000000000 ) ) ;
#3260 = CARTESIAN_POINT ( 'NONE',  ( -336.3521761649654422, -88.64083255475578937, 47.62880233550460218 ) ) ;
#3261 = FACE_OUTER_BOUND ( 'NONE', #23587, .T. ) ;
#3262 = ORIENTED_EDGE ( 'NONE', *, *, #33020, .T. ) ;
#3263 = ORIENTED_EDGE ( 'NONE', *, *, #21170, .T. ) ;
#3264 = ADVANCED_FACE ( 'NONE', ( #21048 ), #1064, .T. ) ;
#3265 = ORIENTED_EDGE ( 'NONE', *, *, #14125, .T. ) ;
#3266 = VECTOR ( 'NONE', #51190, 1000.000000000000000 ) ;
#3267 = DIRECTION ( 'NONE',  ( -0.000000000000000000, -0.8854560256532062468, 0.4647231720437755564 ) ) ;
#3268 = CARTESIAN_POINT ( 'NONE',  ( -330.4913330509368166, -84.00150778970767362, -43.83057281297470098 ) ) ;
#3269 = DIRECTION ( 'NONE',  ( -0.000000000000000000, 1.000000000000000000, 0.000000000000000000 ) ) ;
#3270 = LINE ( 'NONE', #35561, #11916 ) ;
#3271 = PLANE ( 'NONE',  #34788 ) ;
#3272 = ORIENTED_EDGE ( 'NONE', *, *, #34338, .F. ) ;
#3273 = DIRECTION ( 'NONE',  ( 0.000000000000000000, -1.000000000000000000, -0.000000000000000000 ) ) ;
#3274 = LINE ( 'NONE', #50849, #15651 ) ;
#3275 = VERTEX_POINT ( 'NONE', #45242 ) ;
#3276 = EDGE_LOOP ( 'NONE', ( #38813, #42717, #9615, #49268 ) ) ;
#3277 = DIRECTION ( 'NONE',  ( -0.9785564922995060311, 0.000000000000000000, 0.2059786187410889424 ) ) ;
#3279 = VECTOR ( 'NONE', #7, 1000.000000000000000 ) ;
#3278 = DIRECTION ( 'NONE',  ( -0.5586467658036535777, 0.000000000000000000, 0.8294056854502011022 ) ) ;
#3280 = ORIENTED_EDGE ( 'NONE', *, *, #2319, .T. ) ;
#3281 = DIRECTION ( 'NONE',  ( 0.000000000000000000, 0.000000000000000000, -1.000000000000000000 ) ) ;
#3282 = VECTOR ( 'NONE', #26512, 1000.000000000000227 ) ;
#3283 = CARTESIAN_POINT ( 'NONE',  ( -339.1964088526558498, -178.8432607619609485, -20.45418021416653076 ) ) ;
#3284 = PLANE ( 'NONE',  #41894 ) ;
#3285 = ORIENTED_EDGE ( 'NONE', *, *, #6170, .F. ) ;
#3286 = CARTESIAN_POINT ( 'NONE',  ( -339.1964088526558498, -182.1300919119128423, 6.615309698015510165 ) ) ;
#3287 = ORIENTED_EDGE ( 'NONE', *, *, #19178, .T. ) ;
#3288 = CARTESIAN_POINT ( 'NONE',  ( 60.00000000000001421, -93.32050807568917605, -51.65063509461091940 ) ) ;
#3289 = AXIS2_PLACEMENT_3D ( 'NONE', #28565, #4663, #36726 ) ;
#3290 = DIRECTION ( 'NONE',  ( -0.000000000000000000, 1.000000000000000000, 0.000000000000000000 ) ) ;
#3291 = EDGE_LOOP ( 'NONE', ( #31198, #37745, #12549, #584 ) ) ;
#3292 = CARTESIAN_POINT ( 'NONE',  ( -305.0000000000000568, -96.06030588028410477, 53.35787839313353942 ) ) ;
#3293 = CARTESIAN_POINT ( 'NONE',  ( -336.3521761649654422, -182.6878972721721084, 9.838334030658060669 ) ) ;
#3294 = CARTESIAN_POINT ( 'NONE',  ( -339.1964088526558498, -116.8846903019842927, 58.63009191191280678 ) ) ;
#3295 = EDGE_CURVE ( 'NONE', #39399, #14153, #9229, .T. ) ;
#3296 = LINE ( 'NONE', #4077, #47590 ) ;
#3297 = AXIS2_PLACEMENT_3D ( 'NONE', #30598, #51624, #11677 ) ;
#3298 = LINE ( 'NONE', #24302, #51346 ) ;
#3299 = EDGE_LOOP ( 'NONE', ( #46716, #35466, #17869, #16288 ) ) ;
#3300 = VERTEX_POINT ( 'NONE', #46271 ) ;
#3301 = CARTESIAN_POINT ( 'NONE',  ( -126.3604277550460750, -193.5000000000000000, 96.49160960477099991 ) ) ;
#3303 = ORIENTED_EDGE ( 'NONE', *, *, #47683, .T. ) ;
#3302 = PLANE ( 'NONE',  #30453 ) ;
#3304 = ORIENTED_EDGE ( 'NONE', *, *, #26166, .T. ) ;
#3305 = DIRECTION ( 'NONE',  ( 0.6528221181905227155, 0.000000000000000000, -0.7575112421616191360 ) ) ;
#3306 = PLANE ( 'NONE',  #9209 ) ;
#3307 = ORIENTED_EDGE ( 'NONE', *, *, #46155, .T. ) ;
#3308 = VECTOR ( 'NONE', #30906, 1000.000000000000000 ) ;
#3309 = CARTESIAN_POINT ( 'NONE',  ( -63.96873441216510514, -193.5000000000000000, -123.0287672223651612 ) ) ;
#3310 = DIRECTION ( 'NONE',  ( -1.000000000000000000, 9.758900497077107825E-15, -3.701062773504986041E-15 ) ) ;
#3311 = ADVANCED_FACE ( 'NONE', ( #34170 ), #29699, .F. ) ;
#3312 = ORIENTED_EDGE ( 'NONE', *, *, #3999, .F. ) ;
#3313 = DIRECTION ( 'NONE',  ( -0.000000000000000000, 1.000000000000000000, -0.000000000000000000 ) ) ;
#3314 = AXIS2_PLACEMENT_3D ( 'NONE', #24386, #13346, #48581 ) ;
#3315 = DIRECTION ( 'NONE',  ( -0.000000000000000000, -0.4647231720437631775, 0.8854560256532126861 ) ) ;
#3316 = DIRECTION ( 'NONE',  ( 1.000000000000000000, -0.000000000000000000, -0.000000000000000000 ) ) ;
#3317 = ORIENTED_EDGE ( 'NONE', *, *, #1641, .F. ) ;
#3318 = VERTEX_POINT ( 'NONE', #30475 ) ;
#3319 = ORIENTED_EDGE ( 'NONE', *, *, #29800, .T. ) ;
#3320 = FACE_OUTER_BOUND ( 'NONE', #40402, .T. ) ;
#3321 = DIRECTION ( 'NONE',  ( 0.000000000000000000, -1.000000000000000000, 0.000000000000000000 ) ) ;
#3322 = DIRECTION ( 'NONE',  ( 0.000000000000000000, -0.000000000000000000, 1.000000000000000000 ) ) ;
#3323 = CARTESIAN_POINT ( 'NONE',  ( -154.0877180371535928, -193.5000000000000000, -66.87170886601927577 ) ) ;
#3324 = DIRECTION ( 'NONE',  ( -1.000000000000000000, 0.000000000000000000, 0.000000000000000000 ) ) ;
#3325 = ORIENTED_EDGE ( 'NONE', *, *, #32706, .F. ) ;
#3326 = EDGE_CURVE ( 'NONE', #33929, #15769, #22077, .T. ) ;
#3327 = VECTOR ( 'NONE', #33820, 1000.000000000000000 ) ;
#3328 = CARTESIAN_POINT ( 'NONE',  ( -339.1964088526558498, -68.15673923803898049, 20.45418021416614351 ) ) ;
#3329 = ORIENTED_EDGE ( 'NONE', *, *, #5103, .T. ) ;
#3331 = EDGE_LOOP ( 'NONE', ( #41235, #21299, #11048, #39196 ) ) ;
#3330 = LINE ( 'NONE', #19362, #48305 ) ;
#3332 = ORIENTED_EDGE ( 'NONE', *, *, #37399, .F. ) ;
#3333 = ADVANCED_FACE ( 'NONE', ( #10252 ), #1330, .T. ) ;
#3334 = CARTESIAN_POINT ( 'NONE',  ( -48.30901192927175458, -189.7472609257535510, -123.9998842437354227 ) ) ;
#3335 = DIRECTION ( 'NONE',  ( -0.8124868780056863082, 0.000000000000000000, 0.5829794791144649047 ) ) ;
#3336 = CARTESIAN_POINT ( 'NONE',  ( 74.60098876342242136, -177.1207230881787780, 21.82395850507348811 ) ) ;
#3337 = CARTESIAN_POINT ( 'NONE',  ( -118.4510020108455137, -175.3837268820161057, 103.5805805771131674 ) ) ;
#3338 = EDGE_LOOP ( 'NONE', ( #51, #12060, #16979, #19414 ) ) ;
#3339 = DIRECTION ( 'NONE',  ( -0.1768902751225802927, 0.000000000000000000, 0.9842305779475953864 ) ) ;
#3340 = ORIENTED_EDGE ( 'NONE', *, *, #50117, .F. ) ;
#3341 = EDGE_CURVE ( 'NONE', #49982, #31272, #38096, .T. ) ;
#3342 = VERTEX_POINT ( 'NONE', #33408 ) ;
#3343 = CARTESIAN_POINT ( 'NONE',  ( -48.47912675150885065, -183.6283474603465606, 6.938893903907228378E-15 ) ) ;
#3344 = CARTESIAN_POINT ( 'NONE',  ( 8.750818922897904528, -175.3837268820161057, -111.1293539894138434 ) ) ;
#3345 = VECTOR ( 'NONE', #2353, 1000.000000000000000 ) ;
#3346 = DIRECTION ( 'NONE',  ( 0.7175072570443348230, 0.000000000000000000, -0.6965510290629933765 ) ) ;
#3347 = LINE ( 'NONE', #15447, #49201 ) ;
#3348 = PLANE ( 'NONE',  #34808 ) ;
#3349 = LINE ( 'NONE', #22285, #2003 ) ;
#3350 = DIRECTION ( 'NONE',  ( 0.000000000000000000, -9.251858538542971828E-16, -1.000000000000000000 ) ) ;
#3351 = ADVANCED_FACE ( 'NONE', ( #6583 ), #14210, .T. ) ;
#3352 = EDGE_LOOP ( 'NONE', ( #51491, #5309, #27605, #29110 ) ) ;
#3353 = DIRECTION ( 'NONE',  ( 0.000000000000000000, 0.000000000000000000, 1.000000000000000000 ) ) ;
#3354 = DIRECTION ( 'NONE',  ( 0.8455960035018234011, 0.000000000000000000, 0.5338233779647948429 ) ) ;
#3355 = EDGE_CURVE ( 'NONE', #43312, #40054, #1337, .T. ) ;
#3356 = FACE_OUTER_BOUND ( 'NONE', #1998, .T. ) ;
#3357 = ORIENTED_EDGE ( 'NONE', *, *, #51024, .F. ) ;
#3358 = ADVANCED_FACE ( 'NONE', ( #21580 ), #9740, .F. ) ;
#3359 = CARTESIAN_POINT ( 'NONE',  ( -146.2338470511239166, -193.5000000000000000, 76.29032973288703090 ) ) ;
#3360 = CYLINDRICAL_SURFACE ( 'NONE', #33676, 125.0000000000000000 ) ;
#3361 = ORIENTED_EDGE ( 'NONE', *, *, #2511, .F. ) ;
#3362 = DIRECTION ( 'NONE',  ( 0.000000000000000000, -0.9350162426854132791, 0.3546048870425396182 ) ) ;
#3363 = VERTEX_POINT ( 'NONE', #46518 ) ;
#3364 = AXIS2_PLACEMENT_3D ( 'NONE', #22470, #50329, #22198 ) ;
#3365 = AXIS2_PLACEMENT_3D ( 'NONE', #10603, #26108, #30063 ) ;
#3366 = DIRECTION ( 'NONE',  ( 1.000000000000000000, 0.000000000000000000, 0.000000000000000000 ) ) ;
#3367 = FACE_BOUND ( 'NONE', #35965, .T. ) ;
#3368 = CARTESIAN_POINT ( 'NONE',  ( -48.47912675150885065, -189.7472609257535510, -0.9999999999999931166 ) ) ;
#3369 = EDGE_CURVE ( 'NONE', #38792, #48181, #51830, .T. ) ;
#3370 = CARTESIAN_POINT ( 'NONE',  ( -40.24578378811990831, -189.7472609257535510, 124.7285535218268251 ) ) ;
#3371 = EDGE_LOOP ( 'NONE', ( #48236, #17245, #46757, #11428 ) ) ;
#3372 = VERTEX_POINT ( 'NONE', #13680 ) ;
#3373 = CARTESIAN_POINT ( 'NONE',  ( -365.0160704661291788, -113.5000000000000142, 39.99999999999998579 ) ) ;
#3374 = AXIS2_PLACEMENT_3D ( 'NONE', #51221, #7823, #27544 ) ;
#3375 = VERTEX_POINT ( 'NONE', #22334 ) ;
#3376 = DIRECTION ( 'NONE',  ( -0.000000000000000000, 1.000000000000000000, -0.000000000000000000 ) ) ;
#3377 = EDGE_CURVE ( 'NONE', #48181, #6100, #25504, .T. ) ;
#3378 = DIRECTION ( 'NONE',  ( -0.7378332790417333475, 0.000000000000000000, 0.6749830015182038956 ) ) ;
#3379 = DIRECTION ( 'NONE',  ( 0.000000000000000000, 0.000000000000000000, -1.000000000000000000 ) ) ;
#3380 = ORIENTED_EDGE ( 'NONE', *, *, #42330, .T. ) ;
#3383 = VERTEX_POINT ( 'NONE', #1604 ) ;
#3382 = DIRECTION ( 'NONE',  ( 0.000000000000000000, 0.000000000000000000, -1.000000000000000000 ) ) ;
#3381 = DIRECTION ( 'NONE',  ( 0.000000000000000000, 0.1205366802553130001, -0.9927088740980551940 ) ) ;
#3384 = LINE ( 'NONE', #7842, #26468 ) ;
#3385 = EDGE_LOOP ( 'NONE', ( #29736, #48906, #996, #36839 ) ) ;
#3386 = CARTESIAN_POINT ( 'NONE',  ( 28.02885774092381865, -193.5000000000000000, 98.85104101073331151 ) ) ;
#3387 = EDGE_LOOP ( 'NONE', ( #6035, #27977, #39490, #33390 ) ) ;
#3388 = ADVANCED_FACE ( 'NONE', ( #17640 ), #33647, .F. ) ;
#3389 = ADVANCED_FACE ( 'NONE', ( #50470 ), #5822, .T. ) ;
#3390 = CARTESIAN_POINT ( 'NONE',  ( -339.1964088526558498, -68.15673923803898049, 20.45418021416614351 ) ) ;
#3391 = ORIENTED_EDGE ( 'NONE', *, *, #16645, .T. ) ;
#3393 = DIRECTION ( 'NONE',  ( 0.000000000000000000, 1.047444401652940007E-14, 1.000000000000000000 ) ) ;
#3392 = DIRECTION ( 'NONE',  ( 0.000000000000000000, 0.000000000000000000, 1.000000000000000000 ) ) ;
#3394 = ORIENTED_EDGE ( 'NONE', *, *, #20125, .F. ) ;
#3395 = AXIS2_PLACEMENT_3D ( 'NONE', #12085, #47612, #11592 ) ;
#3396 = VECTOR ( 'NONE', #43940, 1000.000000000000000 ) ;
#3397 = DIRECTION ( 'NONE',  ( 0.000000000000000000, 1.000000000000000000, 0.000000000000000000 ) ) ;
#3398 = ORIENTED_EDGE ( 'NONE', *, *, #3355, .F. ) ;
#3399 = DIRECTION ( 'NONE',  ( -0.000000000000000000, 0.9350162426854146114, -0.3546048870425363986 ) ) ;
#3400 = DIRECTION ( 'NONE',  ( 0.000000000000000000, -0.000000000000000000, -1.000000000000000000 ) ) ;
#3401 = DIRECTION ( 'NONE',  ( 1.000000000000000000, 0.000000000000000000, 0.000000000000000000 ) ) ;
#3402 = DIRECTION ( 'NONE',  ( 0.1768902751225802927, 0.000000000000000000, -0.9842305779475953864 ) ) ;
#3403 = CARTESIAN_POINT ( 'NONE',  ( -155.9608607592036833, -177.1207230881787780, 63.81752780153064464 ) ) ;
#3404 = FACE_OUTER_BOUND ( 'NONE', #15358, .T. ) ;
#3405 = ORIENTED_EDGE ( 'NONE', *, *, #13325, .F. ) ;
#3406 = EDGE_CURVE ( 'NONE', #46459, #8474, #36736, .T. ) ;
#3407 = LINE ( 'NONE', #6844, #23762 ) ;
#3408 = DIRECTION ( 'NONE',  ( 1.000000000000000000, 0.000000000000000000, 0.000000000000000000 ) ) ;
#3409 = EDGE_CURVE ( 'NONE', #44223, #31469, #13220, .T. ) ;
#3410 = PLANE ( 'NONE',  #39661 ) ;
#3411 = VERTEX_POINT ( 'NONE', #49945 ) ;
#3412 = ADVANCED_FACE ( 'NONE', ( #38365 ), #42294, .T. ) ;
#3413 = AXIS2_PLACEMENT_3D ( 'NONE', #41633, #49804, #37435 ) ;
#3414 = CARTESIAN_POINT ( 'NONE',  ( -33.86391487983341619, -193.5000000000000000, 124.1426420773540542 ) ) ;
#3415 = DIRECTION ( 'NONE',  ( 0.000000000000000000, 1.000000000000000000, 0.000000000000000000 ) ) ;
#3416 = ADVANCED_FACE ( 'NONE', ( #2877 ), #34673, .F. ) ;
#3417 = CARTESIAN_POINT ( 'NONE',  ( 75.17589904515341459, -189.7472609257535510, -18.28755301364250840 ) ) ;
#3419 = VERTEX_POINT ( 'NONE', #50721 ) ;
#3418 = FACE_OUTER_BOUND ( 'NONE', #12100, .T. ) ;
#3420 = ORIENTED_EDGE ( 'NONE', *, *, #51153, .F. ) ;
#3421 = ORIENTED_EDGE ( 'NONE', *, *, #12545, .F. ) ;
#3422 = DIRECTION ( 'NONE',  ( -0.000000000000000000, -0.4647231720437604574, 0.8854560256532141294 ) ) ;
#3423 = DIRECTION ( 'NONE',  ( 0.000000000000000000, 0.000000000000000000, 1.000000000000000000 ) ) ;
#3424 = CARTESIAN_POINT ( 'NONE',  ( 75.48400724637754422, -177.1207230881787780, -16.06677968424457248 ) ) ;
#3425 = LINE ( 'NONE', #10802, #22018 ) ;
#3426 = VECTOR ( 'NONE', #34753, 999.9999999999998863 ) ;
#3427 = ORIENTED_EDGE ( 'NONE', *, *, #27561, .F. ) ;
#3428 = CARTESIAN_POINT ( 'NONE',  ( 3.372329702444478272, 56.71331670983759921, -17.05911205401795172 ) ) ;
#3429 = AXIS2_PLACEMENT_3D ( 'NONE', #42594, #6608, #22630 ) ;
#3430 = ORIENTED_EDGE ( 'NONE', *, *, #28488, .F. ) ;
#3431 = ORIENTED_EDGE ( 'NONE', *, *, #7986, .T. ) ;
#3432 = VERTEX_POINT ( 'NONE', #35443 ) ;
#3433 = CARTESIAN_POINT ( 'NONE',  ( -238.7407812814481076, -213.5000000000000000, 41.45482488023466772 ) ) ;
#3434 = CARTESIAN_POINT ( 'NONE',  ( -137.9639882952644143, -177.1207230881787780, 87.27805883780240492 ) ) ;
#3435 = VERTEX_POINT ( 'NONE', #22856 ) ;
#3436 = CARTESIAN_POINT ( 'NONE',  ( -330.4913330509368166, -64.99044476834235695, 7.608018572112246858 ) ) ;
#3437 = PLANE ( 'NONE',  #41171 ) ;
#3440 = ORIENTED_EDGE ( 'NONE', *, *, #33669, .F. ) ;
#3439 = FACE_OUTER_BOUND ( 'NONE', #15433, .T. ) ;
#3438 = DIRECTION ( 'NONE',  ( -0.7765238627180437447, 0.000000000000000000, 0.6300878435817094392 ) ) ;
#3441 = EDGE_CURVE ( 'NONE', #6834, #16650, #6830, .T. ) ;
#3442 = DIRECTION ( 'NONE',  ( 0.000000000000000000, 0.000000000000000000, 1.000000000000000000 ) ) ;
#3443 = ORIENTED_EDGE ( 'NONE', *, *, #29152, .T. ) ;
#3444 = FACE_OUTER_BOUND ( 'NONE', #21415, .T. ) ;
#3445 = EDGE_LOOP ( 'NONE', ( #14608, #14809, #20458, #12759 ) ) ;
#3446 = EDGE_CURVE ( 'NONE', #47743, #3034, #15233, .T. ) ;
#3447 = EDGE_CURVE ( 'NONE', #978, #42791, #38875, .T. ) ;
#3448 = EDGE_CURVE ( 'NONE', #716, #19679, #26645, .T. ) ;
#3449 = PLANE ( 'NONE',  #28266 ) ;
#3450 = CARTESIAN_POINT ( 'NONE',  ( -48.13092511607445090, -189.7472609257535510, -0.9374196611341135688 ) ) ;
#3452 = LINE ( 'NONE', #47624, #35728 ) ;
#3451 = DIRECTION ( 'NONE',  ( 0.000000000000000000, 0.000000000000000000, -1.000000000000000000 ) ) ;
#3453 = ORIENTED_EDGE ( 'NONE', *, *, #34271, .F. ) ;
#3454 = ADVANCED_FACE ( 'NONE', ( #11013 ), #42821, .T. ) ;
#3455 = DIRECTION ( 'NONE',  ( -0.000000000000000000, -1.000000000000000000, 0.000000000000000000 ) ) ;
#3456 = CARTESIAN_POINT ( 'NONE',  ( 5.139251539934009294, -193.5000000000000000, 111.8087531435658093 ) ) ;
#3457 = SHAPE_REPRESENTATION_RELATIONSHIP ( 'NONE' , 'NONE' ,  #2890, #36813 ) ;
#3458 = ORIENTED_EDGE ( 'NONE', *, *, #48473, .F. ) ;
#3459 = EDGE_CURVE ( 'NONE', #28559, #14905, #39387, .T. ) ;
#3460 = LINE ( 'NONE', #15560, #14024 ) ;
#3461 = AXIS2_PLACEMENT_3D ( 'NONE', #44854, #17534, #33547 ) ;
#3462 = LINE ( 'NONE', #18471, #31550 ) ;
#3463 = ORIENTED_EDGE ( 'NONE', *, *, #6080, .F. ) ;
#3464 = LINE ( 'NONE', #15838, #49439 ) ;
#3465 = ADVANCED_FACE ( 'NONE', ( #7851 ), #14716, .F. ) ;
#3466 = CARTESIAN_POINT ( 'NONE',  ( 70.19984492582109681, -189.7472609257535510, 39.24667733211968823 ) ) ;
#3467 = EDGE_CURVE ( 'NONE', #50634, #25658, #43347, .T. ) ;
#3468 = ORIENTED_EDGE ( 'NONE', *, *, #40786, .F. ) ;
#3469 = DIRECTION ( 'NONE',  ( 0.000000000000000000, 0.000000000000000000, 1.000000000000000000 ) ) ;
#3470 = VERTEX_POINT ( 'NONE', #51495 ) ;
#3471 = EDGE_CURVE ( 'NONE', #194, #34268, #35193, .T. ) ;
#3472 = CARTESIAN_POINT ( 'NONE',  ( -336.3521761649654422, -64.61288906875131488, 4.498567634385603142 ) ) ;
#3473 = FACE_OUTER_BOUND ( 'NONE', #49138, .T. ) ;
#3474 = ADVANCED_FACE ( 'NONE', ( #26791 ), #27813, .F. ) ;
#3475 = DIRECTION ( 'NONE',  ( 0.000000000000000000, 1.000000000000000000, -0.000000000000000000 ) ) ;
#3476 = CARTESIAN_POINT ( 'NONE',  ( 57.66105628977221897, -189.7472609257535510, 66.02470404298190942 ) ) ;
#3477 = LINE ( 'NONE', #31077, #20716 ) ;
#3478 = AXIS2_PLACEMENT_3D ( 'NONE', #45075, #48227, #120 ) ;
#3479 = EDGE_CURVE ( 'NONE', #20894, #30266, #11543, .T. ) ;
#3480 = CARTESIAN_POINT ( 'NONE',  ( -339.1964088526558498, -123.5000000000000284, 0.000000000000000000 ) ) ;
#3481 = VECTOR ( 'NONE', #19868, 1000.000000000000000 ) ;
#3482 = CARTESIAN_POINT ( 'NONE',  ( 74.77174840718836890, -177.1207230881787780, 20.83798868929603643 ) ) ;
#3483 = FACE_OUTER_BOUND ( 'NONE', #8475, .T. ) ;
#3485 = ORIENTED_EDGE ( 'NONE', *, *, #45972, .F. ) ;
#3484 = CARTESIAN_POINT ( 'NONE',  ( -131.8938452225253855, -193.5000000000000000, 93.09664195018558530 ) ) ;
#3486 = ORIENTED_EDGE ( 'NONE', *, *, #22210, .T. ) ;
#3487 = LINE ( 'NONE', #35538, #45911 ) ;
#3488 = EDGE_CURVE ( 'NONE', #16247, #46453, #38618, .T. ) ;
#3489 = CARTESIAN_POINT ( 'NONE',  ( -336.3521761649654422, -123.5000000000000284, 0.000000000000000000 ) ) ;
#3490 = EDGE_LOOP ( 'NONE', ( #22008, #24921, #2727, #5005 ) ) ;
#3491 = ORIENTED_EDGE ( 'NONE', *, *, #37226, .T. ) ;
#3492 = CARTESIAN_POINT ( 'NONE',  ( -10.02015192278479816, -193.5000000000000000, -117.8859915627474351 ) ) ;
#3493 = ORIENTED_EDGE ( 'NONE', *, *, #21501, .F. ) ;
#3494 = CARTESIAN_POINT ( 'NONE',  ( -330.4913330509368166, -168.7406467949208491, -39.41172259083864304 ) ) ;
#3495 = DIRECTION ( 'NONE',  ( 0.000000000000000000, 0.000000000000000000, -1.000000000000000000 ) ) ;
#3496 = AXIS2_PLACEMENT_3D ( 'NONE', #50222, #31000, #46789 ) ;
#3497 = CARTESIAN_POINT ( 'NONE',  ( -96.65280530915693191, -183.6283474603465606, -115.3442529744087466 ) ) ;
#3498 = CARTESIAN_POINT ( 'NONE',  ( -5.732832253866456007, -193.5000000000000000, -117.4638425504666657 ) ) ;
#3499 = CIRCLE ( 'NONE', #26911, 125.0000000000000000 ) ;
#3500 = ORIENTED_EDGE ( 'NONE', *, *, #50402, .F. ) ;
#3501 = ORIENTED_EDGE ( 'NONE', *, *, #7872, .F. ) ;
#3503 = ORIENTED_EDGE ( 'NONE', *, *, #40056, .F. ) ;
#3502 = VECTOR ( 'NONE', #15020, 1000.000000000000000 ) ;
#3504 = EDGE_CURVE ( 'NONE', #17026, #15537, #23119, .T. ) ;
#3505 = CARTESIAN_POINT ( 'NONE',  ( -167.1668396246903114, -183.6283474603465606, -35.90758392117663078 ) ) ;
#3506 = CARTESIAN_POINT ( 'NONE',  ( 72.95485052494851175, -177.1207230881787780, -29.64437826672757481 ) ) ;
#3507 = DIRECTION ( 'NONE',  ( 1.000000000000000000, 0.000000000000000000, -6.978251959525016136E-17 ) ) ;
#3508 = CARTESIAN_POINT ( 'NONE',  ( 62.86098202833237281, -177.1207230881787780, 56.81883646197908178 ) ) ;
#3509 = DIRECTION ( 'NONE',  ( 0.8858462335218260097, 0.000000000000000000, 0.4639789333096864810 ) ) ;
#3510 = ORIENTED_EDGE ( 'NONE', *, *, #20220, .T. ) ;
#3511 = PLANE ( 'NONE',  #37265 ) ;
#3512 = EDGE_CURVE ( 'NONE', #32383, #25127, #28319, .T. ) ;
#3513 = EDGE_CURVE ( 'NONE', #8223, #41791, #3650, .T. ) ;
#3514 = EDGE_CURVE ( 'NONE', #27512, #39811, #15771, .T. ) ;
#3515 = DIRECTION ( 'NONE',  ( 0.9646355819083594074, 0.000000000000000000, -0.2635871660690647933 ) ) ;
#3516 = LINE ( 'NONE', #15363, #4729 ) ;
#3517 = AXIS2_PLACEMENT_3D ( 'NONE', #39236, #31600, #7449 ) ;
#3518 = EDGE_CURVE ( 'NONE', #32642, #26711, #11787, .T. ) ;
#3519 = ORIENTED_EDGE ( 'NONE', *, *, #6256, .T. ) ;
#3520 = ORIENTED_EDGE ( 'NONE', *, *, #42548, .T. ) ;
#3521 = CIRCLE ( 'NONE', #24526, 125.0000000000000000 ) ;
#3522 = EDGE_LOOP ( 'NONE', ( #20710, #17163, #20618, #27399 ) ) ;
#3523 = CIRCLE ( 'NONE', #29518, 124.9999999999999858 ) ;
#3524 = DIRECTION ( 'NONE',  ( 0.000000000000000000, 0.000000000000000000, 1.000000000000000000 ) ) ;
#3525 = CARTESIAN_POINT ( 'NONE',  ( 51.65665342072240662, -193.5000000000000000, 74.81861753132422166 ) ) ;
#3526 = ORIENTED_EDGE ( 'NONE', *, *, #49473, .T. ) ;
#3527 = CARTESIAN_POINT ( 'NONE',  ( -330.4913330509368166, -123.5000000000000284, 0.000000000000000000 ) ) ;
#3528 = CARTESIAN_POINT ( 'NONE',  ( 16.59365244519689497, -177.1207230881787780, -105.5544085257710805 ) ) ;
#3529 = FACE_OUTER_BOUND ( 'NONE', #18600, .T. ) ;
#3530 = ORIENTED_EDGE ( 'NONE', *, *, #3037, .T. ) ;
#3531 = CARTESIAN_POINT ( 'NONE',  ( 3.686287386450715076E-15, 20.00000000000000000, -51.00000000000000711 ) ) ;
#3532 = ORIENTED_EDGE ( 'NONE', *, *, #5088, .T. ) ;
#3533 = CARTESIAN_POINT ( 'NONE',  ( -330.4913330509368166, -172.3400804610915031, -33.10432812419114157 ) ) ;
#3534 = ADVANCED_FACE ( 'NONE', ( #40171 ), #8119, .F. ) ;
#3535 = CARTESIAN_POINT ( 'NONE',  ( -140.5933766095837427, -193.5000000000000000, -84.49831343337065448 ) ) ;
#3536 = VERTEX_POINT ( 'NONE', #40674 ) ;
#3537 = AXIS2_PLACEMENT_3D ( 'NONE', #27575, #39391, #28346 ) ;
#3538 = EDGE_CURVE ( 'NONE', #40265, #21496, #4186, .T. ) ;
#3539 = DIRECTION ( 'NONE',  ( 0.8980129913408354536, 0.4399689391117108661, 0.000000000000000000 ) ) ;
#3540 = DIRECTION ( 'NONE',  ( 0.000000000000000000, 0.000000000000000000, -1.000000000000000000 ) ) ;
#3541 = CARTESIAN_POINT ( 'NONE',  ( -46.00000000000000711, 20.00000000000000000, 46.00000000000000000 ) ) ;
#3542 = CARTESIAN_POINT ( 'NONE',  ( -59.86929868745821182, -177.1207230881787780, -124.4799742258549600 ) ) ;
#3543 = EDGE_CURVE ( 'NONE', #2646, #9485, #17440, .T. ) ;
#3544 = AXIS2_PLACEMENT_3D ( 'NONE', #17089, #5521, #33095 ) ;
#3545 = CARTESIAN_POINT ( 'NONE',  ( -305.0000000000000568, -102.6919536717979184, -56.27632902032075890 ) ) ;
#3546 = ORIENTED_EDGE ( 'NONE', *, *, #5199, .T. ) ;
#3547 = VERTEX_POINT ( 'NONE', #32552 ) ;
#3548 = CARTESIAN_POINT ( 'NONE',  ( -339.1964088526558498, -131.1080185721124849, 58.50955523165764305 ) ) ;
#3550 = EDGE_LOOP ( 'NONE', ( #720, #32785, #16918, #35231 ) ) ;
#3549 = LINE ( 'NONE', #8013, #32962 ) ;
#3551 = ORIENTED_EDGE ( 'NONE', *, *, #4791, .T. ) ;
#3552 = PLANE ( 'NONE',  #34659 ) ;
#3553 = VECTOR ( 'NONE', #33873, 1000.000000000000000 ) ;
#3554 = AXIS2_PLACEMENT_3D ( 'NONE', #23508, #629, #4057 ) ;
#3555 = DIRECTION ( 'NONE',  ( -0.000000000000000000, 1.000000000000000000, -0.000000000000000000 ) ) ;
#3556 = VECTOR ( 'NONE', #19381, 1000.000000000000000 ) ;
#3557 = AXIS2_PLACEMENT_3D ( 'NONE', #42425, #30334, #46386 ) ;
#3558 = ORIENTED_EDGE ( 'NONE', *, *, #26310, .F. ) ;
#3559 = DIRECTION ( 'NONE',  ( -0.000000000000000000, -0.5680647467311569221, -0.8229838658936556861 ) ) ;
#3560 = CARTESIAN_POINT ( 'NONE',  ( -166.6265240196292439, -189.7472609257535510, 40.81902153125349031 ) ) ;
#3561 = ORIENTED_EDGE ( 'NONE', *, *, #20174, .T. ) ;
#3562 = CARTESIAN_POINT ( 'NONE',  ( -339.1964088526558498, -143.9541802141663709, 55.34326076196097688 ) ) ;
#3563 = DIRECTION ( 'NONE',  ( 1.000000000000000000, 0.000000000000000000, -0.000000000000000000 ) ) ;
#3564 = PLANE ( 'NONE',  #16864 ) ;
#3565 = DIRECTION ( 'NONE',  ( 0.000000000000000000, 0.000000000000000000, 1.000000000000000000 ) ) ;
#3566 = EDGE_LOOP ( 'NONE', ( #46580, #2918, #43455, #41000 ) ) ;
#3567 = EDGE_LOOP ( 'NONE', ( #42805, #46246, #43625, #13778 ) ) ;
#3568 = ORIENTED_EDGE ( 'NONE', *, *, #4402, .F. ) ;
#3569 = LINE ( 'NONE', #31946, #6456 ) ;
#3570 = DIRECTION ( 'NONE',  ( -0.000000000000000000, 1.000000000000000000, -0.000000000000000000 ) ) ;
#3571 = DIRECTION ( 'NONE',  ( -0.9960498426152177842, 0.000000000000000000, 0.08879589532292482545 ) ) ;
#3572 = ADVANCED_BREP_SHAPE_REPRESENTATION ( '', ( #18958, #31742 ), #42661 ) ;
#3573 = FACE_OUTER_BOUND ( 'NONE', #49897, .T. ) ;
#3574 = FACE_OUTER_BOUND ( 'NONE', #7080, .T. ) ;
#3575 = VECTOR ( 'NONE', #48792, 1000.000000000000114 ) ;
#3576 = EDGE_LOOP ( 'NONE', ( #33450, #11548, #45678, #21384 ) ) ;
#3577 = EDGE_CURVE ( 'NONE', #21083, #43984, #39245, .T. ) ;
#3578 = EDGE_CURVE ( 'NONE', #18160, #44807, #12042, .T. ) ;
#3579 = AXIS2_PLACEMENT_3D ( 'NONE', #33927, #46051, #2651 ) ;
#3580 = DIRECTION ( 'NONE',  ( 0.000000000000000000, 1.000000000000000000, 0.000000000000000000 ) ) ;
#3581 = EDGE_LOOP ( 'NONE', ( #29738, #22166, #15045, #4362 ) ) ;
#3583 = EDGE_LOOP ( 'NONE', ( #15764, #3824, #5741, #16773 ) ) ;
#3582 = FACE_OUTER_BOUND ( 'NONE', #7751, .T. ) ;
#3584 = VERTEX_POINT ( 'NONE', #8634 ) ;
#3585 = CARTESIAN_POINT ( 'NONE',  ( 60.02977459919873837, -189.7472609257535510, 60.01515274641012354 ) ) ;
#3586 = DIRECTION ( 'NONE',  ( 0.000000000000000000, 0.000000000000000000, 1.000000000000000000 ) ) ;
#3587 = DIRECTION ( 'NONE',  ( -0.000000000000000000, -1.000000000000000000, 0.000000000000000000 ) ) ;
#3588 = CARTESIAN_POINT ( 'NONE',  ( -81.14588623932559130, -193.5000000000000000, 120.6560517527618117 ) ) ;
#3589 = VERTEX_POINT ( 'NONE', #36476 ) ;
#3590 = PLANE ( 'NONE',  #36779 ) ;
#3591 = EDGE_LOOP ( 'NONE', ( #33582, #4812, #21268, #17034 ) ) ;
#3592 = AXIS2_PLACEMENT_3D ( 'NONE', #10470, #34643, #23354 ) ;
#3593 = ORIENTED_EDGE ( 'NONE', *, *, #34601, .F. ) ;
#3594 = CARTESIAN_POINT ( 'NONE',  ( -140.5285791076019279, -193.5000000000000000, -83.08371579725672973 ) ) ;
#3595 = VECTOR ( 'NONE', #37562, 1000.000000000000114 ) ;
#3597 = AXIS2_PLACEMENT_3D ( 'NONE', #2464, #26367, #6670 ) ;
#3596 = DIRECTION ( 'NONE',  ( -0.000000000000000000, 0.7485107481711089639, 0.6631226582407863113 ) ) ;
#3598 = EDGE_CURVE ( 'NONE', #20728, #14521, #45183, .T. ) ;
#3599 = LINE ( 'NONE', #35393, #38722 ) ;
#3600 = DIRECTION ( 'NONE',  ( -0.000000000000000000, -1.000000000000000000, 0.000000000000000000 ) ) ;
#3601 = CARTESIAN_POINT ( 'NONE',  ( -62.43888699632653783, -189.7472609257535510, 124.2180546213279371 ) ) ;
#3602 = DIRECTION ( 'NONE',  ( 0.000000000000000000, 1.000000000000000000, 0.000000000000000000 ) ) ;
#3603 = CARTESIAN_POINT ( 'NONE',  ( -48.47912675150885065, -121.5000000000000142, -14.99999999999999289 ) ) ;
#3604 = AXIS2_PLACEMENT_3D ( 'NONE', #8347, #20686, #44356 ) ;
#3605 = ORIENTED_EDGE ( 'NONE', *, *, #18593, .F. ) ;
#3606 = LINE ( 'NONE', #31731, #14611 ) ;
#3607 = DIRECTION ( 'NONE',  ( 1.000000000000000000, -0.000000000000000000, 0.000000000000000000 ) ) ;
#3608 = EDGE_CURVE ( 'NONE', #8376, #42588, #35046, .T. ) ;
#3609 = DIRECTION ( 'NONE',  ( 0.000000000000000000, 0.000000000000000000, -1.000000000000000000 ) ) ;
#3610 = ORIENTED_EDGE ( 'NONE', *, *, #799, .T. ) ;
#3611 = CARTESIAN_POINT ( 'NONE',  ( -47.60339180931321579, -175.3837268820161057, -0.4827922027307358088 ) ) ;
#3612 = AXIS2_PLACEMENT_3D ( 'NONE', #17524, #28534, #24602 ) ;
#3613 = CARTESIAN_POINT ( 'NONE',  ( -170.0000000000000284, -123.5000000000000284, -37.63467731922663972 ) ) ;
#3614 = ORIENTED_EDGE ( 'NONE', *, *, #26310, .T. ) ;
#3615 = DIRECTION ( 'NONE',  ( -0.5085311186492216251, 0.000000000000000000, 0.8610436117673548884 ) ) ;
#3616 = VERTEX_POINT ( 'NONE', #20202 ) ;
#3617 = VECTOR ( 'NONE', #19775, 1000.000000000000000 ) ;
#3618 = DIRECTION ( 'NONE',  ( -0.8896570909947530970, 0.000000000000000000, 0.4566292373937018700 ) ) ;
#3619 = FACE_BOUND ( 'NONE', #26900, .T. ) ;
#3621 = EDGE_LOOP ( 'NONE', ( #35276, #11424, #48111, #42430 ) ) ;
#3620 = LINE ( 'NONE', #28312, #46412 ) ;
#3623 = CIRCLE ( 'NONE', #45591, 125.0000000000000000 ) ;
#3622 = LINE ( 'NONE', #39366, #20176 ) ;
#3624 = VERTEX_POINT ( 'NONE', #1005 ) ;
#3625 = EDGE_CURVE ( 'NONE', #20913, #8106, #40417, .T. ) ;
#3626 = VERTEX_POINT ( 'NONE', #8892 ) ;
#3627 = DIRECTION ( 'NONE',  ( -0.000000000000000000, 1.000000000000000000, -0.000000000000000000 ) ) ;
#3628 = VECTOR ( 'NONE', #8719, 1000.000000000000000 ) ;
#3629 = EDGE_LOOP ( 'NONE', ( #49421, #45910, #36646, #26374 ) ) ;
#3630 = CARTESIAN_POINT ( 'NONE',  ( 60.00000000000001421, -43.50000000000000000, 0.000000000000000000 ) ) ;
#3631 = DIRECTION ( 'NONE',  ( 0.000000000000000000, 0.000000000000000000, -1.000000000000000000 ) ) ;
#3632 = EDGE_CURVE ( 'NONE', #21416, #51078, #4440, .T. ) ;
#3633 = CIRCLE ( 'NONE', #39709, 25.00456841203573077 ) ;
#3634 = PLANE ( 'NONE',  #30093 ) ;
#3635 = CARTESIAN_POINT ( 'NONE',  ( 64.46023522152407281, -177.1207230881787780, -51.19472891551279758 ) ) ;
#3636 = EDGE_LOOP ( 'NONE', ( #41958, #31796, #11032, #22327 ) ) ;
#3639 = ORIENTED_EDGE ( 'NONE', *, *, #16504, .T. ) ;
#3638 =( NAMED_UNIT ( * ) PLANE_ANGLE_UNIT ( ) SI_UNIT ( $, .RADIAN. ) );
#3637 = DIRECTION ( 'NONE',  ( 0.000000000000000000, -0.9927088740980551940, -0.1205366802553130001 ) ) ;
#3640 = EDGE_CURVE ( 'NONE', #21717, #19973, #48601, .T. ) ;
#3641 = ORIENTED_EDGE ( 'NONE', *, *, #27551, .T. ) ;
#3642 = DIRECTION ( 'NONE',  ( -0.000000000000000000, 1.000000000000000000, -0.000000000000000000 ) ) ;
#3643 = ORIENTED_EDGE ( 'NONE', *, *, #33662, .T. ) ;
#3644 = DIRECTION ( 'NONE',  ( -0.000000000000000000, 1.000000000000000000, -0.000000000000000000 ) ) ;
#3645 = CIRCLE ( 'NONE', #41390, 125.0000000000000000 ) ;
#3646 = ORIENTED_EDGE ( 'NONE', *, *, #45292, .T. ) ;
#3647 = CARTESIAN_POINT ( 'NONE',  ( -48.47912675150885065, -189.7472609257535510, 6.938893903907228378E-15 ) ) ;
#3648 = VERTEX_POINT ( 'NONE', #12577 ) ;
#3650 = LINE ( 'NONE', #19677, #34226 ) ;
#3649 = PLANE ( 'NONE',  #39999 ) ;
#3651 = EDGE_LOOP ( 'NONE', ( #3780, #414, #50924, #21620 ) ) ;
#3652 = AXIS2_PLACEMENT_3D ( 'NONE', #13894, #21001, #1017 ) ;
#3653 = CARTESIAN_POINT ( 'NONE',  ( -336.3521761649654422, -173.5513585866778214, -31.34948880313881503 ) ) ;
#3654 = ORIENTED_EDGE ( 'NONE', *, *, #25015, .T. ) ;
#3655 = DIRECTION ( 'NONE',  ( -1.000000000000000000, 0.000000000000000000, -0.000000000000000000 ) ) ;
#3656 = DIRECTION ( 'NONE',  ( 0.000000000000000000, 0.000000000000000000, 1.000000000000000000 ) ) ;
#3657 = EDGE_CURVE ( 'NONE', #16597, #12335, #31708, .T. ) ;
#3658 = LINE ( 'NONE', #52037, #37267 ) ;
#3659 = PLANE ( 'NONE',  #19945 ) ;
#3660 = DIRECTION ( 'NONE',  ( -0.000000000000000000, 1.000000000000000000, -0.000000000000000000 ) ) ;
#3661 = FACE_OUTER_BOUND ( 'NONE', #318, .T. ) ;
#3662 = ADVANCED_FACE ( 'NONE', ( #12832 ), #32277, .F. ) ;
#3663 = ORIENTED_EDGE ( 'NONE', *, *, #17023, .F. ) ;
#3664 = SHAPE_REPRESENTATION_RELATIONSHIP ( 'NONE' , 'NONE' ,  #24080, #28043 ) ;
#3665 = VECTOR ( 'NONE', #41584, 1000.000000000000000 ) ;
#3666 = LINE ( 'NONE', #19963, #26308 ) ;
#3667 = CARTESIAN_POINT ( 'NONE',  ( -48.47912675150885065, -189.7472609257535510, 6.938893903907228378E-15 ) ) ;
#3668 = CARTESIAN_POINT ( 'NONE',  ( 62.86098202833237281, -193.5000000000000000, 56.81883646197908178 ) ) ;
#3669 = ORIENTED_EDGE ( 'NONE', *, *, #2858, .F. ) ;
#3670 = DIRECTION ( 'NONE',  ( -0.000000000000000000, -1.000000000000000000, -0.000000000000000000 ) ) ;
#3671 = DIRECTION ( 'NONE',  ( 0.000000000000000000, -1.000000000000000000, 0.000000000000000000 ) ) ;
#3673 = ORIENTED_EDGE ( 'NONE', *, *, #11166, .F. ) ;
#3672 = DIRECTION ( 'NONE',  ( 0.000000000000000000, 0.9927088740980530845, -0.1205366802553303057 ) ) ;
#3674 = ORIENTED_EDGE ( 'NONE', *, *, #11614, .T. ) ;
#3675 = ORIENTED_EDGE ( 'NONE', *, *, #4659, .F. ) ;
#3676 = CARTESIAN_POINT ( 'NONE',  ( -332.3517673607765914, -97.52665284734005979, -53.00046796564681983 ) ) ;
#3677 = CARTESIAN_POINT ( 'NONE',  ( -336.3521761649653854, -97.07224986041923387, -53.86626052140510978 ) ) ;
#3678 = DIRECTION ( 'NONE',  ( 0.000000000000000000, 1.000000000000000000, -0.000000000000000000 ) ) ;
#3679 = DIRECTION ( 'NONE',  ( 0.000000000000000000, 0.000000000000000000, 1.000000000000000000 ) ) ;
#3680 = VECTOR ( 'NONE', #49391, 999.9999999999998863 ) ;
#3681 = ORIENTED_EDGE ( 'NONE', *, *, #33800, .F. ) ;
#3682 = VECTOR ( 'NONE', #30122, 1000.000000000000000 ) ;
#3683 = EDGE_CURVE ( 'NONE', #26682, #51653, #46805, .T. ) ;
#3684 = CARTESIAN_POINT ( 'NONE',  ( 1.164038952974546293, 50.70432412269159528, -21.26556842862619234 ) ) ;
#3685 = AXIS2_PLACEMENT_3D ( 'NONE', #39846, #426, #43801 ) ;
#3686 = EDGE_CURVE ( 'NONE', #1781, #2708, #38422, .T. ) ;
#3687 = ORIENTED_EDGE ( 'NONE', *, *, #7290, .F. ) ;
#3688 = VERTEX_POINT ( 'NONE', #16803 ) ;
#3689 = VERTEX_POINT ( 'NONE', #32809 ) ;
#3690 = LINE ( 'NONE', #19718, #7417 ) ;
#3691 = ADVANCED_FACE ( 'NONE', ( #13097 ), #33066, .T. ) ;
#3693 = VERTEX_POINT ( 'NONE', #28853 ) ;
#3692 = VECTOR ( 'NONE', #36741, 999.9999999999998863 ) ;
#3694 = EDGE_CURVE ( 'NONE', #44232, #19435, #24140, .T. ) ;
#3695 = EDGE_CURVE ( 'NONE', #34352, #1095, #14921, .T. ) ;
#3696 = DIRECTION ( 'NONE',  ( 0.000000000000000000, 0.000000000000000000, 1.000000000000000000 ) ) ;
#3697 = DIRECTION ( 'NONE',  ( 0.000000000000000000, 0.000000000000000000, -1.000000000000000000 ) ) ;
#3700 = ORIENTED_EDGE ( 'NONE', *, *, #38529, .T. ) ;
#3699 = DIRECTION ( 'NONE',  ( 0.000000000000000000, -0.8229838658936596829, -0.5680647467311510379 ) ) ;
#3698 = FACE_OUTER_BOUND ( 'NONE', #20305, .T. ) ;
#3701 = ADVANCED_FACE ( 'NONE', ( #29637 ), #6253, .T. ) ;
#3702 = EDGE_CURVE ( 'NONE', #25229, #12202, #41772, .T. ) ;
#3703 = CARTESIAN_POINT ( 'NONE',  ( 47.53769253747992707, 28.00000000000000355, -45.94327833438006081 ) ) ;
#3704 = VERTEX_POINT ( 'NONE', #33845 ) ;
#3705 = CARTESIAN_POINT ( 'NONE',  ( -48.98765787015808115, -193.5000000000000000, 0.8610436117673582190 ) ) ;
#3706 = VERTEX_POINT ( 'NONE', #38038 ) ;
#3707 = DIRECTION ( 'NONE',  ( -0.000000000000000000, -0.9350162426854121689, 0.3546048870425426158 ) ) ;
#3708 = DIRECTION ( 'NONE',  ( 0.5338233779647826305, 0.000000000000000000, 0.8455960035018311727 ) ) ;
#3710 = DIRECTION ( 'NONE',  ( 0.000000000000000000, 0.000000000000000000, 1.000000000000000000 ) ) ;
#3709 = FACE_OUTER_BOUND ( 'NONE', #42289, .T. ) ;
#3711 = ORIENTED_EDGE ( 'NONE', *, *, #34319, .T. ) ;
#3712 = PLANE ( 'NONE',  #39068 ) ;
#3713 = CARTESIAN_POINT ( 'NONE',  ( -12.13476221271688615, -175.3837268820161057, 119.5996955107804638 ) ) ;
#3714 = CARTESIAN_POINT ( 'NONE',  ( 0.000000000000000000, 0.000000000000000000, 0.000000000000000000 ) ) ;
#3715 = ORIENTED_EDGE ( 'NONE', *, *, #33903, .F. ) ;
#3716 = LINE ( 'NONE', #23690, #24076 ) ;
#3717 = CARTESIAN_POINT ( 'NONE',  ( -336.3521761649654422, -81.08339623743702873, -41.09453333279329712 ) ) ;
#3718 = AXIS2_PLACEMENT_3D ( 'NONE', #6883, #50523, #22662 ) ;
#3719 = CARTESIAN_POINT ( 'NONE',  ( -41.90263914168912152, -189.7472609257535510, -124.8268793598473536 ) ) ;
#3720 = AXIS2_PLACEMENT_3D ( 'NONE', #6838, #22864, #30737 ) ;
#3721 = ORIENTED_EDGE ( 'NONE', *, *, #970, .T. ) ;
#3722 = LINE ( 'NONE', #47634, #21732 ) ;
#3724 = AXIS2_PLACEMENT_3D ( 'NONE', #33735, #41100, #24813 ) ;
#3723 = DIRECTION ( 'NONE',  ( -0.08879589532293158394, 0.000000000000000000, -0.9960498426152172291 ) ) ;
#3725 = ORIENTED_EDGE ( 'NONE', *, *, #47380, .F. ) ;
#3726 = PLANE ( 'NONE',  #21571 ) ;
#3727 = ORIENTED_EDGE ( 'NONE', *, *, #36804, .F. ) ;
#3728 = DIRECTION ( 'NONE',  ( 0.000000000000000000, -7.100801428331730794E-14, -1.000000000000000000 ) ) ;
#3729 = PLANE ( 'NONE',  #33747 ) ;
#3730 = DIRECTION ( 'NONE',  ( 0.000000000000000000, -0.000000000000000000, -1.000000000000000000 ) ) ;
#3731 = DIRECTION ( 'NONE',  ( -0.000000000000000000, 1.000000000000000000, -0.000000000000000000 ) ) ;
#3732 = CARTESIAN_POINT ( 'NONE',  ( -168.8371699641976420, -193.5000000000000000, 33.74820638215509661 ) ) ;
#3733 = CIRCLE ( 'NONE', #51577, 125.0000000000000000 ) ;
#3734 = DIRECTION ( 'NONE',  ( 0.000000000000000000, 1.000000000000000000, 0.000000000000000000 ) ) ;
#3735 = DIRECTION ( 'NONE',  ( 0.000000000000000000, 0.3546048870425300148, -0.9350162426854169428 ) ) ;
#3736 = CARTESIAN_POINT ( 'NONE',  ( -128.7986236165182561, -189.7472609257535510, 94.47107458416955694 ) ) ;
#3738 = ORIENTED_EDGE ( 'NONE', *, *, #17339, .F. ) ;
#3737 = DIRECTION ( 'NONE',  ( 0.000000000000000000, -1.000000000000000000, 0.000000000000000000 ) ) ;
#3739 = EDGE_CURVE ( 'NONE', #33568, #23872, #49883, .T. ) ;
#3740 = EDGE_LOOP ( 'NONE', ( #42913, #12181, #40442, #47807 ) ) ;
#3741 = EDGE_CURVE ( 'NONE', #48449, #15810, #25449, .T. ) ;
#3742 = EDGE_CURVE ( 'NONE', #45844, #6703, #45430, .T. ) ;
#3743 = CARTESIAN_POINT ( 'NONE',  ( 0.000000000000000000, -53.50000000000000000, -20.00000000000000000 ) ) ;
#3744 = ADVANCED_FACE ( 'NONE', ( #30166, #50409, #25703, #5994 ), #5230, .F. ) ;
#3745 = CARTESIAN_POINT ( 'NONE',  ( -339.1964088526558498, -103.0458197858324496, 55.34326076196052213 ) ) ;
#3746 = EDGE_LOOP ( 'NONE', ( #32481, #9702, #34359, #32484 ) ) ;
#3747 = VERTEX_POINT ( 'NONE', #41736 ) ;
#3748 = VECTOR ( 'NONE', #26090, 1000.000000000000000 ) ;
#3749 = ORIENTED_EDGE ( 'NONE', *, *, #43872, .T. ) ;
#3750 = FACE_OUTER_BOUND ( 'NONE', #23349, .T. ) ;
#3751 = PLANE ( 'NONE',  #37614 ) ;
#3752 = ADVANCED_FACE ( 'NONE', ( #13364 ), #21251, .T. ) ;
#3753 = VECTOR ( 'NONE', #41517, 999.9999999999998863 ) ;
#3754 = AXIS2_PLACEMENT_3D ( 'NONE', #27662, #51580, #11636 ) ;
#3755 = ADVANCED_FACE ( 'NONE', ( #38297 ), #41984, .T. ) ;
#3756 = LINE ( 'NONE', #19785, #16895 ) ;
#3757 = CARTESIAN_POINT ( 'NONE',  ( -332.3517673607765914, -85.59754891220836726, -45.24454186338619621 ) ) ;
#3758 = ORIENTED_EDGE ( 'NONE', *, *, #11765, .T. ) ;
#3759 = VERTEX_POINT ( 'NONE', #45958 ) ;
#3760 = CIRCLE ( 'NONE', #417, 125.0000000000000000 ) ;
#3761 = ADVANCED_FACE ( 'NONE', ( #37535 ), #5490, .F. ) ;
#3762 = ORIENTED_EDGE ( 'NONE', *, *, #47933, .F. ) ;
#3763 = FACE_OUTER_BOUND ( 'NONE', #33948, .T. ) ;
#3764 = LINE ( 'NONE', #15351, #11756 ) ;
#3765 = DIRECTION ( 'NONE',  ( 1.000000000000000000, -0.000000000000000000, 0.000000000000000000 ) ) ;
#3766 = EDGE_CURVE ( 'NONE', #44930, #38472, #30060, .T. ) ;
#3767 = AXIS2_PLACEMENT_3D ( 'NONE', #11777, #44892, #8883 ) ;
#3768 = CARTESIAN_POINT ( 'NONE',  ( -80.85382946868867293, -183.6283474603465606, 119.6996507684852702 ) ) ;
#3769 = CIRCLE ( 'NONE', #24782, 125.0000000000000000 ) ;
#3770 = DIRECTION ( 'NONE',  ( -0.000000000000000000, 0.000000000000000000, 1.000000000000000000 ) ) ;
#3771 = ORIENTED_EDGE ( 'NONE', *, *, #29189, .F. ) ;
#3772 = FACE_OUTER_BOUND ( 'NONE', #41187, .T. ) ;
#3773 = ADVANCED_FACE ( 'NONE', ( #34367 ), #46026, .T. ) ;
#3774 = PRODUCT_DEFINITION_CONTEXT ( 'detailed design', #13556, 'design' ) ;
#3775 = AXIS2_PLACEMENT_3D ( 'NONE', #37382, #48963, #33462 ) ;
#3776 = CARTESIAN_POINT ( 'NONE',  ( -332.3517673607765914, -64.73342574900661361, 5.491276508483657892 ) ) ;
#3777 = CARTESIAN_POINT ( 'NONE',  ( -305.0000000000000568, -78.25935320507912252, 39.41172259083855778 ) ) ;
#3778 = VERTEX_POINT ( 'NONE', #29899 ) ;
#3779 = EDGE_LOOP ( 'NONE', ( #28599, #10335, #2234, #9123 ) ) ;
#3780 = ORIENTED_EDGE ( 'NONE', *, *, #51858, .F. ) ;
#3781 = DIRECTION ( 'NONE',  ( 0.000000000000000000, 0.000000000000000000, -1.000000000000000000 ) ) ;
#3782 = DIRECTION ( 'NONE',  ( -0.000000000000000000, 0.9709418174260519008, -0.2393156642875582940 ) ) ;
#3783 = ORIENTED_EDGE ( 'NONE', *, *, #24230, .F. ) ;
#3784 = LINE ( 'NONE', #50857, #18185 ) ;
#3785 = DIRECTION ( 'NONE',  ( -0.000000000000000000, 0.000000000000000000, 1.000000000000000000 ) ) ;
#3786 = DIRECTION ( 'NONE',  ( 0.000000000000000000, -0.9927088740980548609, -0.1205366802553164696 ) ) ;
#3787 = VERTEX_POINT ( 'NONE', #13615 ) ;
#3788 = DIRECTION ( 'NONE',  ( -1.000000000000000000, -0.000000000000000000, 0.000000000000000000 ) ) ;
#3789 = ADVANCED_FACE ( 'NONE', ( #9945 ), #14152, .T. ) ;
#3790 = ORIENTED_EDGE ( 'NONE', *, *, #42697, .T. ) ;
#3791 = CARTESIAN_POINT ( 'NONE',  ( 41.00573479224733120, -193.5000000000000000, -87.27805883780175122 ) ) ;
#3792 = LINE ( 'NONE', #27450, #43895 ) ;
#3793 = FACE_BOUND ( 'NONE', #51894, .T. ) ;
#3794 = VECTOR ( 'NONE', #46599, 1000.000000000000000 ) ;
#3795 = CARTESIAN_POINT ( 'NONE',  ( -336.3521761649654422, -66.51961791625839737, 18.79457521708899392 ) ) ;
#3796 = EDGE_LOOP ( 'NONE', ( #30914, #37786, #31611, #20331 ) ) ;
#3797 = VECTOR ( 'NONE', #47550, 1000.000000000000000 ) ;
#3798 = AXIS2_PLACEMENT_3D ( 'NONE', #34752, #15073, #47642 ) ;
#3799 = CARTESIAN_POINT ( 'NONE',  ( -104.9497554727471851, -189.7472609257535510, -110.3950557015149059 ) ) ;
#3800 = DIRECTION ( 'NONE',  ( 0.000000000000000000, 1.000000000000000000, 0.000000000000000000 ) ) ;
#3801 = CARTESIAN_POINT ( 'NONE',  ( -48.47912675150885065, -188.5000000000000284, 6.938893903907228378E-15 ) ) ;
#3802 = LINE ( 'NONE', #114, #45082 ) ;
#3803 = CIRCLE ( 'NONE', #1292, 125.0000000000000000 ) ;
#3804 = ORIENTED_EDGE ( 'NONE', *, *, #20858, .F. ) ;
#3805 = DIRECTION ( 'NONE',  ( 0.9785564922995046988, 0.000000000000000000, -0.2059786187410953262 ) ) ;
#3806 = ORIENTED_EDGE ( 'NONE', *, *, #6979, .T. ) ;
#3807 = EDGE_CURVE ( 'NONE', #40896, #36109, #23352, .T. ) ;
#3808 = EDGE_LOOP ( 'NONE', ( #16865, #1142, #41787, #25674 ) ) ;
#3809 = AXIS2_PLACEMENT_3D ( 'NONE', #15432, #47479, #11463 ) ;
#3810 = LINE ( 'NONE', #31669, #46183 ) ;
#3812 = ORIENTED_EDGE ( 'NONE', *, *, #28375, .T. ) ;
#3811 = LINE ( 'NONE', #11172, #19423 ) ;
#3813 = AXIS2_PLACEMENT_3D ( 'NONE', #22588, #41779, #50196 ) ;
#3814 = EDGE_CURVE ( 'NONE', #32843, #16440, #7545, .T. ) ;
#3815 = EDGE_CURVE ( 'NONE', #30848, #16149, #10739, .T. ) ;
#3816 = ORIENTED_EDGE ( 'NONE', *, *, #6593, .F. ) ;
#3817 = EDGE_CURVE ( 'NONE', #38590, #27501, #47241, .T. ) ;
#3818 = DIRECTION ( 'NONE',  ( 0.000000000000000000, -0.9709418174260492362, 0.2393156642875685636 ) ) ;
#3819 = ADVANCED_FACE ( 'NONE', ( #3077 ), #11214, .T. ) ;
#3820 = VECTOR ( 'NONE', #31240, 1000.000000000000000 ) ;
#3821 = ADVANCED_FACE ( 'NONE', ( #10963 ), #22552, .F. ) ;
#3822 = VECTOR ( 'NONE', #15616, 1000.000000000000000 ) ;
#3823 = CARTESIAN_POINT ( 'NONE',  ( 56.77503207194100554, -189.7472609257535510, -67.42819922234311036 ) ) ;
#3824 = ORIENTED_EDGE ( 'NONE', *, *, #29102, .T. ) ;
#3825 = CARTESIAN_POINT ( 'NONE',  ( -34.51936650669028239, -193.5000000000000000, -124.2180546213278092 ) ) ;
#3826 = ADVANCED_FACE ( 'NONE', ( #27240 ), #39336, .F. ) ;
#3827 = CARTESIAN_POINT ( 'NONE',  ( -336.3521761649654422, -123.5000000000000284, 0.000000000000000000 ) ) ;
#3828 = ORIENTED_EDGE ( 'NONE', *, *, #10318, .F. ) ;
#3829 = DIRECTION ( 'NONE',  ( 0.000000000000000000, 1.000000000000000000, 0.000000000000000000 ) ) ;
#3830 = DIRECTION ( 'NONE',  ( -0.8896570909947467687, 0.000000000000000000, -0.4566292373937140270 ) ) ;
#3831 = EDGE_CURVE ( 'NONE', #30477, #33788, #6524, .T. ) ;
#3832 = CARTESIAN_POINT ( 'NONE',  ( -2.429962845726266397E-15, 20.00000000000000355, 0.000000000000000000 ) ) ;
#3833 = CYLINDRICAL_SURFACE ( 'NONE', #50092, 125.0000000000000000 ) ;
#3834 = ORIENTED_EDGE ( 'NONE', *, *, #35036, .F. ) ;
#3835 = EDGE_LOOP ( 'NONE', ( #49525, #43121, #26532, #32502 ) ) ;
#3836 = EDGE_CURVE ( 'NONE', #40857, #26725, #46717, .T. ) ;
#3837 = VERTEX_POINT ( 'NONE', #19120 ) ;
#3838 = DIRECTION ( 'NONE',  ( 0.000000000000000000, 1.000000000000000000, 0.000000000000000000 ) ) ;
#3839 = LINE ( 'NONE', #32206, #2504 ) ;
#3840 = AXIS2_PLACEMENT_3D ( 'NONE', #16280, #31799, #36491 ) ;
#3841 = ADVANCED_FACE ( 'NONE', ( #6775 ), #3590, .T. ) ;
#3842 = CARTESIAN_POINT ( 'NONE',  ( 75.95066919219054569, -175.3837268820161057, -11.92584929509534852 ) ) ;
#3843 = AXIS2_PLACEMENT_3D ( 'NONE', #29254, #10068, #21108 ) ;
#3844 = LINE ( 'NONE', #11451, #3481 ) ;
#3845 = DIRECTION ( 'NONE',  ( 0.000000000000000000, 1.000000000000000000, 0.000000000000000000 ) ) ;
#3846 = ORIENTED_EDGE ( 'NONE', *, *, #19059, .T. ) ;
#3847 = VECTOR ( 'NONE', #21598, 1000.000000000000000 ) ;
#3848 = EDGE_CURVE ( 'NONE', #794, #14931, #34610, .T. ) ;
#3849 = EDGE_CURVE ( 'NONE', #49882, #20620, #50223, .T. ) ;
#3850 = LINE ( 'NONE', #24090, #48414 ) ;
#3851 = ORIENTED_EDGE ( 'NONE', *, *, #8610, .F. ) ;
#3853 = ORIENTED_EDGE ( 'NONE', *, *, #33442, .T. ) ;
#3852 = CARTESIAN_POINT ( 'NONE',  ( -152.3176060415594861, -193.5000000000000000, -69.58857822034967455 ) ) ;
#3854 = VERTEX_POINT ( 'NONE', #46983 ) ;
#3855 = DIRECTION ( 'NONE',  ( 0.000000000000000000, 0.000000000000000000, -1.000000000000000000 ) ) ;
#3856 = AXIS2_PLACEMENT_3D ( 'NONE', #21699, #49302, #935 ) ;
#3857 = CARTESIAN_POINT ( 'NONE',  ( -339.1964088526558498, -79.00630452878473875, -38.74998146212148953 ) ) ;
#3858 = AXIS2_PLACEMENT_3D ( 'NONE', #27969, #15906, #43496 ) ;
#3859 = DIRECTION ( 'NONE',  ( 0.000000000000000000, 0.000000000000000000, 1.000000000000000000 ) ) ;
#3860 = CARTESIAN_POINT ( 'NONE',  ( -108.5723883981724640, -183.6283474603465606, 109.6074810615846076 ) ) ;
#3861 = ORIENTED_EDGE ( 'NONE', *, *, #27551, .F. ) ;
#3862 = CARTESIAN_POINT ( 'NONE',  ( 40.29886924377099433, 35.00000000000000000, -46.21030057994576623 ) ) ;
#3863 = VECTOR ( 'NONE', #4430, 1000.000000000000000 ) ;
#3864 = ORIENTED_EDGE ( 'NONE', *, *, #31105, .F. ) ;
#3865 = ADVANCED_FACE ( 'NONE', ( #26986 ), #26733, .T. ) ;
#3866 = AXIS2_PLACEMENT_3D ( 'NONE', #18798, #28583, #26398 ) ;
#3867 = ORIENTED_EDGE ( 'NONE', *, *, #25349, .T. ) ;
#3868 = LINE ( 'NONE', #31968, #7780 ) ;
#3869 = LINE ( 'NONE', #36422, #39936 ) ;
#3870 = CARTESIAN_POINT ( 'NONE',  ( -92.78132261338707565, -189.7472609257535510, -116.8859077982276773 ) ) ;
#3871 = CARTESIAN_POINT ( 'NONE',  ( 74.03660210627325000, -175.3837268820161057, -19.12855698118388048 ) ) ;
#3872 = CARTESIAN_POINT ( 'NONE',  ( 70.91428087927182844, -175.3837268820161057, -33.48461921608517855 ) ) ;
#3873 = ORIENTED_EDGE ( 'NONE', *, *, #38240, .T. ) ;
#3874 = PLANE ( 'NONE',  #10434 ) ;
#3875 = DIRECTION ( 'NONE',  ( 1.043714542225393697E-14, 0.3546048870425426158, 0.9350162426854121689 ) ) ;
#3876 = FACE_BOUND ( 'NONE', #49373, .T. ) ;
#3877 = VERTEX_POINT ( 'NONE', #2817 ) ;
#3878 = CIRCLE ( 'NONE', #18212, 125.0000000000000000 ) ;
#3879 = CIRCLE ( 'NONE', #34113, 60.00000000000000000 ) ;
#3880 = DIRECTION ( 'NONE',  ( 1.043714542225393381E-14, -0.9927088740980535286, 0.1205366802553268502 ) ) ;
#3881 = AXIS2_PLACEMENT_3D ( 'NONE', #35987, #23884, #31252 ) ;
#3882 = VECTOR ( 'NONE', #3670, 1000.000000000000000 ) ;
#3883 = CYLINDRICAL_SURFACE ( 'NONE', #28633, 4.999999999999997335 ) ;
#3884 = ADVANCED_FACE ( 'NONE', ( #18845 ), #19624, .F. ) ;
#3885 = VERTEX_POINT ( 'NONE', #14928 ) ;
#3886 = ADVANCED_FACE ( 'NONE', ( #15441 ), #31445, .T. ) ;
#3887 = CARTESIAN_POINT ( 'NONE',  ( -136.1415351158078408, -189.7472609257535510, -89.10837311819175000 ) ) ;
#3888 = VERTEX_POINT ( 'NONE', #46460 ) ;
#3889 = DIRECTION ( 'NONE',  ( 0.000000000000000000, 0.000000000000000000, -1.000000000000000000 ) ) ;
#3890 = FACE_BOUND ( 'NONE', #1247, .T. ) ;
#3891 = CIRCLE ( 'NONE', #24856, 60.00000000000000000 ) ;
#3893 = EDGE_LOOP ( 'NONE', ( #21888, #46622, #33513, #1785 ) ) ;
#3892 = DIRECTION ( 'NONE',  ( 0.000000000000000000, -0.000000000000000000, 1.000000000000000000 ) ) ;
#3894 = CIRCLE ( 'NONE', #19867, 4.999999999999997335 ) ;
#3895 = VECTOR ( 'NONE', #11796, 1000.000000000000000 ) ;
#3896 = AXIS2_PLACEMENT_3D ( 'NONE', #6064, #22081, #46022 ) ;
#3897 = FACE_OUTER_BOUND ( 'NONE', #9797, .T. ) ;
#3898 = ORIENTED_EDGE ( 'NONE', *, *, #36868, .T. ) ;
#3899 = ORIENTED_EDGE ( 'NONE', *, *, #18638, .F. ) ;
#3900 = CIRCLE ( 'NONE', #17352, 125.0000000000000000 ) ;
#3901 = DIRECTION ( 'NONE',  ( -0.000000000000000000, 1.000000000000000000, -0.000000000000000000 ) ) ;
#3902 = ORIENTED_EDGE ( 'NONE', *, *, #34227, .F. ) ;
#3903 = EDGE_CURVE ( 'NONE', #4422, #49846, #20395, .T. ) ;
#3904 = LINE ( 'NONE', #3630, #38504 ) ;
#3905 = DIRECTION ( 'NONE',  ( -0.9842305779475967187, 0.000000000000000000, -0.1768902751225733538 ) ) ;
#3906 = EDGE_CURVE ( 'NONE', #9933, #12964, #35083, .T. ) ;
#3907 = LINE ( 'NONE', #27556, #19184 ) ;
#3908 = DIRECTION ( 'NONE',  ( 0.9890401873221623674, 0.000000000000000000, 0.1476465640024917925 ) ) ;
#3909 = ORIENTED_EDGE ( 'NONE', *, *, #33659, .T. ) ;
#3912 = ORIENTED_EDGE ( 'NONE', *, *, #17738, .F. ) ;
#3911 = LINE ( 'NONE', #8370, #28936 ) ;
#3910 = LINE ( 'NONE', #35966, #19985 ) ;
#3913 = CIRCLE ( 'NONE', #23241, 60.00000000000000000 ) ;
#3914 = EDGE_LOOP ( 'NONE', ( #31853, #31954, #5133, #18373 ) ) ;
#3915 = AXIS2_PLACEMENT_3D ( 'NONE', #3732, #45000, #16098 ) ;
#3916 = DIRECTION ( 'NONE',  ( 0.9960498426152171181, 0.000000000000000000, -0.08879589532293157006 ) ) ;
#3917 = ORIENTED_EDGE ( 'NONE', *, *, #822, .F. ) ;
#3918 = PLANE ( 'NONE',  #28953 ) ;
#3919 = VERTEX_POINT ( 'NONE', #4129 ) ;
#3920 = CIRCLE ( 'NONE', #1403, 125.0000000000000000 ) ;
#3921 = DIRECTION ( 'NONE',  ( 0.000000000000000000, -1.000000000000000000, 0.000000000000000000 ) ) ;
#3922 = EDGE_LOOP ( 'NONE', ( #22340, #34109, #41447, #45541 ) ) ;
#3924 = DIRECTION ( 'NONE',  ( 0.000000000000000000, 3.469446951953614189E-15, -1.000000000000000000 ) ) ;
#3923 = DIRECTION ( 'NONE',  ( 0.000000000000000000, -0.8854560256532126861, -0.4647231720437631775 ) ) ;
#3925 = ORIENTED_EDGE ( 'NONE', *, *, #31055, .T. ) ;
#3926 = ORIENTED_EDGE ( 'NONE', *, *, #2947, .F. ) ;
#3927 = LINE ( 'NONE', #8384, #19475 ) ;
#3928 = VECTOR ( 'NONE', #36672, 1000.000000000000000 ) ;
#3929 = LINE ( 'NONE', #19182, #43301 ) ;
#3930 = AXIS2_PLACEMENT_3D ( 'NONE', #20465, #23629, #12584 ) ;
#3931 = CARTESIAN_POINT ( 'NONE',  ( 48.06131630543706734, -189.7472609257535510, -79.40367028273054473 ) ) ;
#3932 = CARTESIAN_POINT ( 'NONE',  ( -330.4913330509368166, -156.6043281241909995, 48.84008046109159551 ) ) ;
#3933 = LINE ( 'NONE', #11554, #34979 ) ;
#3934 = VECTOR ( 'NONE', #20581, 1000.000000000000000 ) ;
#3935 = VECTOR ( 'NONE', #12702, 1000.000000000000114 ) ;
#3936 = CARTESIAN_POINT ( 'NONE',  ( 0.000000000000000000, -63.50000000000000000, 0.000000000000000000 ) ) ;
#3937 = VERTEX_POINT ( 'NONE', #31965 ) ;
#3938 = DIRECTION ( 'NONE',  ( 0.7538481341944740510, 1.329199751808056281E-17, -0.6570486972603404308 ) ) ;
#3939 = CIRCLE ( 'NONE', #23224, 5.000000000000001776 ) ;
#3940 = CARTESIAN_POINT ( 'NONE',  ( 75.17589904515342880, -193.5000000000000000, -18.28755301364250130 ) ) ;
#3941 = DIRECTION ( 'NONE',  ( -1.000000000000000000, 0.000000000000000000, -0.000000000000000000 ) ) ;
#3942 = CIRCLE ( 'NONE', #21583, 60.00000000000000000 ) ;
#3943 = DIRECTION ( 'NONE',  ( 0.000000000000000000, 0.000000000000000000, -1.000000000000000000 ) ) ;
#3944 = ORIENTED_EDGE ( 'NONE', *, *, #46560, .F. ) ;
#3945 = PLANE ( 'NONE',  #30724 ) ;
#3946 = CARTESIAN_POINT ( 'NONE',  ( -117.8923552450418697, -193.5000000000000000, 102.7511748916629699 ) ) ;
#3947 = LINE ( 'NONE', #36501, #12339 ) ;
#3948 = ORIENTED_EDGE ( 'NONE', *, *, #47365, .T. ) ;
#3949 = EDGE_CURVE ( 'NONE', #41391, #40574, #51970, .T. ) ;
#3950 = ORIENTED_EDGE ( 'NONE', *, *, #13011, .T. ) ;
#3951 = EDGE_LOOP ( 'NONE', ( #7313, #36599, #49069, #20628 ) ) ;
#3952 = AXIS2_PLACEMENT_3D ( 'NONE', #33214, #44528, #648 ) ;
#3953 = CARTESIAN_POINT ( 'NONE',  ( 14.37129481273059106, -193.5000000000000000, -108.0501018472328241 ) ) ;
#3954 = CIRCLE ( 'NONE', #45083, 4.999999999999997335 ) ;
#3955 = CARTESIAN_POINT ( 'NONE',  ( -339.1964088526558498, -167.9936954712150339, 38.74998146212178796 ) ) ;
#3956 = DIRECTION ( 'NONE',  ( 0.000000000000000000, -0.000000000000000000, -1.000000000000000000 ) ) ;
#3957 = AXIS2_PLACEMENT_3D ( 'NONE', #27496, #39326, #47231 ) ;
#3958 = ORIENTED_EDGE ( 'NONE', *, *, #28314, .F. ) ;
#3959 = CARTESIAN_POINT ( 'NONE',  ( 0.5913660303101753168, 58.11612553618076760, -16.46795210274733279 ) ) ;
#3960 = ORIENTED_EDGE ( 'NONE', *, *, #41705, .F. ) ;
#3961 = ORIENTED_EDGE ( 'NONE', *, *, #21032, .F. ) ;
#3962 = VECTOR ( 'NONE', #17438, 1000.000000000000000 ) ;
#3963 = ORIENTED_EDGE ( 'NONE', *, *, #44529, .F. ) ;
#3964 = ADVANCED_FACE ( 'NONE', ( #8825 ), #28530, .F. ) ;
#3965 = DIRECTION ( 'NONE',  ( -0.000000000000000000, 1.000000000000000000, -0.000000000000000000 ) ) ;
#3966 = VECTOR ( 'NONE', #42362, 1000.000000000000227 ) ;
#3967 = VECTOR ( 'NONE', #19528, 1000.000000000000000 ) ;
#3968 = VERTEX_POINT ( 'NONE', #48543 ) ;
#3969 = AXIS2_PLACEMENT_3D ( 'NONE', #12831, #756, #4696 ) ;
#3970 = FACE_OUTER_BOUND ( 'NONE', #28921, .T. ) ;
#3971 = CARTESIAN_POINT ( 'NONE',  ( -47.49008656418669005, -193.5000000000000000, -0.1476465640024710591 ) ) ;
#3974 = VERTEX_POINT ( 'NONE', #15958 ) ;
#3973 = CARTESIAN_POINT ( 'NONE',  ( 40.29886924377099433, 35.00000000000000000, -46.21030057994576623 ) ) ;
#3972 = CARTESIAN_POINT ( 'NONE',  ( 61.38599058177057799, -193.5000000000000000, 59.62093586438192006 ) ) ;
#3975 = DIRECTION ( 'NONE',  ( -0.000000000000000000, 1.000000000000000000, -0.000000000000000000 ) ) ;
#3976 = VERTEX_POINT ( 'NONE', #36167 ) ;
#3977 = CARTESIAN_POINT ( 'NONE',  ( -15.81236726369125023, -177.1207230881787780, -120.6560517527615417 ) ) ;
#3978 = ORIENTED_EDGE ( 'NONE', *, *, #20019, .T. ) ;
#3979 = DIRECTION ( 'NONE',  ( 0.000000000000000000, 0.000000000000000000, 1.000000000000000000 ) ) ;
#3980 = EDGE_CURVE ( 'NONE', #26956, #24349, #40970, .T. ) ;
#3981 = FACE_OUTER_BOUND ( 'NONE', #22537, .T. ) ;
#3983 = CARTESIAN_POINT ( 'NONE',  ( 72.82672500347334221, -189.7472609257535510, 25.70779184431859221 ) ) ;
#3982 = LINE ( 'NONE', #49944, #44221 ) ;
#3984 = ORIENTED_EDGE ( 'NONE', *, *, #46384, .F. ) ;
#3985 = CARTESIAN_POINT ( 'NONE',  ( -60.00000000000000000, 20.00000000000000000, -60.00000000000000711 ) ) ;
#3986 = VECTOR ( 'NONE', #35379, 1000.000000000000000 ) ;
#3987 = DIRECTION ( 'NONE',  ( -0.000000000000000000, -1.000000000000000000, -0.000000000000000000 ) ) ;
#3988 = AXIS2_PLACEMENT_3D ( 'NONE', #46783, #19421, #3142 ) ;
#3989 = CARTESIAN_POINT ( 'NONE',  ( -48.47912675150885065, -177.1207230881787780, 6.938893903907228378E-15 ) ) ;
#3990 = EDGE_LOOP ( 'NONE', ( #1850, #328, #47951, #29352 ) ) ;
#3991 = LINE ( 'NONE', #8190, #4806 ) ;
#3992 = DIRECTION ( 'NONE',  ( 0.000000000000000000, 1.000000000000000000, -0.000000000000000000 ) ) ;
#3993 = AXIS2_PLACEMENT_3D ( 'NONE', #29672, #23539, #2351 ) ;
#3994 = DIRECTION ( 'NONE',  ( 0.000000000000000000, -0.000000000000000000, 1.000000000000000000 ) ) ;
#3995 = EDGE_CURVE ( 'NONE', #3221, #47296, #9097, .T. ) ;
#3996 = VERTEX_POINT ( 'NONE', #48788 ) ;
#3997 = DIRECTION ( 'NONE',  ( 0.000000000000000000, 1.000000000000000000, -0.000000000000000000 ) ) ;
#3998 = CARTESIAN_POINT ( 'NONE',  ( -339.1964088526558498, -172.3400804610910200, 33.10432812419180948 ) ) ;
#3999 = EDGE_CURVE ( 'NONE', #2485, #25619, #44327, .T. ) ;
#4000 = ORIENTED_EDGE ( 'NONE', *, *, #8294, .T. ) ;
#4001 = CARTESIAN_POINT ( 'NONE',  ( -330.4913330509368166, -64.50000000000000000, -0.4999999999999549249 ) ) ;
#4002 = ORIENTED_EDGE ( 'NONE', *, *, #29985, .T. ) ;
#4003 = VECTOR ( 'NONE', #22707, 1000.000000000000114 ) ;
#4004 = CARTESIAN_POINT ( 'NONE',  ( -332.3517673607765914, -123.5000000000000284, 0.000000000000000000 ) ) ;
#4005 = VECTOR ( 'NONE', #12619, 1000.000000000000000 ) ;
#4006 = CARTESIAN_POINT ( 'NONE',  ( 7.991501969728815880, -189.7472609257535510, 110.3950557015152611 ) ) ;
#4007 = VECTOR ( 'NONE', #22208, 1000.000000000000114 ) ;
#4008 = DIRECTION ( 'NONE',  ( 0.000000000000000000, 0.000000000000000000, -1.000000000000000000 ) ) ;
#4009 = DIRECTION ( 'NONE',  ( 0.000000000000000000, 0.000000000000000000, -1.000000000000000000 ) ) ;
#4010 = DIRECTION ( 'NONE',  ( 0.000000000000000000, 0.4647231720437573488, -0.8854560256532157947 ) ) ;
#4011 = EDGE_CURVE ( 'NONE', #19237, #2758, #11984, .T. ) ;
#4012 = AXIS2_PLACEMENT_3D ( 'NONE', #15781, #27822, #32560 ) ;
#4013 = EDGE_CURVE ( 'NONE', #19121, #23268, #161, .T. ) ;
#4015 = VECTOR ( 'NONE', #50518, 1000.000000000000000 ) ;
#4014 = DIRECTION ( 'NONE',  ( 0.000000000000000000, 0.000000000000000000, -1.000000000000000000 ) ) ;
#4016 = EDGE_CURVE ( 'NONE', #41557, #3584, #8058, .T. ) ;
#4017 = CYLINDRICAL_SURFACE ( 'NONE', #126, 125.0000000000000000 ) ;
#4018 = CARTESIAN_POINT ( 'NONE',  ( -124.1938582159088327, -193.5000000000000000, -99.45993886622791536 ) ) ;
#4020 = EDGE_LOOP ( 'NONE', ( #24596, #9949, #28125, #19542 ) ) ;
#4019 = CARTESIAN_POINT ( 'NONE',  ( -336.3521761649654422, -182.2665742509934148, -5.491276508484069119 ) ) ;
#4021 = ORIENTED_EDGE ( 'NONE', *, *, #2650, .F. ) ;
#4022 = CARTESIAN_POINT ( 'NONE',  ( -49.42645310536304493, -177.1207230881787780, 0.3202698538628349079 ) ) ;
#4023 = DIRECTION ( 'NONE',  ( -0.000000000000000000, 1.000000000000000000, -0.000000000000000000 ) ) ;
#4024 = ORIENTED_EDGE ( 'NONE', *, *, #40394, .F. ) ;
#4025 = VECTOR ( 'NONE', #38998, 1000.000000000000227 ) ;
#4026 = VECTOR ( 'NONE', #33269, 1000.000000000000000 ) ;
#4027 = EDGE_LOOP ( 'NONE', ( #37946, #446, #36105, #51740 ) ) ;
#4028 = ORIENTED_EDGE ( 'NONE', *, *, #1089, .T. ) ;
#4029 = ADVANCED_FACE ( 'NONE', ( #24597 ), #36954, .F. ) ;
#4030 = DIRECTION ( 'NONE',  ( 0.000000000000000000, -1.000000000000000000, 0.000000000000000000 ) ) ;
#4031 = LINE ( 'NONE', #23985, #10742 ) ;
#4032 = AXIS2_PLACEMENT_3D ( 'NONE', #15098, #35052, #26894 ) ;
#4033 = FACE_OUTER_BOUND ( 'NONE', #29892, .T. ) ;
#4034 = CARTESIAN_POINT ( 'NONE',  ( -330.4913330509368166, -151.3613951634091848, -52.00954392751743427 ) ) ;
#4035 = EDGE_LOOP ( 'NONE', ( #36750, #17969, #34335, #27032 ) ) ;
#4036 = VERTEX_POINT ( 'NONE', #35919 ) ;
#4037 = ORIENTED_EDGE ( 'NONE', *, *, #40112, .F. ) ;
#4038 = CARTESIAN_POINT ( 'NONE',  ( -336.3521761649654422, -104.1045282520827300, -55.74477592174792306 ) ) ;
#4039 = DIRECTION ( 'NONE',  ( -0.08879589532294572540, 0.000000000000000000, 0.9960498426152160079 ) ) ;
#4040 = VECTOR ( 'NONE', #41244, 1000.000000000000000 ) ;
#4041 = DIRECTION ( 'NONE',  ( 0.000000000000000000, 0.000000000000000000, 1.000000000000000000 ) ) ;
#4042 = DIRECTION ( 'NONE',  ( -1.000000000000000000, 0.000000000000000000, 0.000000000000000000 ) ) ;
#4043 = CARTESIAN_POINT ( 'NONE',  ( -339.1964088526558498, -151.8251501453687808, -52.89315522108996248 ) ) ;
#4044 = ORIENTED_EDGE ( 'NONE', *, *, #51658, .F. ) ;
#4045 = DIRECTION ( 'NONE',  ( -0.5586467658036535777, 0.000000000000000000, 0.8294056854502011022 ) ) ;
#4046 = DIRECTION ( 'NONE',  ( 0.000000000000000000, -1.000000000000000000, 0.000000000000000000 ) ) ;
#4047 = CARTESIAN_POINT ( 'NONE',  ( -339.1964088526558498, -183.4979166304964622, -0.4999999999999543698 ) ) ;
#4048 = LINE ( 'NONE', #35835, #19019 ) ;
#4049 = VECTOR ( 'NONE', #44692, 1000.000000000000000 ) ;
#4050 = ORIENTED_EDGE ( 'NONE', *, *, #33519, .F. ) ;
#4051 = VERTEX_POINT ( 'NONE', #44838 ) ;
#4052 = ORIENTED_EDGE ( 'NONE', *, *, #3467, .T. ) ;
#4053 = DIRECTION ( 'NONE',  ( 0.000000000000000000, 0.5680647467311656929, 0.8229838658936495799 ) ) ;
#4054 = LINE ( 'NONE', #23505, #4865 ) ;
#4055 = VERTEX_POINT ( 'NONE', #32222 ) ;
#4056 = CARTESIAN_POINT ( 'NONE',  ( -339.1964088526558498, -123.5000000000000284, 0.000000000000000000 ) ) ;
#4057 = DIRECTION ( 'NONE',  ( 0.000000000000000000, 0.000000000000000000, 1.000000000000000000 ) ) ;
#4058 = EDGE_CURVE ( 'NONE', #2027, #33969, #47760, .T. ) ;
#4059 = EDGE_CURVE ( 'NONE', #39414, #30881, #24346, .T. ) ;
#4060 = FACE_OUTER_BOUND ( 'NONE', #45746, .T. ) ;
#4061 = EDGE_LOOP ( 'NONE', ( #35971, #44863, #7815, #34052 ) ) ;
#4062 = DIRECTION ( 'NONE',  ( -0.000000000000000000, -1.000000000000000000, 0.000000000000000000 ) ) ;
#4063 = ORIENTED_EDGE ( 'NONE', *, *, #51076, .T. ) ;
#4064 = CARTESIAN_POINT ( 'NONE',  ( -339.1964088526558498, -151.3613951634092700, -52.00954392751739164 ) ) ;
#4065 = ORIENTED_EDGE ( 'NONE', *, *, #30121, .T. ) ;
#4066 = DIRECTION ( 'NONE',  ( -0.000000000000000000, 1.000000000000000000, -0.000000000000000000 ) ) ;
#4067 = FACE_BOUND ( 'NONE', #49442, .T. ) ;
#4068 = VECTOR ( 'NONE', #47425, 1000.000000000000000 ) ;
#4069 = AXIS2_PLACEMENT_3D ( 'NONE', #17936, #13996, #48249 ) ;
#4070 = DIRECTION ( 'NONE',  ( -0.6528221181905174975, 0.000000000000000000, -0.7575112421616236880 ) ) ;
#4071 = ORIENTED_EDGE ( 'NONE', *, *, #40206, .F. ) ;
#4072 = VECTOR ( 'NONE', #47339, 1000.000000000000000 ) ;
#4073 = FACE_OUTER_BOUND ( 'NONE', #29955, .T. ) ;
#4074 = DIRECTION ( 'NONE',  ( 0.000000000000000000, 1.000000000000000000, 0.000000000000000000 ) ) ;
#4075 = CARTESIAN_POINT ( 'NONE',  ( 46.31065297101394407, -183.6283474603465606, 79.94433946042836681 ) ) ;
#4076 = EDGE_CURVE ( 'NONE', #503, #28684, #12760, .T. ) ;
#4077 = CARTESIAN_POINT ( 'NONE',  ( -158.6498865914718124, -193.5000000000000000, 56.90809649257574421 ) ) ;
#4078 = EDGE_CURVE ( 'NONE', #11822, #17726, #24863, .T. ) ;
#4079 = ORIENTED_EDGE ( 'NONE', *, *, #24879, .T. ) ;
#4080 = CARTESIAN_POINT ( 'NONE',  ( 46.00000000000000711, 0.000000000000000000, -41.00000000000000000 ) ) ;
#4081 = ORIENTED_EDGE ( 'NONE', *, *, #19897, .F. ) ;
#4082 = VERTEX_POINT ( 'NONE', #415 ) ;
#4083 = VECTOR ( 'NONE', #35684, 1000.000000000000000 ) ;
#4084 = ADVANCED_FACE ( 'NONE', ( #697 ), #40882, .T. ) ;
#4085 = DIRECTION ( 'NONE',  ( 0.000000000000000000, 1.410908427127803051E-14, 1.000000000000000000 ) ) ;
#4087 = ORIENTED_EDGE ( 'NONE', *, *, #5082, .F. ) ;
#4086 = LINE ( 'NONE', #40573, #5192 ) ;
#4088 = ADVANCED_FACE ( 'NONE', ( #32997 ), #37466, .T. ) ;
#4089 = VERTEX_POINT ( 'NONE', #1473 ) ;
#4090 = DIRECTION ( 'NONE',  ( 0.000000000000000000, 0.000000000000000000, -1.000000000000000000 ) ) ;
#4091 = CIRCLE ( 'NONE', #1537, 125.0000000000000000 ) ;
#4092 = CARTESIAN_POINT ( 'NONE',  ( -332.3517673607765914, -72.48138011061176655, -29.74944317415788930 ) ) ;
#4093 = VERTEX_POINT ( 'NONE', #18023 ) ;
#4094 = DIRECTION ( 'NONE',  ( 0.000000000000000000, -0.5680647467311596976, -0.8229838658936536877 ) ) ;
#4095 = CARTESIAN_POINT ( 'NONE',  ( 52.98246549829695340, -175.3837268820161057, 73.01058346660533971 ) ) ;
#4096 = ORIENTED_EDGE ( 'NONE', *, *, #2705, .T. ) ;
#4097 = DIRECTION ( 'NONE',  ( -0.000000000000000000, 1.000000000000000000, -0.000000000000000000 ) ) ;
#4098 = CARTESIAN_POINT ( 'NONE',  ( 25.43954814678888710, -193.5000000000000000, 100.8019320314832754 ) ) ;
#4099 = CARTESIAN_POINT ( 'NONE',  ( -339.1964088526558498, -151.3613951634092700, -52.00954392751739164 ) ) ;
#4100 = CYLINDRICAL_SURFACE ( 'NONE', #13167, 15.24495751795539000 ) ;
#4101 = VERTEX_POINT ( 'NONE', #29576 ) ;
#4102 = EDGE_LOOP ( 'NONE', ( #26664, #13919, #30502, #51583 ) ) ;
#4103 = VERTEX_POINT ( 'NONE', #9106 ) ;
#4104 = DIRECTION ( 'NONE',  ( 0.000000000000000000, -0.000000000000000000, -1.000000000000000000 ) ) ;
#4105 = AXIS2_PLACEMENT_3D ( 'NONE', #51777, #35205, #3938 ) ;
#4106 = DIRECTION ( 'NONE',  ( 0.7175072570443348230, 0.000000000000000000, -0.6965510290629933765 ) ) ;
#4107 = VECTOR ( 'NONE', #16339, 1000.000000000000000 ) ;
#4108 = VECTOR ( 'NONE', #7835, 1000.000000000000114 ) ;
#4109 = DIRECTION ( 'NONE',  ( -0.000000000000000000, 1.000000000000000000, -0.000000000000000000 ) ) ;
#4110 = FACE_BOUND ( 'NONE', #36909, .T. ) ;
#4111 = DIRECTION ( 'NONE',  ( -0.000000000000000000, 0.5680647467311540355, -0.8229838658936575735 ) ) ;
#4112 = ORIENTED_EDGE ( 'NONE', *, *, #31050, .T. ) ;
#4113 = CIRCLE ( 'NONE', #39325, 125.0000000000000000 ) ;
#4114 = CARTESIAN_POINT ( 'NONE',  ( -48.47912675150885065, -189.7472609257535510, 6.938893903907228378E-15 ) ) ;
#4115 = EDGE_CURVE ( 'NONE', #28748, #46482, #22532, .T. ) ;
#4116 = VERTEX_POINT ( 'NONE', #13027 ) ;
#4118 = ORIENTED_EDGE ( 'NONE', *, *, #6032, .F. ) ;
#4117 = DIRECTION ( 'NONE',  ( -0.000000000000000000, 1.000000000000000000, 0.000000000000000000 ) ) ;
#4119 = AXIS2_PLACEMENT_3D ( 'NONE', #32780, #48825, #12794 ) ;
#4120 = ORIENTED_EDGE ( 'NONE', *, *, #16380, .T. ) ;
#4121 = DIRECTION ( 'NONE',  ( 0.8757349421956412971, 0.000000000000000000, -0.4827922027307366970 ) ) ;
#4122 = PLANE ( 'NONE',  #9860 ) ;
#4123 = EDGE_CURVE ( 'NONE', #46209, #20432, #41149, .T. ) ;
#4124 = DIRECTION ( 'NONE',  ( -1.000000000000000000, -0.000000000000000000, 0.000000000000000000 ) ) ;
#4125 = EDGE_CURVE ( 'NONE', #25351, #1446, #51867, .T. ) ;
#4126 = EDGE_CURVE ( 'NONE', #29121, #21483, #42624, .T. ) ;
#4127 = CARTESIAN_POINT ( 'NONE',  ( -48.47912675150885065, -189.7472609257535510, 6.938893903907228378E-15 ) ) ;
#4128 = EDGE_LOOP ( 'NONE', ( #13411, #34901, #51105, #15440 ) ) ;
#4129 = CARTESIAN_POINT ( 'NONE',  ( -330.4913330509368166, -181.8741440471348483, -13.87297036558341112 ) ) ;
#4130 = VERTEX_POINT ( 'NONE', #1726 ) ;
#4131 = EDGE_CURVE ( 'NONE', #40700, #7086, #13554, .T. ) ;
#4132 = AXIS2_PLACEMENT_3D ( 'NONE', #9612, #29833, #6464 ) ;
#4133 = EDGE_LOOP ( 'NONE', ( #40928, #699, #8104, #34171 ) ) ;
#4134 = CARTESIAN_POINT ( 'NONE',  ( -168.8371699641976420, -189.7472609257535510, 33.74820638215509661 ) ) ;
#4135 = EDGE_CURVE ( 'NONE', #9572, #12713, #45116, .T. ) ;
#4136 = DIRECTION ( 'NONE',  ( 1.000000000000000000, 8.654812430365571674E-17, -1.050884489711693973E-17 ) ) ;
#4137 = CARTESIAN_POINT ( 'NONE',  ( -164.3791542526839180, -175.3837268820161057, 46.82076062204521349 ) ) ;
#4138 = CARTESIAN_POINT ( 'NONE',  ( 53.56330073376472001, -175.3837268820161057, 72.19655804062048787 ) ) ;
#4139 = DIRECTION ( 'NONE',  ( -0.000000000000000000, 1.000000000000000000, -0.000000000000000000 ) ) ;
#4140 = EDGE_CURVE ( 'NONE', #44024, #33166, #5422, .T. ) ;
#4141 = VERTEX_POINT ( 'NONE', #49044 ) ;
#4142 = LINE ( 'NONE', #23837, #1128 ) ;
#4143 = PLANE ( 'NONE',  #7249 ) ;
#4144 = EDGE_CURVE ( 'NONE', #47580, #36397, #25388, .T. ) ;
#4145 = FACE_BOUND ( 'NONE', #15335, .T. ) ;
#4146 = VERTEX_POINT ( 'NONE', #21711 ) ;
#4147 = EDGE_CURVE ( 'NONE', #15921, #22734, #9361, .T. ) ;
#4148 = AXIS2_PLACEMENT_3D ( 'NONE', #38844, #43572, #3889 ) ;
#4149 = LINE ( 'NONE', #16226, #2117 ) ;
#4150 = VECTOR ( 'NONE', #32730, 1000.000000000000000 ) ;
#4151 = CARTESIAN_POINT ( 'NONE',  ( -332.3517673607765914, -93.75055682584159911, 51.01861988938794923 ) ) ;
#4152 = EDGE_CURVE ( 'NONE', #35261, #2420, #17522, .T. ) ;
#4153 = VERTEX_POINT ( 'NONE', #33783 ) ;
#4154 = FACE_OUTER_BOUND ( 'NONE', #11429, .T. ) ;
#4155 = VERTEX_POINT ( 'NONE', #29835 ) ;
#4156 = EDGE_CURVE ( 'NONE', #20290, #11975, #8220, .T. ) ;
#4157 = PLANE ( 'NONE',  #7515 ) ;
#4158 = FACE_BOUND ( 'NONE', #36801, .T. ) ;
#4160 = ORIENTED_EDGE ( 'NONE', *, *, #25675, .F. ) ;
#4159 = CARTESIAN_POINT ( 'NONE',  ( -330.4913330509368166, -178.4886558749184076, -21.38919645685194837 ) ) ;
#4161 = CARTESIAN_POINT ( 'NONE',  ( -330.4913330509368166, -180.6659093959934523, -14.60509510167853442 ) ) ;
#4162 = EDGE_CURVE ( 'NONE', #35348, #16442, #29266, .T. ) ;
#4163 = EDGE_LOOP ( 'NONE', ( #18885, #29308, #26466, #37742 ) ) ;
#4164 = AXIS2_PLACEMENT_3D ( 'NONE', #28924, #33420, #27957 ) ;
#4165 = ORIENTED_EDGE ( 'NONE', *, *, #25943, .T. ) ;
#4166 = CARTESIAN_POINT ( 'NONE',  ( -121.5885020763900997, -177.1207230881787780, -101.3904297239420913 ) ) ;
#4167 = VERTEX_POINT ( 'NONE', #5942 ) ;
#4168 = CARTESIAN_POINT ( 'NONE',  ( -336.3521761649654422, -155.6724726690323450, 49.48329383994676078 ) ) ;
#4169 = CARTESIAN_POINT ( 'NONE',  ( -336.3521761649654422, -153.2494431741581025, -51.01861988938816950 ) ) ;
#4170 = CARTESIAN_POINT ( 'NONE',  ( 0.000000000000000000, -150.9186671505818822, 52.24190551353965617 ) ) ;
#4171 = CARTESIAN_POINT ( 'NONE',  ( 64.72501964220592185, -189.7472609257535510, 53.00774697410174952 ) ) ;
#4172 = EDGE_LOOP ( 'NONE', ( #8707, #13728, #4050, #28756 ) ) ;
#4174 = VERTEX_POINT ( 'NONE', #42174 ) ;
#4173 = FACE_OUTER_BOUND ( 'NONE', #5086, .T. ) ;
#4175 = VERTEX_POINT ( 'NONE', #21956 ) ;
#4176 = VECTOR ( 'NONE', #28040, 1000.000000000000114 ) ;
#4177 = FACE_OUTER_BOUND ( 'NONE', #20003, .T. ) ;
#4178 = ORIENTED_EDGE ( 'NONE', *, *, #8611, .F. ) ;
#4179 = DIRECTION ( 'NONE',  ( 0.000000000000000000, -1.000000000000000000, -0.000000000000000000 ) ) ;
#4180 = VERTEX_POINT ( 'NONE', #37979 ) ;
#4181 = EDGE_CURVE ( 'NONE', #31384, #23160, #1983, .T. ) ;
#4182 = EDGE_CURVE ( 'NONE', #7899, #43082, #30102, .T. ) ;
#4183 = CARTESIAN_POINT ( 'NONE',  ( 56.77503207194101265, -193.5000000000000000, -67.42819922234311036 ) ) ;
#4184 = ORIENTED_EDGE ( 'NONE', *, *, #7927, .T. ) ;
#4186 = LINE ( 'NONE', #44115, #32528 ) ;
#4185 = DIRECTION ( 'NONE',  ( 0.000000000000000000, 0.000000000000000000, -1.000000000000000000 ) ) ;
#4187 = ADVANCED_FACE ( 'NONE', ( #10131 ), #26146, .F. ) ;
#4188 = EDGE_CURVE ( 'NONE', #23304, #17396, #31382, .T. ) ;
#4189 = ORIENTED_EDGE ( 'NONE', *, *, #3471, .T. ) ;
#4190 = FACE_OUTER_BOUND ( 'NONE', #38485, .T. ) ;
#4191 = DIRECTION ( 'NONE',  ( -0.000000000000000000, 1.000000000000000000, -0.000000000000000000 ) ) ;
#4192 = DIRECTION ( 'NONE',  ( 1.000000000000000000, 0.000000000000000000, 0.000000000000000000 ) ) ;
#4193 = DIRECTION ( 'NONE',  ( 1.000000000000000000, 0.000000000000000000, 0.000000000000000000 ) ) ;
#4194 = DIRECTION ( 'NONE',  ( 0.000000000000000000, -0.2393156642875547968, 0.9709418174260527890 ) ) ;
#4195 = PLANE ( 'NONE',  #35643 ) ;
#4196 = ORIENTED_EDGE ( 'NONE', *, *, #1190, .T. ) ;
#4197 = APPLICATION_PROTOCOL_DEFINITION ( 'draft international standard', 'automotive_design', 1998, #46486 ) ;
#4198 = CARTESIAN_POINT ( 'NONE',  ( -339.1964088526558498, -123.9999999999993747, 59.00000000000002132 ) ) ;
#4199 = CARTESIAN_POINT ( 'NONE',  ( -336.3521761649654422, -142.8954717479169574, 55.74477592174805096 ) ) ;
#4200 = CIRCLE ( 'NONE', #24331, 125.0000000000000000 ) ;
#4201 = AXIS2_PLACEMENT_3D ( 'NONE', #9570, #24820, #33994 ) ;
#4202 = CARTESIAN_POINT ( 'NONE',  ( 55.35935253854128746, -177.1207230881787780, 69.58857822035042773 ) ) ;
#4203 = VERTEX_POINT ( 'NONE', #2253 ) ;
#4204 = FACE_OUTER_BOUND ( 'NONE', #35289, .T. ) ;
#4205 = EDGE_CURVE ( 'NONE', #41934, #19363, #10382, .T. ) ;
#4206 = DIRECTION ( 'NONE',  ( -0.5085311186492094127, 0.000000000000000000, -0.8610436117673619938 ) ) ;
#4207 = LINE ( 'NONE', #32300, #3119 ) ;
#4208 = ORIENTED_EDGE ( 'NONE', *, *, #40350, .F. ) ;
#4209 = VERTEX_POINT ( 'NONE', #18790 ) ;
#4210 = ORIENTED_EDGE ( 'NONE', *, *, #18447, .T. ) ;
#4211 = EDGE_CURVE ( 'NONE', #17485, #20084, #3243, .T. ) ;
#4212 = PLANE ( 'NONE',  #19223 ) ;
#4213 = VECTOR ( 'NONE', #10804, 1000.000000000000114 ) ;
#4214 = CARTESIAN_POINT ( 'NONE',  ( -45.06671089634842531, -183.6283474603465606, -124.9534129907280686 ) ) ;
#4215 = DIRECTION ( 'NONE',  ( -0.000000000000000000, 1.000000000000000000, -0.000000000000000000 ) ) ;
#4216 = LINE ( 'NONE', #28626, #28711 ) ;
#4217 = ORIENTED_EDGE ( 'NONE', *, *, #38282, .T. ) ;
#4218 = CARTESIAN_POINT ( 'NONE',  ( 43.18784210722336780, -189.7472609257535510, -84.98333260264752198 ) ) ;
#4219 = VERTEX_POINT ( 'NONE', #14870 ) ;
#4220 = ORIENTED_EDGE ( 'NONE', *, *, #48097, .F. ) ;
#4221 = EDGE_LOOP ( 'NONE', ( #16679, #9617, #36250, #32450 ) ) ;
#4222 = PLANE ( 'NONE',  #8261 ) ;
#4223 = ADVANCED_FACE ( 'NONE', ( #30882 ), #6466, .T. ) ;
#4224 = VERTEX_POINT ( 'NONE', #3286 ) ;
#4225 = VECTOR ( 'NONE', #49225, 1000.000000000000114 ) ;
#4226 = CIRCLE ( 'NONE', #19352, 125.0000000000000000 ) ;
#4227 = LINE ( 'NONE', #24714, #24207 ) ;
#4228 = CARTESIAN_POINT ( 'NONE',  ( -170.0000000000000284, -123.5000000000000284, 41.63467731922665394 ) ) ;
#4231 = ORIENTED_EDGE ( 'NONE', *, *, #42962, .F. ) ;
#4230 = LINE ( 'NONE', #44437, #26660 ) ;
#4229 = CARTESIAN_POINT ( 'NONE',  ( 68.59638248015004081, -183.6283474603465606, -43.79868877201407429 ) ) ;
#4232 = DIRECTION ( 'NONE',  ( -0.1768902751225592818, 0.000000000000000000, -0.9842305779475992722 ) ) ;
#4233 = VERTEX_POINT ( 'NONE', #34548 ) ;
#4234 = DIRECTION ( 'NONE',  ( 0.5586467658036535777, 0.000000000000000000, -0.8294056854502011022 ) ) ;
#4235 = ORIENTED_EDGE ( 'NONE', *, *, #15568, .T. ) ;
#4236 = EDGE_CURVE ( 'NONE', #14358, #34438, #19058, .T. ) ;
#4238 = ADVANCED_FACE ( 'NONE', ( #23265 ), #50600, .T. ) ;
#4237 = CARTESIAN_POINT ( 'NONE',  ( 46.00000000000000711, -43.50000000000000000, -46.00000000000000000 ) ) ;
#4239 = CARTESIAN_POINT ( 'NONE',  ( 22.03849146056077757, -175.3837268820161057, 103.2098131075567409 ) ) ;
#4241 = DIRECTION ( 'NONE',  ( 0.000000000000000000, 0.000000000000000000, 1.000000000000000000 ) ) ;
#4240 = CARTESIAN_POINT ( 'NONE',  ( -336.3521761649654422, -107.7955183043589500, 56.89493493766750731 ) ) ;
#4242 = ORIENTED_EDGE ( 'NONE', *, *, #33719, .T. ) ;
#4243 = CARTESIAN_POINT ( 'NONE',  ( -170.2790847791494855, -177.1207230881787780, -28.10285082451570915 ) ) ;
#4244 = LINE ( 'NONE', #7662, #2675 ) ;
#4245 = AXIS2_PLACEMENT_3D ( 'NONE', #17795, #25672, #21740 ) ;
#4246 = VERTEX_POINT ( 'NONE', #10907 ) ;
#4247 = CARTESIAN_POINT ( 'NONE',  ( -160.2705093830644216, -183.6283474603465606, -55.92572546981520532 ) ) ;
#4248 = PLANE ( 'NONE',  #39140 ) ;
#4249 = CARTESIAN_POINT ( 'NONE',  ( 60.19403481868999961, -189.7472609257535510, -59.71720175837096178 ) ) ;
#4250 = ORIENTED_EDGE ( 'NONE', *, *, #5910, .T. ) ;
#4251 = DIRECTION ( 'NONE',  ( -0.000000000000000000, 0.000000000000000000, 1.000000000000000000 ) ) ;
#4252 = CARTESIAN_POINT ( 'NONE',  ( -339.1964088526558498, -108.6560878169904640, -58.13482838284724608 ) ) ;
#4253 = EDGE_LOOP ( 'NONE', ( #2783, #29583, #4518, #10762 ) ) ;
#4254 = LINE ( 'NONE', #24477, #11163 ) ;
#4255 = ORIENTED_EDGE ( 'NONE', *, *, #21099, .F. ) ;
#4256 = DIRECTION ( 'NONE',  ( -0.000000000000000000, 1.000000000000000000, -0.000000000000000000 ) ) ;
#4257 = CYLINDRICAL_SURFACE ( 'NONE', #15215, 124.9999999999999858 ) ;
#4258 = EDGE_CURVE ( 'NONE', #993, #30377, #22493, .T. ) ;
#4259 = AXIS2_PLACEMENT_3D ( 'NONE', #33486, #1933, #41604 ) ;
#4260 = CARTESIAN_POINT ( 'NONE',  ( -169.0136227435421006, -189.7472609257535510, -33.11246405730813080 ) ) ;
#4261 = DIRECTION ( 'NONE',  ( -0.000000000000000000, 1.000000000000000000, -0.000000000000000000 ) ) ;
#4262 = PLANE ( 'NONE',  #50931 ) ;
#4263 = EDGE_CURVE ( 'NONE', #5724, #16640, #38747, .T. ) ;
#4264 = CIRCLE ( 'NONE', #16881, 125.0000000000000000 ) ;
#4265 = CARTESIAN_POINT ( 'NONE',  ( -49.44376233341720450, -183.6283474603465606, -0.2635871660690713436 ) ) ;
#4266 = LINE ( 'NONE', #51579, #29502 ) ;
#4267 = LINE ( 'NONE', #36316, #24740 ) ;
#4269 = ORIENTED_EDGE ( 'NONE', *, *, #4188, .F. ) ;
#4268 = DIRECTION ( 'NONE',  ( 0.000000000000000000, -0.000000000000000000, -1.000000000000000000 ) ) ;
#4270 = DIRECTION ( 'NONE',  ( 0.000000000000000000, 1.000000000000000000, 0.000000000000000000 ) ) ;
#4271 = EDGE_CURVE ( 'NONE', #1934, #26319, #31786, .T. ) ;
#4272 = CARTESIAN_POINT ( 'NONE',  ( -157.1522883217072604, -193.5000000000000000, 59.71720175837172206 ) ) ;
#4273 = VERTEX_POINT ( 'NONE', #43213 ) ;
#4274 = ORIENTED_EDGE ( 'NONE', *, *, #29167, .T. ) ;
#4275 = VECTOR ( 'NONE', #14574, 1000.000000000000000 ) ;
#4276 = EDGE_LOOP ( 'NONE', ( #30527, #32688, #9706, #20593 ) ) ;
#4277 = DIRECTION ( 'NONE',  ( -0.7378332790417239107, 0.000000000000000000, -0.6749830015182142207 ) ) ;
#4278 = PLANE ( 'NONE',  #37027 ) ;
#4279 = CARTESIAN_POINT ( 'NONE',  ( -121.0298553105864556, -193.5000000000000000, -100.5610240384918939 ) ) ;
#4280 = ORIENTED_EDGE ( 'NONE', *, *, #32049, .F. ) ;
#4281 = ORIENTED_EDGE ( 'NONE', *, *, #43355, .F. ) ;
#4282 = ORIENTED_EDGE ( 'NONE', *, *, #3518, .F. ) ;
#4283 = EDGE_CURVE ( 'NONE', #49807, #47473, #42662, .T. ) ;
#4284 = CARTESIAN_POINT ( 'NONE',  ( -40.96347969518279086, -189.7472609257535510, -123.7720294769269174 ) ) ;
#4285 = DIRECTION ( 'NONE',  ( 0.000000000000000000, -0.000000000000000000, -1.000000000000000000 ) ) ;
#4287 = ORIENTED_EDGE ( 'NONE', *, *, #39827, .F. ) ;
#4286 = CARTESIAN_POINT ( 'NONE',  ( -339.1964088526558498, -183.0001959263613287, 7.728304129925186672 ) ) ;
#4288 = DIRECTION ( 'NONE',  ( -0.05924062789370748011, 0.000000000000000000, -0.9982437317643217956 ) ) ;
#4289 = CARTESIAN_POINT ( 'NONE',  ( -48.47912675150885065, -175.3837268820161057, 6.938893903907228378E-15 ) ) ;
#4290 = ORIENTED_EDGE ( 'NONE', *, *, #38831, .T. ) ;
#4291 = CARTESIAN_POINT ( 'NONE',  ( 67.66641500972446011, -189.7472609257535510, 46.20836643931067300 ) ) ;
#4292 = AXIS2_PLACEMENT_3D ( 'NONE', #5312, #21599, #1626 ) ;
#4293 = EDGE_CURVE ( 'NONE', #16129, #47736, #15852, .T. ) ;
#4294 = DIRECTION ( 'NONE',  ( -0.000000000000000000, 1.000000000000000000, -0.000000000000000000 ) ) ;
#4295 = EDGE_CURVE ( 'NONE', #49438, #12239, #42955, .T. ) ;
#4296 = DIRECTION ( 'NONE',  ( 0.000000000000000000, 0.000000000000000000, -1.000000000000000000 ) ) ;
#4297 = LINE ( 'NONE', #16133, #40837 ) ;
#4298 = AXIS2_PLACEMENT_3D ( 'NONE', #43565, #51211, #27263 ) ;
#4299 = ORIENTED_EDGE ( 'NONE', *, *, #11765, .F. ) ;
#4300 = ORIENTED_EDGE ( 'NONE', *, *, #25418, .T. ) ;
#4301 = ADVANCED_FACE ( 'NONE', ( #39279 ), #39003, .F. ) ;
#4302 = VERTEX_POINT ( 'NONE', #30351 ) ;
#4303 = CARTESIAN_POINT ( 'NONE',  ( 60.00000000000000000, -113.5000000000000142, 39.99999999999998579 ) ) ;
#4305 = VECTOR ( 'NONE', #35872, 1000.000000000000000 ) ;
#4304 = CARTESIAN_POINT ( 'NONE',  ( -49.46816693883101124, -177.1207230881787780, -0.1476465640024848536 ) ) ;
#4306 = ORIENTED_EDGE ( 'NONE', *, *, #48812, .F. ) ;
#4307 = FACE_OUTER_BOUND ( 'NONE', #5428, .T. ) ;
#4308 = DIRECTION ( 'NONE',  ( 0.000000000000000000, 1.000000000000000000, 0.000000000000000000 ) ) ;
#4309 = ORIENTED_EDGE ( 'NONE', *, *, #11179, .T. ) ;
#4310 = CARTESIAN_POINT ( 'NONE',  ( -135.6699833737243353, -193.5000000000000000, 89.56983042009326823 ) ) ;
#4311 = ORIENTED_EDGE ( 'NONE', *, *, #15775, .T. ) ;
#4312 = LINE ( 'NONE', #29263, #26578 ) ;
#4313 = VERTEX_POINT ( 'NONE', #51383 ) ;
#4314 = CARTESIAN_POINT ( 'NONE',  ( -33.52607327456453845, -175.3837268820161057, -124.1024020384603261 ) ) ;
#4315 = FACE_BOUND ( 'NONE', #34583, .T. ) ;
#4316 = VECTOR ( 'NONE', #40787, 1000.000000000000114 ) ;
#4317 = CARTESIAN_POINT ( 'NONE',  ( -238.7407812814481076, -193.5000000000000000, -41.45482488023466061 ) ) ;
#4318 = EDGE_CURVE ( 'NONE', #44107, #25533, #15374, .T. ) ;
#4319 = VERTEX_POINT ( 'NONE', #18287 ) ;
#4320 = CARTESIAN_POINT ( 'NONE',  ( -330.4913330509368166, -144.8891964568525452, -54.98865587491815177 ) ) ;
#4321 = DIRECTION ( 'NONE',  ( 0.000000000000000000, 0.000000000000000000, -1.000000000000000000 ) ) ;
#4322 = DIRECTION ( 'NONE',  ( 0.000000000000000000, 0.000000000000000000, 1.000000000000000000 ) ) ;
#4323 = CARTESIAN_POINT ( 'NONE',  ( -48.47912675150885065, -175.3837268820161057, 6.938893903907228378E-15 ) ) ;
#4324 = VERTEX_POINT ( 'NONE', #27446 ) ;
#4325 = DIRECTION ( 'NONE',  ( -0.1182731709213730997, 0.000000000000000000, 0.9929810960135161402 ) ) ;
#4326 = EDGE_LOOP ( 'NONE', ( #15229, #15017, #23343, #38726 ) ) ;
#4327 = ORIENTED_EDGE ( 'NONE', *, *, #7454, .F. ) ;
#4328 = LINE ( 'NONE', #20351, #23513 ) ;
#4330 = ORIENTED_EDGE ( 'NONE', *, *, #22980, .T. ) ;
#4329 = LINE ( 'NONE', #49270, #21945 ) ;
#4331 = AXIS2_PLACEMENT_3D ( 'NONE', #40308, #20097, #7750 ) ;
#4332 = EDGE_LOOP ( 'NONE', ( #33824, #856, #51355, #20098 ) ) ;
#4333 = CARTESIAN_POINT ( 'NONE',  ( -95.18697522258266019, -193.5000000000000000, 115.9455772817713353 ) ) ;
#4334 = VECTOR ( 'NONE', #36421, 1000.000000000000114 ) ;
#4335 = AXIS2_PLACEMENT_3D ( 'NONE', #28942, #8996, #25032 ) ;
#4336 = CARTESIAN_POINT ( 'NONE',  ( -339.1964088526558498, -162.2499814621216672, -44.49369547121515467 ) ) ;
#4337 = VERTEX_POINT ( 'NONE', #7492 ) ;
#4338 = DIRECTION ( 'NONE',  ( 0.000000000000000000, 0.000000000000000000, -1.000000000000000000 ) ) ;
#4339 = DIRECTION ( 'NONE',  ( 1.000000000000000000, 0.000000000000000000, -0.000000000000000000 ) ) ;
#4340 = ORIENTED_EDGE ( 'NONE', *, *, #33503, .T. ) ;
#4341 = DIRECTION ( 'NONE',  ( 1.000000000000000000, -0.000000000000000000, -0.000000000000000000 ) ) ;
#4342 = DIRECTION ( 'NONE',  ( 0.000000000000000000, -1.000000000000000000, -0.000000000000000000 ) ) ;
#4343 = EDGE_CURVE ( 'NONE', #23051, #42721, #23511, .T. ) ;
#4344 = ADVANCED_FACE ( 'NONE', ( #16680 ), #32685, .T. ) ;
#4345 = LINE ( 'NONE', #48515, #27752 ) ;
#4346 = CARTESIAN_POINT ( 'NONE',  ( -22.44626007086657182, -193.5000000000000000, 122.2591094863196730 ) ) ;
#4347 = VERTEX_POINT ( 'NONE', #31648 ) ;
#4348 = CIRCLE ( 'NONE', #33722, 125.0000000000000000 ) ;
#4349 = ORIENTED_EDGE ( 'NONE', *, *, #21738, .T. ) ;
#4350 = VERTEX_POINT ( 'NONE', #28725 ) ;
#4351 = LINE ( 'NONE', #47737, #18226 ) ;
#4352 = DIRECTION ( 'NONE',  ( -0.8124868780056742068, 0.000000000000000000, -0.5829794791144820021 ) ) ;
#4353 = CIRCLE ( 'NONE', #32853, 10.99999999999999645 ) ;
#4354 = CARTESIAN_POINT ( 'NONE',  ( -330.4913330509368166, -182.0095552316576573, -7.608018572112656308 ) ) ;
#4355 = FACE_BOUND ( 'NONE', #45889, .T. ) ;
#4356 = DIRECTION ( 'NONE',  ( -0.000000000000000000, 1.000000000000000000, -0.000000000000000000 ) ) ;
#4357 = ORIENTED_EDGE ( 'NONE', *, *, #26907, .T. ) ;
#4358 = EDGE_CURVE ( 'NONE', #15950, #4441, #47698, .T. ) ;
#4359 = EDGE_CURVE ( 'NONE', #46675, #35017, #19181, .T. ) ;
#4360 = VERTEX_POINT ( 'NONE', #44780 ) ;
#4362 = ORIENTED_EDGE ( 'NONE', *, *, #38670, .F. ) ;
#4361 = CARTESIAN_POINT ( 'NONE',  ( 61.38599058177057799, -189.7472609257535510, 59.62093586438192006 ) ) ;
#4363 = ORIENTED_EDGE ( 'NONE', *, *, #23692, .T. ) ;
#4364 = EDGE_CURVE ( 'NONE', #28891, #6751, #28388, .T. ) ;
#4365 = PLANE ( 'NONE',  #34189 ) ;
#4366 = LINE ( 'NONE', #20391, #29171 ) ;
#4367 = AXIS2_PLACEMENT_3D ( 'NONE', #35197, #34430, #11018 ) ;
#4368 = DIRECTION ( 'NONE',  ( 0.000000000000000000, -0.8229838658936516893, 0.5680647467311626952 ) ) ;
#4369 = DIRECTION ( 'NONE',  ( -1.000000000000000000, -0.000000000000000000, -0.000000000000000000 ) ) ;
#4370 = ORIENTED_EDGE ( 'NONE', *, *, #4499, .F. ) ;
#4371 = DIRECTION ( 'NONE',  ( -0.000000000000000000, 0.3546048870425463906, 0.9350162426854107256 ) ) ;
#4372 = VECTOR ( 'NONE', #3232, 1000.000000000000227 ) ;
#4373 = VERTEX_POINT ( 'NONE', #39525 ) ;
#4374 = AXIS2_PLACEMENT_3D ( 'NONE', #5002, #41231, #12340 ) ;
#4375 = ORIENTED_EDGE ( 'NONE', *, *, #28128, .T. ) ;
#4376 = CARTESIAN_POINT ( 'NONE',  ( -62.32061382540517513, -193.5000000000000000, 123.2250735253144285 ) ) ;
#4377 = LINE ( 'NONE', #33006, #40397 ) ;
#4378 = DIRECTION ( 'NONE',  ( 0.000000000000000000, -1.000000000000000000, -0.000000000000000000 ) ) ;
#4379 = DIRECTION ( 'NONE',  ( 1.000000000000000000, 0.000000000000000000, 0.000000000000000000 ) ) ;
#4380 = DIRECTION ( 'NONE',  ( -0.000000000000000000, 1.000000000000000000, -0.000000000000000000 ) ) ;
#4381 = CARTESIAN_POINT ( 'NONE',  ( -305.0000000000000568, -123.9999999999999147, -59.99791663049643375 ) ) ;
#4382 = ORIENTED_EDGE ( 'NONE', *, *, #3186, .F. ) ;
#4383 = CARTESIAN_POINT ( 'NONE',  ( -83.89965873179625078, -175.3837268820161057, 118.8334608768482354 ) ) ;
#4384 = LINE ( 'NONE', #41161, #21512 ) ;
#4385 = VECTOR ( 'NONE', #9772, 1000.000000000000000 ) ;
#4386 = AXIS2_PLACEMENT_3D ( 'NONE', #7790, #30934, #19117 ) ;
#4387 = CARTESIAN_POINT ( 'NONE',  ( -339.1964088526558498, -168.0775241366794717, 40.16023333901038228 ) ) ;
#4388 = FACE_BOUND ( 'NONE', #15368, .T. ) ;
#4389 = ORIENTED_EDGE ( 'NONE', *, *, #37153, .F. ) ;
#4390 = AXIS2_PLACEMENT_3D ( 'NONE', #34627, #2578, #42782 ) ;
#4391 = VECTOR ( 'NONE', #43968, 1000.000000000000000 ) ;
#4392 = DIRECTION ( 'NONE',  ( -0.000000000000000000, 0.6631226582407937498, -0.7485107481711024136 ) ) ;
#4393 = PLANE ( 'NONE',  #39546 ) ;
#4394 = EDGE_LOOP ( 'NONE', ( #11410, #25988, #2714, #17981 ) ) ;
#4395 = CARTESIAN_POINT ( 'NONE',  ( -150.1390659022305840, -175.3837268820161057, 72.73415134496005408 ) ) ;
#4396 = VERTEX_POINT ( 'NONE', #355 ) ;
#4397 = CARTESIAN_POINT ( 'NONE',  ( -305.0000000000000568, -181.8741440471347630, -13.87297036558366692 ) ) ;
#4398 = FACE_BOUND ( 'NONE', #31223, .T. ) ;
#4400 = ORIENTED_EDGE ( 'NONE', *, *, #49706, .T. ) ;
#4399 = PLANE ( 'NONE',  #39663 ) ;
#4401 = VECTOR ( 'NONE', #12046, 1000.000000000000114 ) ;
#4402 = EDGE_CURVE ( 'NONE', #12957, #38011, #44515, .T. ) ;
#4403 = EDGE_CURVE ( 'NONE', #6831, #15659, #4570, .T. ) ;
#4404 = ADVANCED_FACE ( 'NONE', ( #44262 ), #11679, .F. ) ;
#4405 = DIRECTION ( 'NONE',  ( -0.000000000000000000, -1.000000000000000000, -0.000000000000000000 ) ) ;
#4406 = ORIENTED_EDGE ( 'NONE', *, *, #43041, .T. ) ;
#4407 = ADVANCED_FACE ( 'NONE', ( #43992 ), #31905, .T. ) ;
#4408 = VECTOR ( 'NONE', #25531, 1000.000000000000000 ) ;
#4409 = ORIENTED_EDGE ( 'NONE', *, *, #16364, .F. ) ;
#4410 = CARTESIAN_POINT ( 'NONE',  ( -126.8597349762179931, -177.1207230881787780, -96.08646119223956816 ) ) ;
#4411 = ORIENTED_EDGE ( 'NONE', *, *, #1619, .T. ) ;
#4412 = EDGE_CURVE ( 'NONE', #15918, #28294, #35851, .T. ) ;
#4413 = DIRECTION ( 'NONE',  ( -0.000000000000000000, 1.000000000000000000, -0.000000000000000000 ) ) ;
#4414 = EDGE_CURVE ( 'NONE', #28503, #18767, #48724, .T. ) ;
#4415 = DIRECTION ( 'NONE',  ( 0.000000000000000000, -1.000000000000000000, 0.000000000000000000 ) ) ;
#4416 = ADVANCED_FACE ( 'NONE', ( #16407 ), #39772, .F. ) ;
#4417 = VECTOR ( 'NONE', #13847, 1000.000000000000000 ) ;
#4418 = VECTOR ( 'NONE', #25132, 1000.000000000000000 ) ;
#4419 = EDGE_CURVE ( 'NONE', #49836, #2507, #12698, .T. ) ;
#4420 = FACE_OUTER_BOUND ( 'NONE', #20953, .T. ) ;
#4421 = EDGE_CURVE ( 'NONE', #26319, #38573, #101, .T. ) ;
#4422 = VERTEX_POINT ( 'NONE', #24023 ) ;
#4425 = ORIENTED_EDGE ( 'NONE', *, *, #50692, .T. ) ;
#4424 = CARTESIAN_POINT ( 'NONE',  ( -330.4913330509368166, -162.2499814621210419, 44.49369547121568758 ) ) ;
#4423 = CARTESIAN_POINT ( 'NONE',  ( -339.1964088526558498, -162.9984922102927385, -43.83057281297435992 ) ) ;
#4426 = VECTOR ( 'NONE', #13631, 1000.000000000000227 ) ;
#4427 = VECTOR ( 'NONE', #10079, 1000.000000000000000 ) ;
#4428 = ORIENTED_EDGE ( 'NONE', *, *, #47132, .T. ) ;
#4429 = EDGE_CURVE ( 'NONE', #32690, #1606, #40037, .T. ) ;
#4430 = DIRECTION ( 'NONE',  ( -0.000000000000000000, 1.000000000000000000, -0.000000000000000000 ) ) ;
#4431 = ORIENTED_EDGE ( 'NONE', *, *, #23553, .F. ) ;
#4432 = CARTESIAN_POINT ( 'NONE',  ( 74.49773146996551532, -177.1207230881787780, -22.39848972532283256 ) ) ;
#4433 = VERTEX_POINT ( 'NONE', #20081 ) ;
#4434 = ADVANCED_FACE ( 'NONE', ( #36106 ), #16148, .F. ) ;
#4435 = LINE ( 'NONE', #473, #44798 ) ;
#4436 = AXIS2_PLACEMENT_3D ( 'NONE', #27266, #23079, #39090 ) ;
#4437 = DIRECTION ( 'NONE',  ( -0.000000000000000000, 1.000000000000000000, -0.000000000000000000 ) ) ;
#4438 = VERTEX_POINT ( 'NONE', #24537 ) ;
#4440 = LINE ( 'NONE', #20457, #25005 ) ;
#4439 = LINE ( 'NONE', #44114, #37558 ) ;
#4441 = VERTEX_POINT ( 'NONE', #5626 ) ;
#4442 = ORIENTED_EDGE ( 'NONE', *, *, #20036, .F. ) ;
#4443 = CARTESIAN_POINT ( 'NONE',  ( -332.3517673607765914, -129.1091364105427317, 59.73723787327234191 ) ) ;
#4444 = CARTESIAN_POINT ( 'NONE',  ( -49.17567778057185990, -189.7472609257535510, 0.7175072570443320474 ) ) ;
#4445 = DIRECTION ( 'NONE',  ( 0.000000000000000000, 0.000000000000000000, 1.000000000000000000 ) ) ;
#4446 = DIRECTION ( 'NONE',  ( -1.000000000000000000, -0.000000000000000000, 0.000000000000000000 ) ) ;
#4447 = CARTESIAN_POINT ( 'NONE',  ( -153.7332855749581881, -189.7472609257535510, 67.42819922234392038 ) ) ;
#4448 = AXIS2_PLACEMENT_3D ( 'NONE', #41669, #2759, #13822 ) ;
#4449 = FACE_OUTER_BOUND ( 'NONE', #50031, .T. ) ;
#4450 = SHAPE_DEFINITION_REPRESENTATION ( #50801, #40181 ) ;
#4451 = LINE ( 'NONE', #11623, #39596 ) ;
#4452 = DIRECTION ( 'NONE',  ( 0.000000000000000000, 0.3546048870425363986, 0.9350162426854146114 ) ) ;
#4453 = EDGE_CURVE ( 'NONE', #30289, #36857, #49765, .T. ) ;
#4454 = LINE ( 'NONE', #44408, #25664 ) ;
#4455 = AXIS2_PLACEMENT_3D ( 'NONE', #23479, #35292, #34515 ) ;
#4456 = CARTESIAN_POINT ( 'NONE',  ( -336.3521761649654422, -93.75055682584159911, 51.01861988938794923 ) ) ;
#4457 = VERTEX_POINT ( 'NONE', #9299 ) ;
#4458 = PLANE ( 'NONE',  #25670 ) ;
#4459 = CARTESIAN_POINT ( 'NONE',  ( -48.47912675150885065, -177.1207230881787780, 6.938893903907228378E-15 ) ) ;
#4460 = CARTESIAN_POINT ( 'NONE',  ( -49.40581635894069024, -193.5000000000000000, 0.3758275821142362250 ) ) ;
#4461 = ORIENTED_EDGE ( 'NONE', *, *, #32429, .T. ) ;
#4462 = ORIENTED_EDGE ( 'NONE', *, *, #40585, .F. ) ;
#4463 = AXIS2_PLACEMENT_3D ( 'NONE', #8652, #40436, #4989 ) ;
#4464 = ORIENTED_EDGE ( 'NONE', *, *, #49929, .F. ) ;
#4465 = VECTOR ( 'NONE', #38777, 1000.000000000000227 ) ;
#4466 = ADVANCED_FACE ( 'NONE', ( #40816 ), #37400, .T. ) ;
#4467 = CARTESIAN_POINT ( 'NONE',  ( -14.28570516517293676, -193.5000000000000000, 120.2323164553486663 ) ) ;
#4468 = AXIS2_PLACEMENT_3D ( 'NONE', #59, #48159, #7934 ) ;
#4469 = CARTESIAN_POINT ( 'NONE',  ( -134.9506378406916554, -189.7472609257535510, 90.26448786734091811 ) ) ;
#4470 = DIRECTION ( 'NONE',  ( 0.8455960035018272869, 0.000000000000000000, -0.5338233779647886257 ) ) ;
#4471 = FACE_OUTER_BOUND ( 'NONE', #42996, .T. ) ;
#4472 = VERTEX_POINT ( 'NONE', #30041 ) ;
#4473 = EDGE_CURVE ( 'NONE', #14259, #19641, #9042, .T. ) ;
#4474 = EDGE_CURVE ( 'NONE', #26506, #46675, #25841, .T. ) ;
#4475 = FACE_OUTER_BOUND ( 'NONE', #11489, .T. ) ;
#4476 = EDGE_CURVE ( 'NONE', #29838, #9298, #37669, .T. ) ;
#4477 = CIRCLE ( 'NONE', #19586, 20.00000000000001776 ) ;
#4478 = CARTESIAN_POINT ( 'NONE',  ( 68.79964045138288498, -183.6283474603465606, 43.25148278810711844 ) ) ;
#4479 = ADVANCED_FACE ( 'NONE', ( #5885 ), #4846, .F. ) ;
#4480 = DIRECTION ( 'NONE',  ( -0.4566292373937018145, 0.000000000000000000, -0.8896570909947529859 ) ) ;
#4481 = ORIENTED_EDGE ( 'NONE', *, *, #2986, .F. ) ;
#4482 = EDGE_LOOP ( 'NONE', ( #15533, #11596, #13300, #16661 ) ) ;
#4483 = ADVANCED_FACE ( 'NONE', ( #5102 ), #32932, .F. ) ;
#4484 = CYLINDRICAL_SURFACE ( 'NONE', #20837, 124.9999999999999858 ) ;
#4485 = VECTOR ( 'NONE', #13696, 1000.000000000000000 ) ;
#4486 = EDGE_CURVE ( 'NONE', #24719, #7018, #21114, .T. ) ;
#4487 = CIRCLE ( 'NONE', #3652, 125.0000000000000000 ) ;
#4488 = LINE ( 'NONE', #27619, #7412 ) ;
#4489 = CARTESIAN_POINT ( 'NONE',  ( -47.74129347246713451, -189.7472609257535510, 0.6749830015182212151 ) ) ;
#4492 = EDGE_LOOP ( 'NONE', ( #22196, #39135, #9926, #37270 ) ) ;
#4491 = CARTESIAN_POINT ( 'NONE',  ( -102.5006284722404502, -177.1207230881787780, -112.7238987608084386 ) ) ;
#4490 = FACE_OUTER_BOUND ( 'NONE', #25109, .T. ) ;
#4493 = EDGE_CURVE ( 'NONE', #18044, #33603, #41596, .T. ) ;
#4494 = CARTESIAN_POINT ( 'NONE',  ( 74.00867759460086859, -175.3837268820161057, 24.93467037017222410 ) ) ;
#4495 = ORIENTED_EDGE ( 'NONE', *, *, #20183, .F. ) ;
#4496 = FACE_OUTER_BOUND ( 'NONE', #12150, .T. ) ;
#4497 = CARTESIAN_POINT ( 'NONE',  ( 49.88781503343062695, -193.5000000000000000, -75.49882471933871386 ) ) ;
#4498 = ORIENTED_EDGE ( 'NONE', *, *, #37863, .T. ) ;
#4499 = EDGE_CURVE ( 'NONE', #15154, #22921, #1923, .T. ) ;
#4500 = FACE_OUTER_BOUND ( 'NONE', #42787, .T. ) ;
#4501 = FACE_OUTER_BOUND ( 'NONE', #20780, .T. ) ;
#4503 = FACE_OUTER_BOUND ( 'NONE', #39069, .T. ) ;
#4502 = DIRECTION ( 'NONE',  ( -0.3482016354343866471, 0.000000000000000000, -0.9374196611341253371 ) ) ;
#4504 = VECTOR ( 'NONE', #9541, 1000.000000000000000 ) ;
#4505 = ORIENTED_EDGE ( 'NONE', *, *, #46571, .F. ) ;
#4506 = EDGE_CURVE ( 'NONE', #26366, #37592, #10776, .T. ) ;
#4507 = CARTESIAN_POINT ( 'NONE',  ( -8.721998590732194856, -177.1207230881787780, -118.5089480183145270 ) ) ;
#4508 = AXIS2_PLACEMENT_3D ( 'NONE', #50657, #14651, #34861 ) ;
#4509 = CARTESIAN_POINT ( 'NONE',  ( 45.36094686508022988, -183.6283474603465606, -82.57748230379237953 ) ) ;
#4510 =( NAMED_UNIT ( * ) PLANE_ANGLE_UNIT ( ) SI_UNIT ( $, .RADIAN. ) );
#4511 = EDGE_LOOP ( 'NONE', ( #44369, #16068, #13485, #31467 ) ) ;
#4512 = DIRECTION ( 'NONE',  ( 0.000000000000000000, -0.000000000000000000, 1.000000000000000000 ) ) ;
#4513 = CARTESIAN_POINT ( 'NONE',  ( 59.80284513346456521, -183.6283474603465606, 62.45009659481583952 ) ) ;
#4514 = VERTEX_POINT ( 'NONE', #1133 ) ;
#4515 = LINE ( 'NONE', #558, #44397 ) ;
#4516 = CARTESIAN_POINT ( 'NONE',  ( -47.74129347246712740, -175.3837268820161057, -0.6749830015182022303 ) ) ;
#4517 = ADVANCED_FACE ( 'NONE', ( #33721 ), #13756, .T. ) ;
#4518 = ORIENTED_EDGE ( 'NONE', *, *, #28497, .T. ) ;
#4519 = CARTESIAN_POINT ( 'NONE',  ( -168.6933499419502880, -183.6283474603465606, 30.40954281680879845 ) ) ;
#4520 = ORIENTED_EDGE ( 'NONE', *, *, #26121, .T. ) ;
#4521 = DIRECTION ( 'NONE',  ( -0.000000000000000000, -0.8229838658936516893, 0.5680647467311626952 ) ) ;
#4522 = CARTESIAN_POINT ( 'NONE',  ( 67.66641500972444589, -175.3837268820161057, 46.20836643931066590 ) ) ;
#4523 = VECTOR ( 'NONE', #15969, 1000.000000000000227 ) ;
#4524 = DIRECTION ( 'NONE',  ( 0.000000000000000000, -0.000000000000000000, 1.000000000000000000 ) ) ;
#4525 = DIRECTION ( 'NONE',  ( -0.000000000000000000, 1.000000000000000000, -0.000000000000000000 ) ) ;
#4526 = DIRECTION ( 'NONE',  ( -0.000000000000000000, -0.5680647467311485954, 0.8229838658936613482 ) ) ;
#4527 = AXIS2_PLACEMENT_3D ( 'NONE', #31728, #48012, #32231 ) ;
#4528 = CARTESIAN_POINT ( 'NONE',  ( -336.3521761649654422, -82.40546666720629787, 42.41660376256258047 ) ) ;
#4529 = DIRECTION ( 'NONE',  ( -0.000000000000000000, -0.5680647467311485954, 0.8229838658936613482 ) ) ;
#4530 = DIRECTION ( 'NONE',  ( 0.000000000000000000, 0.7485107481710977506, -0.6631226582407989678 ) ) ;
#4532 = ORIENTED_EDGE ( 'NONE', *, *, #7051, .T. ) ;
#4531 = CARTESIAN_POINT ( 'NONE',  ( -336.3521761649654422, -160.6539403396202772, 45.90766452162722544 ) ) ;
#4533 = ORIENTED_EDGE ( 'NONE', *, *, #35436, .F. ) ;
#4534 = EDGE_CURVE ( 'NONE', #45319, #37719, #41870, .T. ) ;
#4535 = ADVANCED_FACE ( 'NONE', ( #49247, #33974, #879, #13242, #21376, #16922, #25323, #50023, #29260, #5359, #24801, #1405, #17460, #6900, #38168, #31321, #22676, #2179, #26089, #42117, #35266, #6141, #39216, #6395, #42379, #43153, #18221, #3225, #42893, #34492, #38688, #26351, #2448, #10328, #38943, #22422, #51316, #34243, #38441, #2952, #26861, #19259, #46341, #22158, #26612, #2692, #7158, #35015, #18991, #42646, #46862, #47111 ), #23198, .T. ) ;
#4536 = DIRECTION ( 'NONE',  ( 0.000000000000000000, -1.000000000000000000, -0.000000000000000000 ) ) ;
#4537 = DIRECTION ( 'NONE',  ( 0.000000000000000000, 0.000000000000000000, 1.000000000000000000 ) ) ;
#4538 = ORIENTED_EDGE ( 'NONE', *, *, #15846, .F. ) ;
#4539 = VERTEX_POINT ( 'NONE', #10074 ) ;
#4540 = ORIENTED_EDGE ( 'NONE', *, *, #27541, .F. ) ;
#4541 = CARTESIAN_POINT ( 'NONE',  ( 70.49476099643867144, -177.1207230881787780, 34.94873081740416865 ) ) ;
#4542 = PLANE ( 'NONE',  #35367 ) ;
#4543 = CARTESIAN_POINT ( 'NONE',  ( -336.3521761649654422, -105.0395444947681369, -56.09938080879045685 ) ) ;
#4544 = ORIENTED_EDGE ( 'NONE', *, *, #47788, .T. ) ;
#4545 = ORIENTED_EDGE ( 'NONE', *, *, #37759, .T. ) ;
#4546 = DIRECTION ( 'NONE',  ( 0.6965510290629982615, 0.000000000000000000, -0.7175072570443298270 ) ) ;
#4547 = CARTESIAN_POINT ( 'NONE',  ( -332.3517673607765914, -107.7955183043589500, 56.89493493766750731 ) ) ;
#4549 = ORIENTED_EDGE ( 'NONE', *, *, #4125, .F. ) ;
#4548 = LINE ( 'NONE', #4822, #47602 ) ;
#4550 = EDGE_CURVE ( 'NONE', #51567, #49394, #18474, .T. ) ;
#4551 = DIRECTION ( 'NONE',  ( 0.9890401873221644768, 0.000000000000000000, -0.1476465640024779702 ) ) ;
#4552 = CARTESIAN_POINT ( 'NONE',  ( -95.18697522258271704, -183.6283474603465606, 115.9455772817713211 ) ) ;
#4553 = AXIS2_PLACEMENT_3D ( 'NONE', #4827, #25304, #37906 ) ;
#4554 = ORIENTED_EDGE ( 'NONE', *, *, #36426, .F. ) ;
#4555 = DIRECTION ( 'NONE',  ( -0.6528221181905280446, 0.000000000000000000, 0.7575112421616145841 ) ) ;
#4556 = AXIS2_PLACEMENT_3D ( 'NONE', #49890, #38819, #46725 ) ;
#4557 = CARTESIAN_POINT ( 'NONE',  ( -173.1763543514842070, -183.6283474603465606, 8.694908215728892387 ) ) ;
#4558 = DIRECTION ( 'NONE',  ( 0.9027978299657446470, 0.000000000000000000, -0.4300652022765183435 ) ) ;
#4559 = DIRECTION ( 'NONE',  ( 0.000000000000000000, 2.937465085987393136E-14, 1.000000000000000000 ) ) ;
#4560 = VECTOR ( 'NONE', #2706, 1000.000000000000000 ) ;
#4561 = EDGE_CURVE ( 'NONE', #9866, #10499, #44362, .T. ) ;
#4562 = VERTEX_POINT ( 'NONE', #51074 ) ;
#4563 = ORIENTED_EDGE ( 'NONE', *, *, #33251, .T. ) ;
#4564 = DIRECTION ( 'NONE',  ( 0.000000000000000000, -1.000000000000000000, 0.000000000000000000 ) ) ;
#4565 = CARTESIAN_POINT ( 'NONE',  ( -170.0000000000000284, -113.5000000000000142, -60.00000000000001421 ) ) ;
#4566 = ORIENTED_EDGE ( 'NONE', *, *, #35933, .T. ) ;
#4567 = DIRECTION ( 'NONE',  ( 0.000000000000000000, 0.000000000000000000, -1.000000000000000000 ) ) ;
#4568 = CARTESIAN_POINT ( 'NONE',  ( 2.066935079424583765, -175.3837268820161057, -114.3245189510257802 ) ) ;
#4569 = ORIENTED_EDGE ( 'NONE', *, *, #31332, .F. ) ;
#4570 = LINE ( 'NONE', #19563, #48567 ) ;
#4571 = VECTOR ( 'NONE', #929, 1000.000000000000114 ) ;
#4572 = CARTESIAN_POINT ( 'NONE',  ( 60.00000000000001421, 0.000000000000000000, 60.00000000000000711 ) ) ;
#4573 = ORIENTED_EDGE ( 'NONE', *, *, #32378, .F. ) ;
#4574 = LINE ( 'NONE', #48729, #43361 ) ;
#4575 = ORIENTED_EDGE ( 'NONE', *, *, #1732, .F. ) ;
#4576 = CARTESIAN_POINT ( 'NONE',  ( -172.4422607493951318, -193.5000000000000000, 16.06677968424543579 ) ) ;
#4577 = EDGE_LOOP ( 'NONE', ( #13481, #12977, #4037, #45093 ) ) ;
#4578 = SHAPE_REPRESENTATION ( 'MAS-325', ( #4934, #35983, #26752, #5778, #13328, #15851, #4105, #33483, #14173, #46920, #18366, #51091 ), #51945 ) ;
#4579 = CYLINDRICAL_SURFACE ( 'NONE', #29880, 125.0000000000000000 ) ;
#4580 = DIRECTION ( 'NONE',  ( -0.9027978299657416494, 0.000000000000000000, -0.4300652022765245608 ) ) ;
#4581 = LINE ( 'NONE', #24548, #3083 ) ;
#4582 = DIRECTION ( 'NONE',  ( 0.000000000000000000, -0.7485107481711024136, -0.6631226582407937498 ) ) ;
#4583 = ORIENTED_EDGE ( 'NONE', *, *, #2249, .T. ) ;
#4584 = DIRECTION ( 'NONE',  ( -0.000000000000000000, -1.000000000000000000, 0.000000000000000000 ) ) ;
#4585 = ORIENTED_EDGE ( 'NONE', *, *, #5919, .T. ) ;
#4586 = ORIENTED_EDGE ( 'NONE', *, *, #26085, .F. ) ;
#4587 = CARTESIAN_POINT ( 'NONE',  ( -56.05401443572781517, -189.7472609257535510, 124.7702732086913073 ) ) ;
#4589 = EDGE_LOOP ( 'NONE', ( #20479, #13086, #51843, #40986 ) ) ;
#4588 = DIRECTION ( 'NONE',  ( 9.613575272659281827E-18, 0.4304733388468033328, -0.9026032930042329205 ) ) ;
#4590 = CIRCLE ( 'NONE', #33952, 125.0000000000000000 ) ;
#4591 = VECTOR ( 'NONE', #1016, 1000.000000000000000 ) ;
#4592 = ORIENTED_EDGE ( 'NONE', *, *, #10571, .T. ) ;
#4593 = DIRECTION ( 'NONE',  ( -0.000000000000000000, -1.000000000000000000, 0.000000000000000000 ) ) ;
#4594 = EDGE_CURVE ( 'NONE', #32153, #3411, #16686, .T. ) ;
#4595 = VECTOR ( 'NONE', #46478, 1000.000000000000000 ) ;
#4596 = LINE ( 'NONE', #21926, #6966 ) ;
#4597 = CARTESIAN_POINT ( 'NONE',  ( -339.1964088526558498, -172.3400804610915600, -33.10432812419107051 ) ) ;
#4598 = ORIENTED_EDGE ( 'NONE', *, *, #2892, .F. ) ;
#4599 = DIRECTION ( 'NONE',  ( -0.8858462335218260097, 0.000000000000000000, 0.4639789333096864810 ) ) ;
#4600 = VECTOR ( 'NONE', #34095, 1000.000000000000114 ) ;
#4601 = ORIENTED_EDGE ( 'NONE', *, *, #26721, .T. ) ;
#4602 = LINE ( 'NONE', #20907, #1489 ) ;
#4603 = CARTESIAN_POINT ( 'NONE',  ( 8.879953965148887463, -193.5000000000000000, 109.9360785596608849 ) ) ;
#4605 = VECTOR ( 'NONE', #50778, 1000.000000000000000 ) ;
#4604 = DIRECTION ( 'NONE',  ( -0.000000000000000000, -0.6631226582407885317, 0.7485107481711069655 ) ) ;
#4606 = DIRECTION ( 'NONE',  ( 0.000000000000000000, 0.000000000000000000, -1.000000000000000000 ) ) ;
#4607 = EDGE_LOOP ( 'NONE', ( #39024, #8177, #27221, #7287 ) ) ;
#4608 = ORIENTED_EDGE ( 'NONE', *, *, #18532, .F. ) ;
#4609 = ORIENTED_EDGE ( 'NONE', *, *, #926, .T. ) ;
#4610 = DIRECTION ( 'NONE',  ( 0.000000000000000000, 0.000000000000000000, -1.000000000000000000 ) ) ;
#4611 = CARTESIAN_POINT ( 'NONE',  ( -164.0008810331606810, -175.3837268820161057, 47.74645837849822527 ) ) ;
#4612 = EDGE_CURVE ( 'NONE', #1159, #16305, #30546, .T. ) ;
#4613 = FACE_BOUND ( 'NONE', #18387, .T. ) ;
#4614 = FACE_BOUND ( 'NONE', #41051, .T. ) ;
#4615 = CARTESIAN_POINT ( 'NONE',  ( -44.48323084606168720, -177.1207230881787780, 124.9361149384469769 ) ) ;
#4616 = EDGE_LOOP ( 'NONE', ( #6012, #2106, #35546, #45814 ) ) ;
#4617 = EDGE_LOOP ( 'NONE', ( #13248, #5203, #688, #36367 ) ) ;
#4619 = ORIENTED_EDGE ( 'NONE', *, *, #50811, .F. ) ;
#4618 = DIRECTION ( 'NONE',  ( -0.000000000000000000, -0.7485107481711046340, -0.6631226582407911962 ) ) ;
#4620 = FACE_OUTER_BOUND ( 'NONE', #7190, .T. ) ;
#4621 = ORIENTED_EDGE ( 'NONE', *, *, #23988, .T. ) ;
#4622 = AXIS2_PLACEMENT_3D ( 'NONE', #51448, #24802, #28469 ) ;
#4623 = CARTESIAN_POINT ( 'NONE',  ( -339.1964088526558498, -68.51134412508183402, -21.38919645685240312 ) ) ;
#4624 = LINE ( 'NONE', #16739, #41748 ) ;
#4625 = AXIS2_PLACEMENT_3D ( 'NONE', #12304, #39889, #27808 ) ;
#4626 = AXIS2_PLACEMENT_3D ( 'NONE', #22164, #46350, #2186 ) ;
#4627 = CARTESIAN_POINT ( 'NONE',  ( -305.0000000000000568, -155.3847370087607374, 50.82679948493869659 ) ) ;
#4628 = DIRECTION ( 'NONE',  ( -0.000000000000000000, 1.000000000000000000, -0.000000000000000000 ) ) ;
#4629 = ORIENTED_EDGE ( 'NONE', *, *, #30401, .T. ) ;
#4630 = CARTESIAN_POINT ( 'NONE',  ( 59.00260725618640123, -193.5000000000000000, -63.81752780152988436 ) ) ;
#4631 = VERTEX_POINT ( 'NONE', #15064 ) ;
#4632 = VECTOR ( 'NONE', #44351, 999.9999999999998863 ) ;
#4633 = VERTEX_POINT ( 'NONE', #6657 ) ;
#4634 = CARTESIAN_POINT ( 'NONE',  ( -332.3517673607765914, -179.5993808087905279, -18.46045550523168899 ) ) ;
#4635 = VECTOR ( 'NONE', #23816, 1000.000000000000000 ) ;
#4636 = FACE_OUTER_BOUND ( 'NONE', #47867, .T. ) ;
#4637 = CARTESIAN_POINT ( 'NONE',  ( 66.03142248012325410, -193.5000000000000000, 50.12318939044039467 ) ) ;
#4638 = AXIS2_PLACEMENT_3D ( 'NONE', #49799, #33507, #41372 ) ;
#4639 = LINE ( 'NONE', #16478, #7950 ) ;
#4640 = EDGE_CURVE ( 'NONE', #2552, #31987, #31067, .T. ) ;
#4641 = CARTESIAN_POINT ( 'NONE',  ( -123.6678354051270361, -189.7472609257535510, 99.85818990449065780 ) ) ;
#4642 = DIRECTION ( 'NONE',  ( -0.000000000000000000, -0.2393156642875516049, 0.9709418174260534551 ) ) ;
#4643 = VERTEX_POINT ( 'NONE', #30816 ) ;
#4644 = VECTOR ( 'NONE', #42288, 1000.000000000000000 ) ;
#4645 = CARTESIAN_POINT ( 'NONE',  ( -339.1964088526558498, -180.9052250602809977, -13.63415328425247885 ) ) ;
#4646 = DIRECTION ( 'NONE',  ( -0.000000000000000000, 0.7485107481710934207, -0.6631226582408039638 ) ) ;
#4647 = ADVANCED_FACE ( 'NONE', ( #10847 ), #51563, .T. ) ;
#4649 = VECTOR ( 'NONE', #10999, 1000.000000000000000 ) ;
#4648 = LINE ( 'NONE', #32764, #33705 ) ;
#4650 = FACE_BOUND ( 'NONE', #14053, .T. ) ;
#4651 = VERTEX_POINT ( 'NONE', #32352 ) ;
#4652 = DIRECTION ( 'NONE',  ( 0.1182731709213592358, 0.000000000000000000, 0.9929810960135178055 ) ) ;
#4653 = ORIENTED_EDGE ( 'NONE', *, *, #18778, .T. ) ;
#4654 = CARTESIAN_POINT ( 'NONE',  ( -12.13476221271687194, -175.3837268820161057, 119.5996955107804780 ) ) ;
#4655 = VERTEX_POINT ( 'NONE', #47367 ) ;
#4656 = CARTESIAN_POINT ( 'NONE',  ( 26.52087324849106054, -173.5000000000000284, -70.00000000000002842 ) ) ;
#4657 = EDGE_CURVE ( 'NONE', #4167, #4175, #43675, .T. ) ;
#4658 = ORIENTED_EDGE ( 'NONE', *, *, #24720, .T. ) ;
#4659 = EDGE_CURVE ( 'NONE', #36146, #24293, #3722, .T. ) ;
#4660 = DIRECTION ( 'NONE',  ( 0.000000000000000000, 1.000000000000000000, -0.000000000000000000 ) ) ;
#4661 = ADVANCED_FACE ( 'NONE', ( #39463 ), #27647, .F. ) ;
#4662 = AXIS2_PLACEMENT_3D ( 'NONE', #15567, #15839, #16088 ) ;
#4663 = DIRECTION ( 'NONE',  ( -1.000000000000000000, 0.000000000000000000, 0.000000000000000000 ) ) ;
#4665 = ORIENTED_EDGE ( 'NONE', *, *, #21636, .T. ) ;
#4664 = LINE ( 'NONE', #20692, #16209 ) ;
#4666 = AXIS2_PLACEMENT_3D ( 'NONE', #1916, #13748, #50018 ) ;
#4667 = VECTOR ( 'NONE', #41285, 1000.000000000000000 ) ;
#4668 = CARTESIAN_POINT ( 'NONE',  ( 37.29583330861160562, -193.5000000000000000, -89.54698061029594669 ) ) ;
#4669 = ORIENTED_EDGE ( 'NONE', *, *, #10521, .T. ) ;
#4670 = ORIENTED_EDGE ( 'NONE', *, *, #10541, .F. ) ;
#4671 = LINE ( 'NONE', #20702, #43538 ) ;
#4672 = DIRECTION ( 'NONE',  ( 0.6068001458185890984, 0.000000000000000000, 0.7948544414133565938 ) ) ;
#4673 = ORIENTED_EDGE ( 'NONE', *, *, #48285, .T. ) ;
#4674 = AXIS2_PLACEMENT_3D ( 'NONE', #28400, #49174, #8434 ) ;
#4675 = ADVANCED_FACE ( 'NONE', ( #47888 ), #23954, .T. ) ;
#4676 = LINE ( 'NONE', #20437, #51135 ) ;
#4677 = AXIS2_PLACEMENT_3D ( 'NONE', #5702, #16753, #40892 ) ;
#4678 = CARTESIAN_POINT ( 'NONE',  ( -336.3521761649654422, -64.73342574900661361, 5.491276508483657892 ) ) ;
#4679 = CARTESIAN_POINT ( 'NONE',  ( -48.47912675150885065, -177.1207230881787780, 6.938893903907228378E-15 ) ) ;
#4680 = AXIS2_PLACEMENT_3D ( 'NONE', #998, #48056, #8886 ) ;
#4681 = VECTOR ( 'NONE', #33708, 1000.000000000000114 ) ;
#4682 = CARTESIAN_POINT ( 'NONE',  ( -330.4913330509368166, -179.7763290203206452, 20.80804632820240840 ) ) ;
#4683 = CARTESIAN_POINT ( 'NONE',  ( -67.22356632362119910, -183.6283474603465606, -123.5865930638409793 ) ) ;
#4684 = ORIENTED_EDGE ( 'NONE', *, *, #49713, .F. ) ;
#4687 = ORIENTED_EDGE ( 'NONE', *, *, #30225, .T. ) ;
#4686 = CARTESIAN_POINT ( 'NONE',  ( -339.1964088526558498, -143.9541802141663709, 55.34326076196097688 ) ) ;
#4685 = DIRECTION ( 'NONE',  ( -0.6749830015182091136, 0.000000000000000000, -0.7378332790417285736 ) ) ;
#4688 = ORIENTED_EDGE ( 'NONE', *, *, #24709, .T. ) ;
#4689 = PLANE ( 'NONE',  #26504 ) ;
#4690 = VERTEX_POINT ( 'NONE', #7673 ) ;
#4691 = DIRECTION ( 'NONE',  ( 0.000000000000000000, -0.9709418174260492362, 0.2393156642875685636 ) ) ;
#4692 = ORIENTED_EDGE ( 'NONE', *, *, #26584, .F. ) ;
#4693 = FACE_BOUND ( 'NONE', #20510, .T. ) ;
#4694 = CARTESIAN_POINT ( 'NONE',  ( -47.87232660569026166, -189.7472609257535510, 0.7948544414133635883 ) ) ;
#4695 = VERTEX_POINT ( 'NONE', #46 ) ;
#4697 = DIRECTION ( 'NONE',  ( 1.000000000000000000, -0.000000000000000000, 0.000000000000000000 ) ) ;
#4696 = DIRECTION ( 'NONE',  ( 0.000000000000000000, -9.251858538542971828E-16, 1.000000000000000000 ) ) ;
#4698 = ORIENTED_EDGE ( 'NONE', *, *, #33940, .T. ) ;
#4699 = ORIENTED_EDGE ( 'NONE', *, *, #29231, .T. ) ;
#4700 = LINE ( 'NONE', #29123, #19513 ) ;
#4701 = AXIS2_PLACEMENT_3D ( 'NONE', #33605, #29137, #45199 ) ;
#4702 = LINE ( 'NONE', #24414, #23895 ) ;
#4703 = CARTESIAN_POINT ( 'NONE',  ( -339.1964088526558498, -64.50000000000000000, -0.5000000000000457412 ) ) ;
#4704 = DIRECTION ( 'NONE',  ( 0.000000000000000000, -1.000000000000000000, 0.000000000000000000 ) ) ;
#4705 = ORIENTED_EDGE ( 'NONE', *, *, #45842, .F. ) ;
#4706 = AXIS2_PLACEMENT_3D ( 'NONE', #39392, #48334, #3400 ) ;
#4707 = LINE ( 'NONE', #25204, #27232 ) ;
#4708 = VECTOR ( 'NONE', #28360, 1000.000000000000227 ) ;
#4709 = EDGE_CURVE ( 'NONE', #31272, #15810, #3464, .T. ) ;
#4710 = EDGE_CURVE ( 'NONE', #8813, #19788, #42704, .T. ) ;
#4711 = SHAPE_DEFINITION_REPRESENTATION ( #21821, #24080 ) ;
#4712 = PLANE ( 'NONE',  #25368 ) ;
#4713 = DIRECTION ( 'NONE',  ( 0.000000000000000000, 1.000000000000000000, -0.000000000000000000 ) ) ;
#4714 = CARTESIAN_POINT ( 'NONE',  ( -60.86541030502398542, -183.6283474603465606, -124.3848060646151623 ) ) ;
#4715 = FACE_OUTER_BOUND ( 'NONE', #30165, .T. ) ;
#4716 = ORIENTED_EDGE ( 'NONE', *, *, #47844, .F. ) ;
#4717 = VERTEX_POINT ( 'NONE', #36298 ) ;
#4718 = DIRECTION ( 'NONE',  ( 0.000000000000000000, 0.000000000000000000, -1.000000000000000000 ) ) ;
#4719 = CIRCLE ( 'NONE', #34085, 125.0000000000000000 ) ;
#4720 = VECTOR ( 'NONE', #364, 1000.000000000000000 ) ;
#4721 = LINE ( 'NONE', #16563, #47899 ) ;
#4722 = PLANE ( 'NONE',  #25324 ) ;
#4723 = ORIENTED_EDGE ( 'NONE', *, *, #47073, .T. ) ;
#4724 = ORIENTED_EDGE ( 'NONE', *, *, #6680, .F. ) ;
#4725 = EDGE_CURVE ( 'NONE', #32204, #25437, #15027, .T. ) ;
#4726 = CIRCLE ( 'NONE', #46705, 125.0000000000000000 ) ;
#4727 = ORIENTED_EDGE ( 'NONE', *, *, #49335, .T. ) ;
#4728 = ADVANCED_FACE ( 'NONE', ( #19749 ), #297, .T. ) ;
#4729 = VECTOR ( 'NONE', #46648, 1000.000000000000000 ) ;
#4730 = CARTESIAN_POINT ( 'NONE',  ( -332.3517673607765914, -70.03480886230919111, 25.08789112700620194 ) ) ;
#4731 = EDGE_CURVE ( 'NONE', #3968, #48534, #35781, .T. ) ;
#4732 = CARTESIAN_POINT ( 'NONE',  ( -336.3521761649654422, -72.48138011061176655, -29.74944317415788930 ) ) ;
#4733 = CARTESIAN_POINT ( 'NONE',  ( -340.0000000000000568, -123.5000000000000284, 0.000000000000000000 ) ) ;
#4734 = DIRECTION ( 'NONE',  ( 0.3482016354343995812, 0.000000000000000000, -0.9374196611341205632 ) ) ;
#4735 = EDGE_CURVE ( 'NONE', #12446, #23845, #31850, .T. ) ;
#4736 = ORIENTED_EDGE ( 'NONE', *, *, #46158, .F. ) ;
#4737 = CARTESIAN_POINT ( 'NONE',  ( -172.4422607493951318, -183.6283474603465606, 16.06677968424543579 ) ) ;
#4738 = CARTESIAN_POINT ( 'NONE',  ( 64.29733702426837283, -193.5000000000000000, 53.91167979418564471 ) ) ;
#4739 = ORIENTED_EDGE ( 'NONE', *, *, #37885, .F. ) ;
#4740 = CARTESIAN_POINT ( 'NONE',  ( -336.3521761649654422, -88.64083255475578937, 47.62880233550460218 ) ) ;
#4741 = VERTEX_POINT ( 'NONE', #27891 ) ;
#4742 = AXIS2_PLACEMENT_3D ( 'NONE', #33545, #12531, #48556 ) ;
#4743 = VECTOR ( 'NONE', #2048, 1000.000000000000000 ) ;
#4744 = ORIENTED_EDGE ( 'NONE', *, *, #24342, .T. ) ;
#4745 = PLANE ( 'NONE',  #40182 ) ;
#4746 = VECTOR ( 'NONE', #34437, 1000.000000000000000 ) ;
#4747 = DIRECTION ( 'NONE',  ( 0.000000000000000000, 0.000000000000000000, -1.000000000000000000 ) ) ;
#4748 = DIRECTION ( 'NONE',  ( 1.043714542225393381E-14, -0.9350162426854132791, 0.3546048870425396182 ) ) ;
#4751 = ORIENTED_EDGE ( 'NONE', *, *, #50761, .F. ) ;
#4750 = DIRECTION ( 'NONE',  ( -0.8858462335218260097, 0.000000000000000000, -0.4639789333096864810 ) ) ;
#4749 = DIRECTION ( 'NONE',  ( 0.000000000000000000, 0.6631226582407964143, 0.7485107481710999711 ) ) ;
#4752 = AXIS2_PLACEMENT_3D ( 'NONE', #6958, #27953, #7985 ) ;
#4753 = AXIS2_PLACEMENT_3D ( 'NONE', #40576, #4593, #4090 ) ;
#4754 = AXIS2_PLACEMENT_3D ( 'NONE', #12685, #41071, #342 ) ;
#4755 = CARTESIAN_POINT ( 'NONE',  ( -115.4536696835168641, -193.5000000000000000, -105.5434062319793185 ) ) ;
#4757 = ORIENTED_EDGE ( 'NONE', *, *, #32273, .F. ) ;
#4756 = VECTOR ( 'NONE', #16926, 1000.000000000000000 ) ;
#4758 = DIRECTION ( 'NONE',  ( 0.000000000000000000, -1.000000000000000000, 0.000000000000000000 ) ) ;
#4759 = DIRECTION ( 'NONE',  ( -0.000000000000000000, 0.000000000000000000, -1.000000000000000000 ) ) ;
#4760 = ORIENTED_EDGE ( 'NONE', *, *, #22770, .F. ) ;
#4761 = AXIS2_PLACEMENT_3D ( 'NONE', #17497, #1171, #20632 ) ;
#4762 = DIRECTION ( 'NONE',  ( 0.9785564922995032555, 0.000000000000000000, 0.2059786187411021818 ) ) ;
#4763 = DIRECTION ( 'NONE',  ( -0.000000000000000000, 0.8229838658936556861, -0.5680647467311569221 ) ) ;
#4764 = EDGE_LOOP ( 'NONE', ( #51388, #22551, #42688, #31227 ) ) ;
#4765 = CIRCLE ( 'NONE', #21543, 125.0000000000000000 ) ;
#4766 = EDGE_CURVE ( 'NONE', #19096, #21817, #46921, .T. ) ;
#4767 = LINE ( 'NONE', #1333, #33226 ) ;
#4768 = DIRECTION ( 'NONE',  ( -0.000000000000000000, 1.000000000000000000, -0.000000000000000000 ) ) ;
#4769 = PLANE ( 'NONE',  #29868 ) ;
#4770 = ORIENTED_EDGE ( 'NONE', *, *, #41010, .T. ) ;
#4771 = SURFACE_STYLE_FILL_AREA ( #16612 ) ;
#4772 = LINE ( 'NONE', #28407, #13118 ) ;
#4773 = LINE ( 'NONE', #24471, #15670 ) ;
#4774 = EDGE_CURVE ( 'NONE', #8596, #50621, #39970, .T. ) ;
#4775 = ADVANCED_FACE ( 'NONE', ( #32096 ), #12113, .T. ) ;
#4776 = ORIENTED_EDGE ( 'NONE', *, *, #15874, .T. ) ;
#4777 = EDGE_CURVE ( 'NONE', #20693, #27989, #4515, .T. ) ;
#4778 = LINE ( 'NONE', #13184, #38228 ) ;
#4779 = EDGE_CURVE ( 'NONE', #26640, #6875, #11345, .T. ) ;
#4780 = DIRECTION ( 'NONE',  ( 0.9151456172430210145, 0.000000000000000000, -0.4031234292879665171 ) ) ;
#4781 = ORIENTED_EDGE ( 'NONE', *, *, #34306, .F. ) ;
#4782 = VECTOR ( 'NONE', #48998, 1000.000000000000000 ) ;
#4783 = CIRCLE ( 'NONE', #8943, 125.0000000000000000 ) ;
#4784 = CARTESIAN_POINT ( 'NONE',  ( -332.3517673607765914, -123.5000000000000284, 0.000000000000000000 ) ) ;
#4785 = ADVANCED_FACE ( 'NONE', ( #23455 ), #41749, .F. ) ;
#4786 = DIRECTION ( 'NONE',  ( -0.5829794791144703447, 0.000000000000000000, -0.8124868780056825335 ) ) ;
#4787 = AXIS2_PLACEMENT_3D ( 'NONE', #19284, #26641, #39241 ) ;
#4788 = FACE_OUTER_BOUND ( 'NONE', #5093, .T. ) ;
#4789 = PLANE ( 'NONE',  #23904 ) ;
#4790 = CARTESIAN_POINT ( 'NONE',  ( -36.09284319799462537, -183.6283474603465606, 124.3848060646152618 ) ) ;
#4791 = EDGE_CURVE ( 'NONE', #30259, #26571, #13373, .T. ) ;
#4792 = ADVANCED_FACE ( 'NONE', ( #50169 ), #22561, .T. ) ;
#4793 = DIRECTION ( 'NONE',  ( -0.000000000000000000, -0.9709418174260534551, -0.2393156642875516327 ) ) ;
#4794 = CIRCLE ( 'NONE', #38320, 124.9999999999999858 ) ;
#4795 = ADVANCED_FACE ( 'NONE', ( #34376 ), #18090, .T. ) ;
#4796 = VECTOR ( 'NONE', #24671, 999.9999999999998863 ) ;
#4797 = CARTESIAN_POINT ( 'NONE',  ( -339.1964088526558498, -108.8949048983204051, 57.16590939599314680 ) ) ;
#4798 = FACE_OUTER_BOUND ( 'NONE', #44198, .T. ) ;
#4800 = ORIENTED_EDGE ( 'NONE', *, *, #490, .F. ) ;
#4799 = CARTESIAN_POINT ( 'NONE',  ( 73.09196206113300320, -193.5000000000000000, 29.07697310430963356 ) ) ;
#4801 = AXIS2_PLACEMENT_3D ( 'NONE', #41455, #40478, #32083 ) ;
#4802 = AXIS2_PLACEMENT_3D ( 'NONE', #39219, #17132, #28669 ) ;
#4803 = ADVANCED_FACE ( 'NONE', ( #30178 ), #22026, .F. ) ;
#4804 = ORIENTED_EDGE ( 'NONE', *, *, #25842, .T. ) ;
#4805 = LINE ( 'NONE', #48946, #27467 ) ;
#4806 = VECTOR ( 'NONE', #42, 1000.000000000000000 ) ;
#4807 = ADVANCED_FACE ( 'NONE', ( #13892 ), #33597, .F. ) ;
#4808 = VECTOR ( 'NONE', #44705, 1000.000000000000000 ) ;
#4809 = LINE ( 'NONE', #1100, #18779 ) ;
#4810 = ORIENTED_EDGE ( 'NONE', *, *, #45737, .T. ) ;
#4811 = ORIENTED_EDGE ( 'NONE', *, *, #26596, .F. ) ;
#4812 = ORIENTED_EDGE ( 'NONE', *, *, #34491, .F. ) ;
#4813 = DIRECTION ( 'NONE',  ( 0.2348860457809842095, 0.000000000000000000, -0.9720229140804107493 ) ) ;
#4814 = CARTESIAN_POINT ( 'NONE',  ( -64.08700758308646073, -189.7472609257535510, -124.0217483183786982 ) ) ;
#4815 = DIRECTION ( 'NONE',  ( 0.000000000000000000, -1.410908427127803051E-14, -1.000000000000000000 ) ) ;
#4816 = ORIENTED_EDGE ( 'NONE', *, *, #14898, .T. ) ;
#4817 = VERTEX_POINT ( 'NONE', #17587 ) ;
#4818 = EDGE_CURVE ( 'NONE', #34369, #9644, #1544, .T. ) ;
#4819 = EDGE_CURVE ( 'NONE', #1349, #12957, #519, .T. ) ;
#4820 = PLANE ( 'NONE',  #15978 ) ;
#4821 = VECTOR ( 'NONE', #6518, 1000.000000000000000 ) ;
#4823 = VERTEX_POINT ( 'NONE', #46221 ) ;
#4822 = CARTESIAN_POINT ( 'NONE',  ( -339.1964088526558498, -178.4886558749180949, 21.38919645685277970 ) ) ;
#4824 = AXIS2_PLACEMENT_3D ( 'NONE', #45269, #34196, #17413 ) ;
#4825 = CARTESIAN_POINT ( 'NONE',  ( -48.47912675150885065, -183.6283474603465606, 6.938893903907228378E-15 ) ) ;
#4826 = ORIENTED_EDGE ( 'NONE', *, *, #50049, .T. ) ;
#4827 = CARTESIAN_POINT ( 'NONE',  ( -49.29161362951452929, -189.7472609257535510, -0.5829794791144748967 ) ) ;
#4828 = VECTOR ( 'NONE', #26503, 999.9999999999998863 ) ;
#4829 = ORIENTED_EDGE ( 'NONE', *, *, #39321, .T. ) ;
#4830 = DIRECTION ( 'NONE',  ( 1.000000000000000000, -0.000000000000000000, 0.000000000000000000 ) ) ;
#4831 = DIRECTION ( 'NONE',  ( -0.8858462335218260097, -0.000000000000000000, 0.4639789333096864810 ) ) ;
#4832 = CARTESIAN_POINT ( 'NONE',  ( -49.40581635894068313, -193.5000000000000000, -0.3758275821142418316 ) ) ;
#4833 = EDGE_LOOP ( 'NONE', ( #26547, #7152, #9128, #12730 ) ) ;
#4834 = VECTOR ( 'NONE', #8231, 1000.000000000000000 ) ;
#4835 = ORIENTED_EDGE ( 'NONE', *, *, #22337, .F. ) ;
#4836 = CARTESIAN_POINT ( 'NONE',  ( -48.47912675150885065, -183.6283474603465606, 6.938893903907228378E-15 ) ) ;
#4837 = CARTESIAN_POINT ( 'NONE',  ( -55.71438232577009586, -175.3837268820161057, -124.7904286264580662 ) ) ;
#4838 = AXIS2_PLACEMENT_3D ( 'NONE', #45796, #33459, #13475 ) ;
#4839 = VERTEX_POINT ( 'NONE', #38574 ) ;
#4840 = CARTESIAN_POINT ( 'NONE',  ( -2.700932609314997457, -193.5000000000000000, -116.3157639405751809 ) ) ;
#4841 = VECTOR ( 'NONE', #1469, 1000.000000000000000 ) ;
#4842 = LINE ( 'NONE', #24534, #43832 ) ;
#4843 = EDGE_CURVE ( 'NONE', #8199, #2225, #2573, .T. ) ;
#4844 = EDGE_CURVE ( 'NONE', #47870, #32445, #46467, .T. ) ;
#4845 = ORIENTED_EDGE ( 'NONE', *, *, #38552, .T. ) ;
#4846 = PLANE ( 'NONE',  #51947 ) ;
#4847 = CIRCLE ( 'NONE', #42604, 60.00000000000000000 ) ;
#4848 = CARTESIAN_POINT ( 'NONE',  ( -305.0000000000000568, -115.7716958700755470, -59.50019592636139265 ) ) ;
#4849 = EDGE_CURVE ( 'NONE', #36987, #11325, #45697, .T. ) ;
#4850 = CIRCLE ( 'NONE', #45147, 12.00000000000000000 ) ;
#4851 = ADVANCED_FACE ( 'NONE', ( #42244 ), #45440, .F. ) ;
#4852 = ORIENTED_EDGE ( 'NONE', *, *, #48458, .T. ) ;
#4853 = CARTESIAN_POINT ( 'NONE',  ( -330.4913330509368166, -123.5000000000000284, 0.000000000000000000 ) ) ;
#4854 = VERTEX_POINT ( 'NONE', #25712 ) ;
#4855 = CARTESIAN_POINT ( 'NONE',  ( -332.3517673607765914, -92.15051119686104641, -50.05135858667769355 ) ) ;
#4856 = ORIENTED_EDGE ( 'NONE', *, *, #1266, .T. ) ;
#4857 = PLANE ( 'NONE',  #23177 ) ;
#4858 = CARTESIAN_POINT ( 'NONE',  ( -95.18697522258271704, -183.6283474603465606, 115.9455772817713211 ) ) ;
#4859 = CARTESIAN_POINT ( 'NONE',  ( -332.3517673607765914, -65.65568511206123503, -15.93848283698870105 ) ) ;
#4860 = CARTESIAN_POINT ( 'NONE',  ( -305.0000000000000568, -182.6878972721721084, 9.838334030658062446 ) ) ;
#4861 = VERTEX_POINT ( 'NONE', #18358 ) ;
#4862 = DIRECTION ( 'NONE',  ( 0.7378332790417239107, 0.000000000000000000, 0.6749830015182142207 ) ) ;
#4863 = ORIENTED_EDGE ( 'NONE', *, *, #5697, .T. ) ;
#4864 = ORIENTED_EDGE ( 'NONE', *, *, #31099, .T. ) ;
#4865 = VECTOR ( 'NONE', #20072, 1000.000000000000114 ) ;
#4866 = VECTOR ( 'NONE', #2621, 1000.000000000000000 ) ;
#4867 = EDGE_CURVE ( 'NONE', #39129, #23608, #33853, .T. ) ;
#4868 = CARTESIAN_POINT ( 'NONE',  ( -238.7407812814481076, -213.5000000000000000, -41.45482488023466061 ) ) ;
#4870 = EDGE_LOOP ( 'NONE', ( #49194, #278, #42297, #16027 ) ) ;
#4869 = CARTESIAN_POINT ( 'NONE',  ( -49.25565061422690150, -175.3837268820161057, 0.6300878435817109935 ) ) ;
#4871 = AXIS2_PLACEMENT_3D ( 'NONE', #6688, #14838, #14311 ) ;
#4872 = ORIENTED_EDGE ( 'NONE', *, *, #30380, .T. ) ;
#4873 = DIRECTION ( 'NONE',  ( -1.000000000000000000, 7.812315528781795159E-15, -6.921107616850865492E-15 ) ) ;
#4874 = ADVANCED_FACE ( 'NONE', ( #29909 ), #9956, .F. ) ;
#4875 = CARTESIAN_POINT ( 'NONE',  ( -135.6699833737243637, -189.7472609257535510, 89.56983042009322560 ) ) ;
#4876 = CIRCLE ( 'NONE', #24152, 4.000000000000003553 ) ;
#4877 = EDGE_LOOP ( 'NONE', ( #5711, #24882, #28345, #18724 ) ) ;
#4878 = PLANE ( 'NONE',  #18889 ) ;
#4879 = VERTEX_POINT ( 'NONE', #6003 ) ;
#4880 = DIRECTION ( 'NONE',  ( -0.6068001458185834363, 0.000000000000000000, -0.7948544414133608127 ) ) ;
#4881 = DIRECTION ( 'NONE',  ( -0.9995608365087940150, 0.000000000000000000, -0.02963332782257007206 ) ) ;
#4882 = PLANE ( 'NONE',  #2594 ) ;
#4883 = FACE_BOUND ( 'NONE', #51499, .T. ) ;
#4884 = ORIENTED_EDGE ( 'NONE', *, *, #40643, .T. ) ;
#4885 = ORIENTED_EDGE ( 'NONE', *, *, #26417, .T. ) ;
#4886 = ORIENTED_EDGE ( 'NONE', *, *, #21660, .F. ) ;
#4887 = AXIS2_PLACEMENT_3D ( 'NONE', #49172, #36541, #24461 ) ;
#4888 = DIRECTION ( 'NONE',  ( 0.000000000000000000, -0.000000000000000000, -1.000000000000000000 ) ) ;
#4889 = LINE ( 'NONE', #25367, #27703 ) ;
#4890 = DIRECTION ( 'NONE',  ( 0.000000000000000000, -0.000000000000000000, -1.000000000000000000 ) ) ;
#4891 = CARTESIAN_POINT ( 'NONE',  ( -38.66762320617019100, -183.6283474603465606, -124.6143426664033882 ) ) ;
#4892 = CARTESIAN_POINT ( 'NONE',  ( -339.1964088526558498, -178.8432607619606358, 20.45418021416736565 ) ) ;
#4893 = ORIENTED_EDGE ( 'NONE', *, *, #34825, .T. ) ;
#4894 = ORIENTED_EDGE ( 'NONE', *, *, #50777, .F. ) ;
#4896 = ORIENTED_EDGE ( 'NONE', *, *, #42575, .T. ) ;
#4895 = LINE ( 'NONE', #24852, #44983 ) ;
#4897 = CIRCLE ( 'NONE', #30885, 13.99999999999998934 ) ;
#4898 = ORIENTED_EDGE ( 'NONE', *, *, #19246, .T. ) ;
#4899 = AXIS2_PLACEMENT_3D ( 'NONE', #44054, #48266, #20658 ) ;
#4901 = AXIS2_PLACEMENT_3D ( 'NONE', #31826, #20248, #35491 ) ;
#4900 = DIRECTION ( 'NONE',  ( 0.000000000000000000, -1.000000000000000000, 0.000000000000000000 ) ) ;
#4902 = FACE_OUTER_BOUND ( 'NONE', #17787, .T. ) ;
#4903 = VECTOR ( 'NONE', #37370, 1000.000000000000000 ) ;
#4904 = DIRECTION ( 'NONE',  ( 0.000000000000000000, 0.000000000000000000, -1.000000000000000000 ) ) ;
#4905 = FACE_OUTER_BOUND ( 'NONE', #322, .T. ) ;
#4906 = EDGE_CURVE ( 'NONE', #32338, #38633, #38047, .T. ) ;
#4907 = LINE ( 'NONE', #9104, #34320 ) ;
#4908 = ORIENTED_EDGE ( 'NONE', *, *, #14096, .F. ) ;
#4909 = DIRECTION ( 'NONE',  ( -1.000000000000000000, 0.000000000000000000, 0.000000000000000000 ) ) ;
#4910 = ORIENTED_EDGE ( 'NONE', *, *, #2601, .F. ) ;
#4911 = ORIENTED_EDGE ( 'NONE', *, *, #15194, .F. ) ;
#4912 = CARTESIAN_POINT ( 'NONE',  ( 1.755575411425465360, -193.5000000000000000, 114.4616734920527392 ) ) ;
#4913 = CIRCLE ( 'NONE', #34273, 124.9999999999999858 ) ;
#4914 = DIRECTION ( 'NONE',  ( -0.000000000000000000, 0.9927088740980556381, 0.1205366802553095307 ) ) ;
#4915 = CARTESIAN_POINT ( 'NONE',  ( -34.63763967761164508, -175.3837268820161057, -123.2250735253142864 ) ) ;
#4916 = DIRECTION ( 'NONE',  ( -1.000000000000000000, -0.000000000000000000, 4.884776371667511665E-16 ) ) ;
#4917 = LINE ( 'NONE', #41415, #16303 ) ;
#4918 = CARTESIAN_POINT ( 'NONE',  ( 25.43954814678887644, -183.6283474603465606, 100.8019320314832754 ) ) ;
#4919 = EDGE_LOOP ( 'NONE', ( #12716, #6157, #18491, #35139 ) ) ;
#4920 = DIRECTION ( 'NONE',  ( 0.000000000000000000, 0.000000000000000000, 1.000000000000000000 ) ) ;
#4921 = LINE ( 'NONE', #1210, #47546 ) ;
#4922 = AXIS2_PLACEMENT_3D ( 'NONE', #30473, #1841, #17884 ) ;
#4923 = DIRECTION ( 'NONE',  ( 1.000000000000000000, 0.000000000000000000, 0.000000000000000000 ) ) ;
#4925 = FACE_BOUND ( 'NONE', #25137, .T. ) ;
#4924 = PRODUCT_RELATED_PRODUCT_CATEGORY ( 'part', '', ( #30214 ) ) ;
#4926 = ORIENTED_EDGE ( 'NONE', *, *, #7852, .T. ) ;
#4927 = EDGE_CURVE ( 'NONE', #29810, #35254, #10720, .T. ) ;
#4928 = LINE ( 'NONE', #20952, #28960 ) ;
#4929 = ORIENTED_EDGE ( 'NONE', *, *, #49046, .T. ) ;
#4930 = DIRECTION ( 'NONE',  ( -0.000000000000000000, 1.000000000000000000, -0.000000000000000000 ) ) ;
#4931 = EDGE_LOOP ( 'NONE', ( #26759, #38319, #25353, #4431 ) ) ;
#4932 = DIRECTION ( 'NONE',  ( 0.9929810960135161402, 0.000000000000000000, 0.1182731709213730997 ) ) ;
#4933 = ORIENTED_EDGE ( 'NONE', *, *, #7554, .F. ) ;
#4934 = AXIS2_PLACEMENT_3D ( 'NONE', #44406, #16813, #769 ) ;
#4935 = FACE_OUTER_BOUND ( 'NONE', #16729, .T. ) ;
#4936 = AXIS2_PLACEMENT_3D ( 'NONE', #22735, #14597, #30600 ) ;
#4937 = VECTOR ( 'NONE', #15751, 1000.000000000000000 ) ;
#4938 = LINE ( 'NONE', #13054, #25935 ) ;
#4940 = ORIENTED_EDGE ( 'NONE', *, *, #48536, .T. ) ;
#4939 = LINE ( 'NONE', #20962, #32135 ) ;
#4941 = AXIS2_PLACEMENT_3D ( 'NONE', #49927, #22062, #22592 ) ;
#4942 = EDGE_CURVE ( 'NONE', #48950, #1552, #14663, .T. ) ;
#4943 = CARTESIAN_POINT ( 'NONE',  ( -47.97059563285963435, -189.7472609257535510, 0.8610436117673654355 ) ) ;
#4944 = ORIENTED_EDGE ( 'NONE', *, *, #48824, .F. ) ;
#4945 = EDGE_LOOP ( 'NONE', ( #14046, #15469, #22508, #16520 ) ) ;
#4946 = ORIENTED_EDGE ( 'NONE', *, *, #21031, .F. ) ;
#4947 = LINE ( 'NONE', #19100, #13306 ) ;
#4948 = AXIS2_PLACEMENT_3D ( 'NONE', #17035, #49079, #41441 ) ;
#4949 = CARTESIAN_POINT ( 'NONE',  ( -111.3295483157475729, -175.3837268820161057, 108.0501018472332362 ) ) ;
#4950 = EDGE_CURVE ( 'NONE', #43377, #19283, #10971, .T. ) ;
#4951 = ORIENTED_EDGE ( 'NONE', *, *, #20866, .F. ) ;
#4952 = FILL_AREA_STYLE_COLOUR ( '', #7451 ) ;
#4953 = CARTESIAN_POINT ( 'NONE',  ( -62.97606545226379637, -175.3837268820161057, -123.1496609813404177 ) ) ;
#4954 = CARTESIAN_POINT ( 'NONE',  ( -164.3791542526839464, -189.7472609257535510, 46.82076062204520639 ) ) ;
#4955 = AXIS2_PLACEMENT_3D ( 'NONE', #38295, #21768, #14396 ) ;
#4956 = EDGE_CURVE ( 'NONE', #26038, #49256, #18606, .T. ) ;
#4957 = CARTESIAN_POINT ( 'NONE',  ( -332.3517673607765914, -169.4076645216271402, -37.15394033962039089 ) ) ;
#4958 = LINE ( 'NONE', #29104, #40756 ) ;
#4959 = ORIENTED_EDGE ( 'NONE', *, *, #30356, .F. ) ;
#4962 = ORIENTED_EDGE ( 'NONE', *, *, #38155, .F. ) ;
#4961 = CARTESIAN_POINT ( 'NONE',  ( -336.3521761649653854, -143.2422018649890276, 56.65902810251888155 ) ) ;
#4960 = CARTESIAN_POINT ( 'NONE',  ( -49.35486169370448550, -177.1207230881787780, -0.4827922027307481878 ) ) ;
#4963 = ORIENTED_EDGE ( 'NONE', *, *, #9017, .F. ) ;
#4964 = CARTESIAN_POINT ( 'NONE',  ( -99.02518858244150124, -175.3837268820161057, 114.3245189510261497 ) ) ;
#4965 = ORIENTED_EDGE ( 'NONE', *, *, #23692, .F. ) ;
#4966 = FACE_OUTER_BOUND ( 'NONE', #39955, .T. ) ;
#4967 = VERTEX_POINT ( 'NONE', #3086 ) ;
#4968 = DIRECTION ( 'NONE',  ( 0.000000000000000000, -0.2393156642875482742, 0.9709418174260544543 ) ) ;
#4969 = EDGE_CURVE ( 'NONE', #34216, #27501, #3347, .T. ) ;
#4970 = CARTESIAN_POINT ( 'NONE',  ( -48.47912675150885065, -183.6283474603465606, 6.938893903907228378E-15 ) ) ;
#4971 = EDGE_LOOP ( 'NONE', ( #23890, #46570, #15532, #46947 ) ) ;
#4972 = DIRECTION ( 'NONE',  ( 0.000000000000000000, 0.000000000000000000, 1.000000000000000000 ) ) ;
#4973 = ORIENTED_EDGE ( 'NONE', *, *, #41733, .T. ) ;
#4974 = ORIENTED_EDGE ( 'NONE', *, *, #43975, .T. ) ;
#4975 = FACE_OUTER_BOUND ( 'NONE', #29299, .T. ) ;
#4976 = ADVANCED_FACE ( 'NONE', ( #38822 ), #19128, .T. ) ;
#4977 = CARTESIAN_POINT ( 'NONE',  ( -339.1964088526558498, -150.9396941197147726, 53.35787839313415759 ) ) ;
#4978 = VECTOR ( 'NONE', #26764, 1000.000000000000000 ) ;
#4979 = CARTESIAN_POINT ( 'NONE',  ( -332.3517673607765914, -153.6873197461136442, -51.85292399224849902 ) ) ;
#4980 =( LENGTH_UNIT ( ) NAMED_UNIT ( * ) SI_UNIT ( .MILLI., .METRE. ) );
#4981 = ORIENTED_EDGE ( 'NONE', *, *, #51911, .T. ) ;
#4982 = VECTOR ( 'NONE', #45100, 999.9999999999998863 ) ;
#4983 = DIRECTION ( 'NONE',  ( 0.000000000000000000, -0.000000000000000000, -1.000000000000000000 ) ) ;
#4984 = PRODUCT_CONTEXT ( 'NONE', #41108, 'mechanical' ) ;
#4985 = CARTESIAN_POINT ( 'NONE',  ( -48.64924157374594671, -175.3837268820161057, 124.9998842437354227 ) ) ;
#4986 = LINE ( 'NONE', #49390, #2698 ) ;
#4987 = LINE ( 'NONE', #17336, #2828 ) ;
#4988 = LINE ( 'NONE', #24678, #50854 ) ;
#4989 = DIRECTION ( 'NONE',  ( 0.000000000000000000, 0.000000000000000000, 1.000000000000000000 ) ) ;
#4990 = VECTOR ( 'NONE', #12276, 1000.000000000000000 ) ;
#4991 = ORIENTED_EDGE ( 'NONE', *, *, #4182, .T. ) ;
#4992 = DIRECTION ( 'NONE',  ( 0.000000000000000000, 0.000000000000000000, -1.000000000000000000 ) ) ;
#4993 = ADVANCED_FACE ( 'NONE', ( #47765 ), #11740, .F. ) ;
#4994 = CARTESIAN_POINT ( 'NONE',  ( 75.21854001195777073, -177.1207230881787780, -8.665274887905439982 ) ) ;
#4995 = PLANE ( 'NONE',  #14420 ) ;
#4996 = AXIS2_PLACEMENT_3D ( 'NONE', #29745, #9792, #2668 ) ;
#4997 = EDGE_LOOP ( 'NONE', ( #1117, #27493, #34912, #45983 ) ) ;
#4998 = ORIENTED_EDGE ( 'NONE', *, *, #20880, .T. ) ;
#4999 = ORIENTED_EDGE ( 'NONE', *, *, #11407, .F. ) ;
#5000 = VECTOR ( 'NONE', #51137, 1000.000000000000000 ) ;
#5001 = DIRECTION ( 'NONE',  ( 0.2348860457809707758, 0.000000000000000000, 0.9720229140804138579 ) ) ;
#5002 = CARTESIAN_POINT ( 'NONE',  ( -48.47912675150885065, -177.1207230881787780, 6.938893903907228378E-15 ) ) ;
#5003 = FACE_OUTER_BOUND ( 'NONE', #257, .T. ) ;
#5004 = DIRECTION ( 'NONE',  ( -1.000000000000000000, 0.000000000000000000, 0.000000000000000000 ) ) ;
#5005 = ORIENTED_EDGE ( 'NONE', *, *, #41431, .T. ) ;
#5006 = DIRECTION ( 'NONE',  ( 0.000000000000000000, 5.157911135237706217E-14, -1.000000000000000000 ) ) ;
#5007 = ORIENTED_EDGE ( 'NONE', *, *, #31948, .F. ) ;
#5008 = CARTESIAN_POINT ( 'NONE',  ( -47.70260288879080690, -183.6283474603465606, -0.6300878435817026668 ) ) ;
#5009 = ORIENTED_EDGE ( 'NONE', *, *, #21442, .T. ) ;
#5010 = DIRECTION ( 'NONE',  ( -0.000000000000000000, -1.000000000000000000, 0.000000000000000000 ) ) ;
#5011 = AXIS2_PLACEMENT_3D ( 'NONE', #24563, #40578, #12727 ) ;
#5012 = ORIENTED_EDGE ( 'NONE', *, *, #33400, .F. ) ;
#5013 = DIRECTION ( 'NONE',  ( -0.4566292373937018145, 0.000000000000000000, -0.8896570909947529859 ) ) ;
#5014 = VECTOR ( 'NONE', #10304, 1000.000000000000227 ) ;
#5015 = EDGE_CURVE ( 'NONE', #38434, #8106, #15623, .T. ) ;
#5016 = ADVANCED_FACE ( 'NONE', ( #35655 ), #42779, .F. ) ;
#5017 = DIRECTION ( 'NONE',  ( -0.000000000000000000, 0.6631226582408039638, 0.7485107481710934207 ) ) ;
#5018 = PRODUCT_DEFINITION_SHAPE ( 'NONE', 'NONE',  #52045 ) ;
#5019 = CARTESIAN_POINT ( 'NONE',  ( -12.13476221271688615, -175.3837268820161057, 119.5996955107804638 ) ) ;
#5022 = ORIENTED_EDGE ( 'NONE', *, *, #10158, .F. ) ;
#5021 = DIRECTION ( 'NONE',  ( 0.000000000000000000, 0.000000000000000000, 1.000000000000000000 ) ) ;
#5020 = CARTESIAN_POINT ( 'NONE',  ( -1.600401561467127700E-24, 58.14470866581338271, -16.45750525699328293 ) ) ;
#5023 = DIRECTION ( 'NONE',  ( -0.9785564922995017012, 0.000000000000000000, -0.2059786187411094538 ) ) ;
#5024 = ORIENTED_EDGE ( 'NONE', *, *, #40626, .F. ) ;
#5025 = CARTESIAN_POINT ( 'NONE',  ( -146.0653709326077490, -189.7472609257535510, -78.11481899503411341 ) ) ;
#5026 = DIRECTION ( 'NONE',  ( -0.000000000000000000, 1.000000000000000000, -0.000000000000000000 ) ) ;
#5027 = ORIENTED_EDGE ( 'NONE', *, *, #17642, .F. ) ;
#5028 = EDGE_CURVE ( 'NONE', #21361, #25289, #6784, .T. ) ;
#5029 = CARTESIAN_POINT ( 'NONE',  ( 67.66641500972444589, -189.7472609257535510, 46.20836643931066590 ) ) ;
#5031 = DIRECTION ( 'NONE',  ( 0.9473263538541899509, 0.000000000000000000, 0.3202698538628415692 ) ) ;
#5030 = DIRECTION ( 'NONE',  ( -0.4031234292879600778, 0.000000000000000000, -0.9151456172430237901 ) ) ;
#5032 = ORIENTED_EDGE ( 'NONE', *, *, #46874, .T. ) ;
#5033 = EDGE_CURVE ( 'NONE', #16704, #49741, #45003, .T. ) ;
#5034 = VECTOR ( 'NONE', #8037, 1000.000000000000000 ) ;
#5035 = CARTESIAN_POINT ( 'NONE',  ( -336.3521761649654422, -179.2447759217480154, -19.39547174791710660 ) ) ;
#5036 = PLANE ( 'NONE',  #27015 ) ;
#5037 = EDGE_CURVE ( 'NONE', #51798, #2804, #27249, .T. ) ;
#5038 = DIRECTION ( 'NONE',  ( 0.000000000000000000, 1.000000000000000000, -0.000000000000000000 ) ) ;
#5039 = ORIENTED_EDGE ( 'NONE', *, *, #14585, .T. ) ;
#5040 = CARTESIAN_POINT ( 'NONE',  ( -171.4559849729830603, -183.6283474603465606, 22.39848972532371718 ) ) ;
#5041 = SURFACE_STYLE_FILL_AREA ( #49956 ) ;
#5042 = CARTESIAN_POINT ( 'NONE',  ( -38.66762320617019100, -177.1207230881787780, -124.6143426664033882 ) ) ;
#5043 = CARTESIAN_POINT ( 'NONE',  ( -166.8403286750647680, -189.7472609257535510, -40.19484891389974734 ) ) ;
#5044 = ADVANCED_FACE ( 'NONE', ( #47501 ), #7802, .F. ) ;
#5045 = ORIENTED_EDGE ( 'NONE', *, *, #44887, .F. ) ;
#5046 = CARTESIAN_POINT ( 'NONE',  ( -141.5426765053792906, -183.6283474603465606, 81.94739446021134199 ) ) ;
#5047 = DIRECTION ( 'NONE',  ( -0.000000000000000000, 1.000000000000000000, -0.000000000000000000 ) ) ;
#5048 = ORIENTED_EDGE ( 'NONE', *, *, #36756, .F. ) ;
#5049 = VECTOR ( 'NONE', #16956, 1000.000000000000000 ) ;
#5050 = CARTESIAN_POINT ( 'NONE',  ( 76.04209377433249983, -189.7472609257535510, -10.93003379476865611 ) ) ;
#5051 = CARTESIAN_POINT ( 'NONE',  ( -332.3517673607765914, -71.15086438280971493, -29.31839013542551342 ) ) ;
#5052 = DIRECTION ( 'NONE',  ( -0.1768902751225666370, 0.000000000000000000, -0.9842305779475979399 ) ) ;
#5053 = DIRECTION ( 'NONE',  ( -0.000000000000000000, 1.000000000000000000, -0.000000000000000000 ) ) ;
#5054 = CARTESIAN_POINT ( 'NONE',  ( -280.0000000000000000, -123.5000000000000284, 6.938893903907228378E-15 ) ) ;
#5055 = CARTESIAN_POINT ( 'NONE',  ( -143.2689064740322067, -183.6283474603465606, -79.94433946042767047 ) ) ;
#5056 = LINE ( 'NONE', #21863, #37115 ) ;
#5058 = ORIENTED_EDGE ( 'NONE', *, *, #13061, .T. ) ;
#5057 = DIRECTION ( 'NONE',  ( -0.000000000000000000, 1.000000000000000000, -0.000000000000000000 ) ) ;
#5059 = EDGE_LOOP ( 'NONE', ( #46114, #4300, #33440, #28529 ) ) ;
#5060 = LINE ( 'NONE', #41835, #19892 ) ;
#5061 = AXIS2_PLACEMENT_3D ( 'NONE', #2995, #18005, #10886 ) ;
#5062 = VECTOR ( 'NONE', #26047, 1000.000000000000000 ) ;
#5063 = DIRECTION ( 'NONE',  ( 0.000000000000000000, 1.000000000000000000, 0.000000000000000000 ) ) ;
#5064 = ORIENTED_EDGE ( 'NONE', *, *, #34902, .F. ) ;
#5065 = EDGE_LOOP ( 'NONE', ( #16560, #8801, #35858, #4829 ) ) ;
#5067 = EDGE_CURVE ( 'NONE', #21790, #47759, #31199, .T. ) ;
#5066 = ORIENTED_EDGE ( 'NONE', *, *, #27417, .T. ) ;
#5068 = CARTESIAN_POINT ( 'NONE',  ( -48.47912675150885065, -177.1207230881787780, 6.938893903907228378E-15 ) ) ;
#5069 = EDGE_CURVE ( 'NONE', #48404, #40700, #47252, .T. ) ;
#5070 = EDGE_CURVE ( 'NONE', #25951, #26701, #11220, .T. ) ;
#5071 = ADVANCED_FACE ( 'NONE', ( #51200 ), #15186, .F. ) ;
#5072 = FACE_OUTER_BOUND ( 'NONE', #25891, .T. ) ;
#5073 = CARTESIAN_POINT ( 'NONE',  ( -49.47868758801764955, -193.5000000000000000, -0.02963332782256313663 ) ) ;
#5074 = ORIENTED_EDGE ( 'NONE', *, *, #34657, .F. ) ;
#5075 = ORIENTED_EDGE ( 'NONE', *, *, #13394, .T. ) ;
#5076 = EDGE_CURVE ( 'NONE', #32067, #22651, #3879, .T. ) ;
#5077 = CARTESIAN_POINT ( 'NONE',  ( -332.3517673607765914, -182.6878972721721084, 9.838334030658062446 ) ) ;
#5079 = VERTEX_POINT ( 'NONE', #44341 ) ;
#5078 = DIRECTION ( 'NONE',  ( 0.8455960035018199594, 0.000000000000000000, 0.5338233779648003940 ) ) ;
#5080 = CIRCLE ( 'NONE', #34444, 125.0000000000000000 ) ;
#5081 = EDGE_CURVE ( 'NONE', #39780, #15096, #51717, .T. ) ;
#5082 = EDGE_CURVE ( 'NONE', #471, #24853, #29032, .T. ) ;
#5083 = CARTESIAN_POINT ( 'NONE',  ( 76.01188277843577623, -189.7472609257535510, 11.26891947860283061 ) ) ;
#5084 = VERTEX_POINT ( 'NONE', #28021 ) ;
#5085 = CARTESIAN_POINT ( 'NONE',  ( -339.1964088526558498, -175.5095439275173135, 27.86139516340941213 ) ) ;
#5086 = EDGE_LOOP ( 'NONE', ( #11415, #8588, #17385, #34730 ) ) ;
#5087 = PLANE ( 'NONE',  #38323 ) ;
#5088 = EDGE_CURVE ( 'NONE', #45420, #36303, #16214, .T. ) ;
#5089 = DIRECTION ( 'NONE',  ( -0.000000000000000000, 0.9709418174260553425, 0.2393156642875449158 ) ) ;
#5090 = CARTESIAN_POINT ( 'NONE',  ( -40.24578378811990831, -193.5000000000000000, 124.7285535218268251 ) ) ;
#5091 = EDGE_CURVE ( 'NONE', #36064, #46209, #37443, .T. ) ;
#5092 = ORIENTED_EDGE ( 'NONE', *, *, #20266, .T. ) ;
#5093 = EDGE_LOOP ( 'NONE', ( #12922, #7712, #8845, #13939 ) ) ;
#5094 = CARTESIAN_POINT ( 'NONE',  ( 70.98542830588607444, -193.5000000000000000, -36.78613984829961936 ) ) ;
#5095 = EDGE_CURVE ( 'NONE', #17485, #23694, #24870, .T. ) ;
#5096 = CARTESIAN_POINT ( 'NONE',  ( -167.1668396246903114, -177.1207230881787780, -35.90758392117661657 ) ) ;
#5097 = ORIENTED_EDGE ( 'NONE', *, *, #46111, .T. ) ;
#5098 = DIRECTION ( 'NONE',  ( -0.000000000000000000, 1.000000000000000000, -0.000000000000000000 ) ) ;
#5099 = ADVANCED_FACE ( 'NONE', ( #16751 ), #44062, .T. ) ;
#5100 = CARTESIAN_POINT ( 'NONE',  ( -48.41988612361514299, -193.5000000000000000, -0.9982437317643144681 ) ) ;
#5101 = VERTEX_POINT ( 'NONE', #40358 ) ;
#5102 = FACE_OUTER_BOUND ( 'NONE', #18635, .T. ) ;
#5103 = EDGE_CURVE ( 'NONE', #38078, #5877, #10589, .T. ) ;
#5104 = CARTESIAN_POINT ( 'NONE',  ( 63.82222181224018698, -175.3837268820161057, 52.57768177182521896 ) ) ;
#5105 = VECTOR ( 'NONE', #33395, 1000.000000000000000 ) ;
#5106 = AXIS2_PLACEMENT_3D ( 'NONE', #48415, #36310, #5052 ) ;
#5107 = ORIENTED_EDGE ( 'NONE', *, *, #22979, .T. ) ;
#5108 = LINE ( 'NONE', #638, #4756 ) ;
#5109 = ORIENTED_EDGE ( 'NONE', *, *, #9017, .T. ) ;
#5110 = LINE ( 'NONE', #12965, #22060 ) ;
#5111 = LINE ( 'NONE', #13249, #29420 ) ;
#5112 = VERTEX_POINT ( 'NONE', #4915 ) ;
#5113 = PLANE ( 'NONE',  #22351 ) ;
#5114 = CARTESIAN_POINT ( 'NONE',  ( -49.32472275501068282, -175.3837268820161057, 0.5338233779647895139 ) ) ;
#5115 = CYLINDRICAL_SURFACE ( 'NONE', #12301, 125.0000000000000000 ) ;
#5116 = DIRECTION ( 'NONE',  ( 0.9646355819083594074, 0.000000000000000000, -0.2635871660690647933 ) ) ;
#5117 = EDGE_CURVE ( 'NONE', #12735, #1095, #3869, .T. ) ;
#5118 = EDGE_LOOP ( 'NONE', ( #17205, #8368, #34996, #10046 ) ) ;
#5119 = DIRECTION ( 'NONE',  ( -0.000000000000000000, 1.000000000000000000, -0.000000000000000000 ) ) ;
#5120 = VERTEX_POINT ( 'NONE', #32756 ) ;
#5121 = EDGE_LOOP ( 'NONE', ( #8622, #11437, #47841, #17475 ) ) ;
#5122 = VECTOR ( 'NONE', #7259, 1000.000000000000000 ) ;
#5123 = CARTESIAN_POINT ( 'NONE',  ( -330.4913330509368166, -89.00580675195338642, -49.09328500076577484 ) ) ;
#5125 = EDGE_LOOP ( 'NONE', ( #45449, #7926, #8710, #24424 ) ) ;
#5124 = CARTESIAN_POINT ( 'NONE',  ( -336.3521761649654422, -148.5878911270064009, 53.46519113769075204 ) ) ;
#5126 = EDGE_LOOP ( 'NONE', ( #38864, #2851, #48361, #29230 ) ) ;
#5127 = CARTESIAN_POINT ( 'NONE',  ( 75.47134233844786877, -193.5000000000000000, -3.504489105734896803 ) ) ;
#5128 = ADVANCED_FACE ( 'NONE', ( #40616 ), #19890, .F. ) ;
#5129 = LINE ( 'NONE', #9070, #13684 ) ;
#5130 = CARTESIAN_POINT ( 'NONE',  ( -127.4665351220365608, -183.6283474603465606, -96.88131563365296017 ) ) ;
#5131 = ORIENTED_EDGE ( 'NONE', *, *, #3446, .F. ) ;
#5132 = DIRECTION ( 'NONE',  ( 0.000000000000000000, 1.000000000000000000, 0.000000000000000000 ) ) ;
#5133 = ORIENTED_EDGE ( 'NONE', *, *, #47370, .T. ) ;
#5134 = DIRECTION ( 'NONE',  ( -0.000000000000000000, 1.000000000000000000, -0.000000000000000000 ) ) ;
#5135 = CARTESIAN_POINT ( 'NONE',  ( -260.0000000000000000, -93.50000000000001421, -51.54700538379269403 ) ) ;
#5136 = VECTOR ( 'NONE', #32364, 1000.000000000000000 ) ;
#5137 = ADVANCED_FACE ( 'NONE', ( #48273 ), #423, .T. ) ;
#5138 = EDGE_CURVE ( 'NONE', #4337, #30281, #32413, .T. ) ;
#5139 = EDGE_CURVE ( 'NONE', #48181, #3854, #31970, .T. ) ;
#5140 = DIRECTION ( 'NONE',  ( -0.000000000000000000, 1.000000000000000000, -0.000000000000000000 ) ) ;
#5141 = DIRECTION ( 'NONE',  ( -1.000000000000000000, 0.000000000000000000, 0.000000000000000000 ) ) ;
#5142 = ORIENTED_EDGE ( 'NONE', *, *, #18952, .F. ) ;
#5143 = ORIENTED_EDGE ( 'NONE', *, *, #51972, .T. ) ;
#5144 = EDGE_CURVE ( 'NONE', #45713, #51152, #11993, .T. ) ;
#5146 = VERTEX_POINT ( 'NONE', #20149 ) ;
#5145 = CIRCLE ( 'NONE', #35319, 20.00000000000000355 ) ;
#5147 = FACE_OUTER_BOUND ( 'NONE', #18775, .T. ) ;
#5148 = CARTESIAN_POINT ( 'NONE',  ( 76.43863189440992301, -189.7472609257535510, -4.533605064403313456 ) ) ;
#5149 = CARTESIAN_POINT ( 'NONE',  ( -330.0000000000000568, -91.84230854612501105, 0.000000000000000000 ) ) ;
#5150 = FACE_BOUND ( 'NONE', #22354, .T. ) ;
#5151 = PLANE ( 'NONE',  #40637 ) ;
#5152 = ORIENTED_EDGE ( 'NONE', *, *, #16410, .T. ) ;
#5153 = ORIENTED_EDGE ( 'NONE', *, *, #34955, .T. ) ;
#5155 = EDGE_LOOP ( 'NONE', ( #28531, #14817, #44995, #43158 ) ) ;
#5154 = PLANE ( 'NONE',  #39095 ) ;
#5156 = ORIENTED_EDGE ( 'NONE', *, *, #44885, .T. ) ;
#5157 = CIRCLE ( 'NONE', #1802, 60.00000000000000000 ) ;
#5158 = EDGE_CURVE ( 'NONE', #13423, #4690, #7250, .T. ) ;
#5159 = FACE_OUTER_BOUND ( 'NONE', #50140, .T. ) ;
#5160 = CARTESIAN_POINT ( 'NONE',  ( -164.8312043469690593, -193.5000000000000000, -42.87565520599202529 ) ) ;
#5161 = CARTESIAN_POINT ( 'NONE',  ( -47.78257572244586271, -175.3837268820161057, 0.7175072570443418174 ) ) ;
#5162 = EDGE_CURVE ( 'NONE', #13423, #2282, #11044, .T. ) ;
#5163 = CARTESIAN_POINT ( 'NONE',  ( -48.47912675150885065, -177.1207230881787780, 6.938893903907228378E-15 ) ) ;
#5164 = CARTESIAN_POINT ( 'NONE',  ( -336.3521761649654422, -179.5993808087905279, -18.46045550523168899 ) ) ;
#5165 = EDGE_LOOP ( 'NONE', ( #21508, #34881, #44394, #32658 ) ) ;
#5166 = CARTESIAN_POINT ( 'NONE',  ( 74.77174840718836890, -193.5000000000000000, 20.83798868929603643 ) ) ;
#5167 = ORIENTED_EDGE ( 'NONE', *, *, #25581, .T. ) ;
#5168 = EDGE_CURVE ( 'NONE', #15221, #12949, #31021, .T. ) ;
#5169 = EDGE_LOOP ( 'NONE', ( #28365, #758, #11382, #15914 ) ) ;
#5170 = CARTESIAN_POINT ( 'NONE',  ( -305.0000000000000568, -146.2946350401741711, -55.50139289590185854 ) ) ;
#5171 =( LENGTH_UNIT ( ) NAMED_UNIT ( * ) SI_UNIT ( .MILLI., .METRE. ) );
#5172 = DIRECTION ( 'NONE',  ( -0.000000000000000000, -0.2393156642875482742, 0.9709418174260544543 ) ) ;
#5173 = ORIENTED_EDGE ( 'NONE', *, *, #14048, .T. ) ;
#5174 = CIRCLE ( 'NONE', #25305, 60.00000000000000000 ) ;
#5175 = CARTESIAN_POINT ( 'NONE',  ( -330.4913330509368166, -67.57827586672146936, 21.74306257088659677 ) ) ;
#5176 = DIRECTION ( 'NONE',  ( -0.9374196611341254481, 0.000000000000000000, 0.3482016354343867026 ) ) ;
#5177 = LINE ( 'NONE', #44849, #32921 ) ;
#5178 = ORIENTED_EDGE ( 'NONE', *, *, #1586, .F. ) ;
#5179 = DIRECTION ( 'NONE',  ( 1.000000000000000000, -0.000000000000000000, -0.000000000000000000 ) ) ;
#5180 = VECTOR ( 'NONE', #422, 1000.000000000000114 ) ;
#5181 = FACE_OUTER_BOUND ( 'NONE', #49947, .T. ) ;
#5182 = VECTOR ( 'NONE', #23344, 1000.000000000000000 ) ;
#5183 = CARTESIAN_POINT ( 'NONE',  ( 61.98524708613674505, -193.5000000000000000, 56.33604425924832526 ) ) ;
#5184 = FACE_BOUND ( 'NONE', #9444, .T. ) ;
#5185 = ORIENTED_EDGE ( 'NONE', *, *, #7290, .T. ) ;
#5186 = CARTESIAN_POINT ( 'NONE',  ( 76.01188277843579044, -175.3837268820161057, 11.26891947860284482 ) ) ;
#5187 = ORIENTED_EDGE ( 'NONE', *, *, #8035, .F. ) ;
#5188 = CARTESIAN_POINT ( 'NONE',  ( 28.02885774092381865, -175.3837268820161057, 98.85104101073331151 ) ) ;
#5189 = ORIENTED_EDGE ( 'NONE', *, *, #626, .F. ) ;
#5190 = DIRECTION ( 'NONE',  ( 0.000000000000000000, 0.8229838658936633466, 0.5680647467311457088 ) ) ;
#5191 = ORIENTED_EDGE ( 'NONE', *, *, #32233, .F. ) ;
#5192 = VECTOR ( 'NONE', #375, 1000.000000000000000 ) ;
#5193 = DIRECTION ( 'NONE',  ( -0.8757349421956412971, 0.000000000000000000, 0.4827922027307366970 ) ) ;
#5194 = VECTOR ( 'NONE', #34847, 1000.000000000000000 ) ;
#5195 = CARTESIAN_POINT ( 'NONE',  ( -332.3517673607765914, -73.44864141332200802, 31.34948880313848107 ) ) ;
#5197 = ORIENTED_EDGE ( 'NONE', *, *, #34887, .T. ) ;
#5196 = DIRECTION ( 'NONE',  ( 0.000000000000000000, 1.000000000000000000, 0.000000000000000000 ) ) ;
#5198 = ADVANCED_FACE ( 'NONE', ( #47067 ), #27073, .T. ) ;
#5199 = EDGE_CURVE ( 'NONE', #4116, #16039, #30718, .T. ) ;
#5200 = CARTESIAN_POINT ( 'NONE',  ( -332.3517673607765914, -180.1556192733800117, 16.67542351306693149 ) ) ;
#5201 = VERTEX_POINT ( 'NONE', #15262 ) ;
#5202 = VERTEX_POINT ( 'NONE', #47327 ) ;
#5203 = ORIENTED_EDGE ( 'NONE', *, *, #22179, .F. ) ;
#5204 = APPLICATION_CONTEXT ( 'automotive_design' ) ;
#5205 = DIRECTION ( 'NONE',  ( 0.000000000000000000, 0.000000000000000000, 1.000000000000000000 ) ) ;
#5206 = LINE ( 'NONE', #735, #33567 ) ;
#5207 = EDGE_LOOP ( 'NONE', ( #18500, #49859, #9155, #27760 ) ) ;
#5208 = FACE_OUTER_BOUND ( 'NONE', #6742, .T. ) ;
#5209 = LINE ( 'NONE', #19465, #21120 ) ;
#5210 = LINE ( 'NONE', #33574, #49032 ) ;
#5211 = CIRCLE ( 'NONE', #51389, 125.0000000000000000 ) ;
#5212 = ORIENTED_EDGE ( 'NONE', *, *, #7324, .F. ) ;
#5213 = VECTOR ( 'NONE', #38448, 1000.000000000000000 ) ;
#5214 = VECTOR ( 'NONE', #33926, 1000.000000000000114 ) ;
#5215 = LINE ( 'NONE', #4957, #51948 ) ;
#5216 = LINE ( 'NONE', #52014, #34867 ) ;
#5217 = VERTEX_POINT ( 'NONE', #42850 ) ;
#5220 = ORIENTED_EDGE ( 'NONE', *, *, #7819, .T. ) ;
#5219 = DIRECTION ( 'NONE',  ( 1.043714542225393697E-14, -0.2393156642875516604, 0.9709418174260535661 ) ) ;
#5218 = LINE ( 'NONE', #32797, #29886 ) ;
#5221 = EDGE_LOOP ( 'NONE', ( #40776, #24432, #19603, #46434 ) ) ;
#5222 = ADVANCED_FACE ( 'NONE', ( #27337 ), #22887, .F. ) ;
#5223 = DIRECTION ( 'NONE',  ( 0.000000000000000000, 0.000000000000000000, -1.000000000000000000 ) ) ;
#5224 = ORIENTED_EDGE ( 'NONE', *, *, #5328, .T. ) ;
#5225 = PLANE ( 'NONE',  #49132 ) ;
#5226 = ORIENTED_EDGE ( 'NONE', *, *, #9874, .F. ) ;
#5227 = DIRECTION ( 'NONE',  ( -0.000000000000000000, 1.000000000000000000, -0.000000000000000000 ) ) ;
#5228 = FACE_OUTER_BOUND ( 'NONE', #31964, .T. ) ;
#5229 = ORIENTED_EDGE ( 'NONE', *, *, #31741, .F. ) ;
#5230 = PLANE ( 'NONE',  #9884 ) ;
#5231 = ORIENTED_EDGE ( 'NONE', *, *, #33191, .T. ) ;
#5232 = AXIS2_PLACEMENT_3D ( 'NONE', #20289, #839, #28944 ) ;
#5233 = EDGE_CURVE ( 'NONE', #43120, #38762, #11934, .T. ) ;
#5234 = ORIENTED_EDGE ( 'NONE', *, *, #20200, .F. ) ;
#5235 = DIRECTION ( 'NONE',  ( 0.000000000000000000, 0.000000000000000000, 1.000000000000000000 ) ) ;
#5236 = VECTOR ( 'NONE', #17591, 1000.000000000000114 ) ;
#5238 = CIRCLE ( 'NONE', #36266, 125.0000000000000000 ) ;
#5237 = CARTESIAN_POINT ( 'NONE',  ( -8.721998590732173540, -183.6283474603465606, -118.5089480183145128 ) ) ;
#5239 = CARTESIAN_POINT ( 'NONE',  ( 30.05499637021958392, -177.1207230881787780, -97.24912084693205827 ) ) ;
#5240 = DIRECTION ( 'NONE',  ( 0.000000000000000000, 0.000000000000000000, 1.000000000000000000 ) ) ;
#5241 = ORIENTED_EDGE ( 'NONE', *, *, #50570, .F. ) ;
#5242 = DIRECTION ( 'NONE',  ( 0.000000000000000000, -1.000000000000000000, -0.000000000000000000 ) ) ;
#5243 = APPLICATION_PROTOCOL_DEFINITION ( 'draft international standard', 'automotive_design', 1998, #21312 ) ;
#5244 = CARTESIAN_POINT ( 'NONE',  ( -336.3521761649654422, -123.5000000000000284, 0.000000000000000000 ) ) ;
#5245 = DIRECTION ( 'NONE',  ( 0.000000000000000000, 0.000000000000000000, 1.000000000000000000 ) ) ;
#5246 = DIRECTION ( 'NONE',  ( 1.000000000000000000, 0.000000000000000000, -0.000000000000000000 ) ) ;
#5247 = LINE ( 'NONE', #25721, #43299 ) ;
#5248 = LINE ( 'NONE', #1280, #11450 ) ;
#5249 = VERTEX_POINT ( 'NONE', #32438 ) ;
#5250 = EDGE_LOOP ( 'NONE', ( #33276, #26247, #50368, #36390 ) ) ;
#5251 = DIRECTION ( 'NONE',  ( 0.000000000000000000, -0.9927088740980553050, -0.1205366802553130001 ) ) ;
#5252 = CARTESIAN_POINT ( 'NONE',  ( -213.8817838414232426, -193.5000000000000000, 10.00000000000002842 ) ) ;
#5253 = ORIENTED_EDGE ( 'NONE', *, *, #37515, .T. ) ;
#5254 = ORIENTED_EDGE ( 'NONE', *, *, #20417, .F. ) ;
#5255 = ORIENTED_EDGE ( 'NONE', *, *, #7025, .T. ) ;
#5256 = AXIS2_PLACEMENT_3D ( 'NONE', #17671, #32640, #12658 ) ;
#5257 = EDGE_CURVE ( 'NONE', #21902, #30065, #47547, .T. ) ;
#5258 = DIRECTION ( 'NONE',  ( 0.5315839928299667116, 0.000000000000000000, -0.8470055835512242393 ) ) ;
#5259 = LINE ( 'NONE', #4732, #22004 ) ;
#5260 = FACE_OUTER_BOUND ( 'NONE', #16892, .T. ) ;
#5261 = DIRECTION ( 'NONE',  ( -0.000000000000000000, 0.1205366802553199113, -0.9927088740980544168 ) ) ;
#5262 = ORIENTED_EDGE ( 'NONE', *, *, #51590, .F. ) ;
#5263 = PLANE ( 'NONE',  #49320 ) ;
#5264 = EDGE_CURVE ( 'NONE', #48345, #10459, #24037, .T. ) ;
#5265 = CARTESIAN_POINT ( 'NONE',  ( 3.686287386450715076E-15, 0.000000000000000000, -51.00000000000000711 ) ) ;
#5266 = VECTOR ( 'NONE', #38907, 1000.000000000000000 ) ;
#5267 = CIRCLE ( 'NONE', #34613, 125.0000000000000000 ) ;
#5268 = DIRECTION ( 'NONE',  ( -0.6068001458185945385, 0.000000000000000000, 0.7948544414133523750 ) ) ;
#5269 = VERTEX_POINT ( 'NONE', #48219 ) ;
#5270 = FACE_OUTER_BOUND ( 'NONE', #4332, .T. ) ;
#5271 = AXIS2_PLACEMENT_3D ( 'NONE', #30114, #21720, #42185 ) ;
#5272 = EDGE_CURVE ( 'NONE', #49114, #27618, #4783, .T. ) ;
#5273 = CIRCLE ( 'NONE', #34619, 125.0000000000000000 ) ;
#5274 = ORIENTED_EDGE ( 'NONE', *, *, #21158, .F. ) ;
#5275 = CARTESIAN_POINT ( 'NONE',  ( -145.4373324222574126, -193.5000000000000000, -78.89300572996837957 ) ) ;
#5276 = ORIENTED_EDGE ( 'NONE', *, *, #36574, .T. ) ;
#5277 =( LENGTH_UNIT ( ) NAMED_UNIT ( * ) SI_UNIT ( .MILLI., .METRE. ) );
#5278 = PLANE ( 'NONE',  #23544 ) ;
#5279 = ORIENTED_EDGE ( 'NONE', *, *, #28788, .T. ) ;
#5282 = ORIENTED_EDGE ( 'NONE', *, *, #15225, .T. ) ;
#5281 = DIRECTION ( 'NONE',  ( 0.000000000000000000, 0.000000000000000000, -1.000000000000000000 ) ) ;
#5280 = CARTESIAN_POINT ( 'NONE',  ( -336.3521761649654422, -176.9651911376907094, -25.08789112700655721 ) ) ;
#5283 = ADVANCED_FACE ( 'NONE', ( #8266 ), #5115, .T. ) ;
#5284 = DIRECTION ( 'NONE',  ( 0.000000000000000000, 0.8854560256532141294, 0.4647231720437604574 ) ) ;
#5285 = VERTEX_POINT ( 'NONE', #4075 ) ;
#5286 = CARTESIAN_POINT ( 'NONE',  ( -152.8876895714563773, -189.7472609257535510, 66.89437584437912676 ) ) ;
#5287 = AXIS2_PLACEMENT_3D ( 'NONE', #21960, #26408, #22496 ) ;
#5288 = CARTESIAN_POINT ( 'NONE',  ( -149.3265790242249125, -193.5000000000000000, 72.15117186584558340 ) ) ;
#5289 = ORIENTED_EDGE ( 'NONE', *, *, #47163, .T. ) ;
#5290 = CARTESIAN_POINT ( 'NONE',  ( -160.0000000000000284, -123.5000000000000284, 37.63467731922665394 ) ) ;
#5293 = ORIENTED_EDGE ( 'NONE', *, *, #31357, .T. ) ;
#5292 = CARTESIAN_POINT ( 'NONE',  ( -129.3001299485802633, -189.7472609257535510, -94.04236105995799733 ) ) ;
#5291 = LINE ( 'NONE', #49173, #50959 ) ;
#5294 = ORIENTED_EDGE ( 'NONE', *, *, #4156, .T. ) ;
#5295 = AXIS2_PLACEMENT_3D ( 'NONE', #32308, #3678, #47329 ) ;
#5296 = CARTESIAN_POINT ( 'NONE',  ( 27.50603775690334274, -189.7472609257535510, -99.25348746834811209 ) ) ;
#5297 = DIRECTION ( 'NONE',  ( 0.000000000000000000, 0.000000000000000000, 1.000000000000000000 ) ) ;
#5298 = DIRECTION ( 'NONE',  ( -0.000000000000000000, -1.000000000000000000, 0.000000000000000000 ) ) ;
#5299 = EDGE_LOOP ( 'NONE', ( #8382, #39030, #44092, #3263 ) ) ;
#5300 = DIRECTION ( 'NONE',  ( -0.9960498426152171181, 0.000000000000000000, 0.08879589532293157006 ) ) ;
#5301 = CARTESIAN_POINT ( 'NONE',  ( -94.25732089370191602, -183.6283474603465606, 116.3157639405754935 ) ) ;
#5302 = FACE_OUTER_BOUND ( 'NONE', #28951, .T. ) ;
#5303 = EDGE_LOOP ( 'NONE', ( #23409, #19625, #6002, #41668 ) ) ;
#5304 = AXIS2_PLACEMENT_3D ( 'NONE', #26809, #27589, #15007 ) ;
#5305 = CARTESIAN_POINT ( 'NONE',  ( -149.9407190013152160, -175.3837268820161057, -73.01058346660458653 ) ) ;
#5306 = VECTOR ( 'NONE', #45460, 999.9999999999998863 ) ;
#5307 = DIRECTION ( 'NONE',  ( -0.000000000000000000, 1.000000000000000000, -0.000000000000000000 ) ) ;
#5308 = LINE ( 'NONE', #8711, #34163 ) ;
#5309 = ORIENTED_EDGE ( 'NONE', *, *, #48392, .F. ) ;
#5310 = VECTOR ( 'NONE', #4793, 1000.000000000000114 ) ;
#5311 = DIRECTION ( 'NONE',  ( 0.000000000000000000, 0.9350162426854157216, 0.3546048870425330679 ) ) ;
#5312 = CARTESIAN_POINT ( 'NONE',  ( -47.55243714407701816, -193.5000000000000000, -0.3758275821142288420 ) ) ;
#5313 = CARTESIAN_POINT ( 'NONE',  ( 42.96730897722186171, 30.00000000000000355, -41.16782622478179832 ) ) ;
#5314 = EDGE_CURVE ( 'NONE', #26602, #39066, #8773, .T. ) ;
#5315 = CARTESIAN_POINT ( 'NONE',  ( -330.4913330509368166, -90.39567187580871632, -48.84008046109136814 ) ) ;
#5316 = CIRCLE ( 'NONE', #20407, 60.00000000000000000 ) ;
#5317 = DIRECTION ( 'NONE',  ( 0.000000000000000000, -1.000000000000000000, -0.000000000000000000 ) ) ;
#5318 = EDGE_CURVE ( 'NONE', #47080, #28486, #44526, .T. ) ;
#5319 = CARTESIAN_POINT ( 'NONE',  ( 46.00000000000000711, -42.50000000000000000, -41.00000000000000000 ) ) ;
#5320 = DIRECTION ( 'NONE',  ( -1.000000000000000000, 0.000000000000000000, 0.000000000000000000 ) ) ;
#5322 = ORIENTED_EDGE ( 'NONE', *, *, #31274, .T. ) ;
#5321 = PLANE ( 'NONE',  #31229 ) ;
#5323 = VECTOR ( 'NONE', #29453, 1000.000000000000000 ) ;
#5324 = EDGE_LOOP ( 'NONE', ( #6168, #51958, #1138, #12611 ) ) ;
#5325 = LINE ( 'NONE', #9775, #25753 ) ;
#5326 = ADVANCED_FACE ( 'NONE', ( #24814 ), #40830, .T. ) ;
#5327 = EDGE_CURVE ( 'NONE', #41796, #265, #4581, .T. ) ;
#5328 = EDGE_CURVE ( 'NONE', #13273, #42367, #22369, .T. ) ;
#5329 = AXIS2_PLACEMENT_3D ( 'NONE', #33932, #40778, #1367 ) ;
#5330 = PLANE ( 'NONE',  #36364 ) ;
#5332 = ORIENTED_EDGE ( 'NONE', *, *, #2505, .T. ) ;
#5331 = CARTESIAN_POINT ( 'NONE',  ( -30.31202594373736403, -183.6283474603465606, -123.6727797384705951 ) ) ;
#5333 = VERTEX_POINT ( 'NONE', #24296 ) ;
#5334 = EDGE_CURVE ( 'NONE', #50561, #45007, #21125, .T. ) ;
#5335 = EDGE_LOOP ( 'NONE', ( #36991, #42920, #19832, #29285 ) ) ;
#5336 = CARTESIAN_POINT ( 'NONE',  ( -47.48307690889363641, -175.3837268820161057, 0.08879589532294547560 ) ) ;
#5337 = CARTESIAN_POINT ( 'NONE',  ( -339.1964088526558498, -178.8432607619609485, -20.45418021416653076 ) ) ;
#5338 = DIRECTION ( 'NONE',  ( 0.000000000000000000, 1.000000000000000000, 0.000000000000000000 ) ) ;
#5339 = ORIENTED_EDGE ( 'NONE', *, *, #20842, .F. ) ;
#5340 = CARTESIAN_POINT ( 'NONE',  ( -339.1964088526558498, -123.5000000000000284, 0.000000000000000000 ) ) ;
#5342 = ORIENTED_EDGE ( 'NONE', *, *, #36627, .T. ) ;
#5341 = LINE ( 'NONE', #37117, #50980 ) ;
#5343 = AXIS2_PLACEMENT_3D ( 'NONE', #35132, #51439, #3074 ) ;
#5344 = LINE ( 'NONE', #6123, #5449 ) ;
#5345 = ORIENTED_EDGE ( 'NONE', *, *, #24348, .F. ) ;
#5346 = CARTESIAN_POINT ( 'NONE',  ( -48.47912675150885065, -183.6283474603465606, 6.938893903907228378E-15 ) ) ;
#5347 = ORIENTED_EDGE ( 'NONE', *, *, #41312, .T. ) ;
#5348 = CARTESIAN_POINT ( 'NONE',  ( -330.4913330509368166, -115.7716958700747085, 59.50019592636128607 ) ) ;
#5349 = DIRECTION ( 'NONE',  ( 0.000000000000000000, 0.000000000000000000, 1.000000000000000000 ) ) ;
#5350 = DIRECTION ( 'NONE',  ( 0.000000000000000000, 0.4647231720437789981, 0.8854560256532044704 ) ) ;
#5351 = ORIENTED_EDGE ( 'NONE', *, *, #43170, .F. ) ;
#5352 = ORIENTED_EDGE ( 'NONE', *, *, #51010, .T. ) ;
#5353 = DIRECTION ( 'NONE',  ( 0.000000000000000000, -1.000000000000000000, 0.000000000000000000 ) ) ;
#5354 = CARTESIAN_POINT ( 'NONE',  ( 43.18784210722336780, -175.3837268820161057, -84.98333260264752198 ) ) ;
#5355 = VERTEX_POINT ( 'NONE', #4859 ) ;
#5356 = DIRECTION ( 'NONE',  ( -1.000000000000000000, 0.000000000000000000, 0.000000000000000000 ) ) ;
#5357 = AXIS2_PLACEMENT_3D ( 'NONE', #21003, #5246, #1549 ) ;
#5358 = EDGE_LOOP ( 'NONE', ( #20860, #24051, #4052, #2729 ) ) ;
#5359 = FACE_BOUND ( 'NONE', #39863, .T. ) ;
#5361 = VECTOR ( 'NONE', #10453, 1000.000000000000000 ) ;
#5360 = CARTESIAN_POINT ( 'NONE',  ( -336.3521761649654422, -140.1754235130667610, -56.65561927338005432 ) ) ;
#5362 = EDGE_LOOP ( 'NONE', ( #20699, #6750, #37266, #13609 ) ) ;
#5363 = DIRECTION ( 'NONE',  ( 0.000000000000000000, 0.000000000000000000, 1.000000000000000000 ) ) ;
#5364 = EDGE_LOOP ( 'NONE', ( #44418, #14828, #27757, #36654 ) ) ;
#5365 = LINE ( 'NONE', #21382, #11134 ) ;
#5366 = PLANE ( 'NONE',  #20302 ) ;
#5367 = ORIENTED_EDGE ( 'NONE', *, *, #45780, .F. ) ;
#5368 = ADVANCED_FACE ( 'NONE', ( #16936 ), #32695, .T. ) ;
#5369 = FACE_OUTER_BOUND ( 'NONE', #39839, .T. ) ;
#5370 = ADVANCED_FACE ( 'NONE', ( #40305 ), #36373, .F. ) ;
#5371 = CARTESIAN_POINT ( 'NONE',  ( -121.1142239062970418, -177.1207230881787780, 101.7307360698549132 ) ) ;
#5372 = DIRECTION ( 'NONE',  ( 0.000000000000000000, 0.000000000000000000, -1.000000000000000000 ) ) ;
#5373 = EDGE_CURVE ( 'NONE', #49836, #42173, #32943, .T. ) ;
#5374 = AXIS2_PLACEMENT_3D ( 'NONE', #13726, #45793, #9789 ) ;
#5375 = PLANE ( 'NONE',  #42542 ) ;
#5376 = VERTEX_POINT ( 'NONE', #44004 ) ;
#5377 = FACE_OUTER_BOUND ( 'NONE', #10324, .T. ) ;
#5378 = EDGE_LOOP ( 'NONE', ( #34765, #47494, #37205, #48118 ) ) ;
#5379 = ORIENTED_EDGE ( 'NONE', *, *, #33037, .F. ) ;
#5380 = CARTESIAN_POINT ( 'NONE',  ( 67.04262753014327814, -175.3837268820161057, -47.74645837849745078 ) ) ;
#5382 = ORIENTED_EDGE ( 'NONE', *, *, #23427, .F. ) ;
#5381 = LINE ( 'NONE', #50311, #38771 ) ;
#5383 = ADVANCED_FACE ( 'NONE', ( #48996 ), #12972, .F. ) ;
#5384 = EDGE_LOOP ( 'NONE', ( #26424, #5498, #21444, #49488 ) ) ;
#5385 = DIRECTION ( 'NONE',  ( 0.000000000000000000, 1.000000000000000000, 0.000000000000000000 ) ) ;
#5386 = ADVANCED_FACE ( 'NONE', ( #15908 ), #1683, .T. ) ;
#5387 = ADVANCED_FACE ( 'NONE', ( #26101 ), #33213, .T. ) ;
#5388 = DIRECTION ( 'NONE',  ( -1.000000000000000000, 0.000000000000000000, 0.000000000000000000 ) ) ;
#5389 = ORIENTED_EDGE ( 'NONE', *, *, #23139, .T. ) ;
#5390 = ADVANCED_FACE ( 'NONE', ( #9562 ), #29779, .F. ) ;
#5391 = DIRECTION ( 'NONE',  ( 0.9473263538541923934, 0.000000000000000000, -0.3202698538628350744 ) ) ;
#5392 = EDGE_LOOP ( 'NONE', ( #3816, #46775, #46312, #36724 ) ) ;
#5393 = LINE ( 'NONE', #16961, #2358 ) ;
#5394 = LINE ( 'NONE', #45600, #34231 ) ;
#5395 = AXIS2_PLACEMENT_3D ( 'NONE', #8840, #8578, #24611 ) ;
#5396 = EDGE_CURVE ( 'NONE', #35024, #19199, #37937, .T. ) ;
#5397 = CIRCLE ( 'NONE', #31405, 125.0000000000000000 ) ;
#5398 = CARTESIAN_POINT ( 'NONE',  ( -339.1964088526558498, -138.1050951016792681, -57.16590939599323917 ) ) ;
#5399 = PLANE ( 'NONE',  #35810 ) ;
#5400 = ORIENTED_EDGE ( 'NONE', *, *, #11730, .T. ) ;
#5401 = ORIENTED_EDGE ( 'NONE', *, *, #12187, .F. ) ;
#5402 = VECTOR ( 'NONE', #24607, 1000.000000000000000 ) ;
#5403 = EDGE_LOOP ( 'NONE', ( #696, #1538, #13803, #32807 ) ) ;
#5404 = PLANE ( 'NONE',  #47600 ) ;
#5405 = FACE_OUTER_BOUND ( 'NONE', #51753, .T. ) ;
#5406 = DIRECTION ( 'NONE',  ( 0.000000000000000000, -1.000000000000000000, 0.000000000000000000 ) ) ;
#5407 = DIRECTION ( 'NONE',  ( 0.000000000000000000, 0.000000000000000000, 1.000000000000000000 ) ) ;
#5408 = EDGE_LOOP ( 'NONE', ( #22235, #33553, #31997, #33040 ) ) ;
#5409 = UNCERTAINTY_MEASURE_WITH_UNIT (LENGTH_MEASURE( 1.000000000000000082E-05 ), #30388, 'distance_accuracy_value', 'NONE');
#5410 = AXIS2_PLACEMENT_3D ( 'NONE', #45356, #45104, #17229 ) ;
#5411 = EDGE_CURVE ( 'NONE', #43356, #50666, #49781, .T. ) ;
#5412 = VERTEX_POINT ( 'NONE', #18235 ) ;
#5414 = ORIENTED_EDGE ( 'NONE', *, *, #50955, .F. ) ;
#5413 = FACE_OUTER_BOUND ( 'NONE', #12856, .T. ) ;
#5415 = DIRECTION ( 'NONE',  ( 0.000000000000000000, 0.000000000000000000, 1.000000000000000000 ) ) ;
#5416 = ORIENTED_EDGE ( 'NONE', *, *, #49738, .T. ) ;
#5417 = LINE ( 'NONE', #37457, #600 ) ;
#5418 = CARTESIAN_POINT ( 'NONE',  ( -114.9600645115007040, -193.5000000000000000, 105.8550183720738573 ) ) ;
#5419 = LINE ( 'NONE', #40347, #43101 ) ;
#5420 = FACE_OUTER_BOUND ( 'NONE', #30721, .T. ) ;
#5421 = ORIENTED_EDGE ( 'NONE', *, *, #12784, .F. ) ;
#5422 = LINE ( 'NONE', #5690, #1509 ) ;
#5423 = ORIENTED_EDGE ( 'NONE', *, *, #8027, .F. ) ;
#5424 = EDGE_CURVE ( 'NONE', #23290, #43364, #45832, .T. ) ;
#5425 = ORIENTED_EDGE ( 'NONE', *, *, #41298, .T. ) ;
#5426 = CYLINDRICAL_SURFACE ( 'NONE', #4448, 124.9999999999999858 ) ;
#5427 = CARTESIAN_POINT ( 'NONE',  ( -332.3517673607765914, -179.5993808087905279, -18.46045550523168899 ) ) ;
#5428 = EDGE_LOOP ( 'NONE', ( #8463, #44744, #29369, #10462 ) ) ;
#5429 = AXIS2_PLACEMENT_3D ( 'NONE', #37844, #48655, #17384 ) ;
#5430 = AXIS2_PLACEMENT_3D ( 'NONE', #16273, #44126, #12051 ) ;
#5431 = EDGE_CURVE ( 'NONE', #28470, #44354, #1145, .T. ) ;
#5432 = EDGE_CURVE ( 'NONE', #13401, #43754, #25580, .T. ) ;
#5433 = DIRECTION ( 'NONE',  ( -0.000000000000000000, 1.000000000000000000, -0.000000000000000000 ) ) ;
#5434 = EDGE_CURVE ( 'NONE', #43746, #8800, #49261, .T. ) ;
#5435 = DIRECTION ( 'NONE',  ( -0.000000000000000000, -0.9927088740980544168, -0.1205366802553199251 ) ) ;
#5436 = FACE_OUTER_BOUND ( 'NONE', #36883, .T. ) ;
#5437 = EDGE_CURVE ( 'NONE', #32747, #5648, #13253, .T. ) ;
#5438 = DIRECTION ( 'NONE',  ( 0.000000000000000000, -0.2393156642875582940, -0.9709418174260519008 ) ) ;
#5439 = CIRCLE ( 'NONE', #12116, 125.0000000000000000 ) ;
#5440 = EDGE_CURVE ( 'NONE', #10662, #41535, #38304, .T. ) ;
#5441 = LINE ( 'NONE', #21459, #21098 ) ;
#5442 = LINE ( 'NONE', #21461, #5596 ) ;
#5443 = ORIENTED_EDGE ( 'NONE', *, *, #28532, .T. ) ;
#5444 = EDGE_CURVE ( 'NONE', #8565, #25286, #13509, .T. ) ;
#5445 = FACE_OUTER_BOUND ( 'NONE', #43971, .T. ) ;
#5446 = ORIENTED_EDGE ( 'NONE', *, *, #23615, .T. ) ;
#5447 = FACE_OUTER_BOUND ( 'NONE', #9918, .T. ) ;
#5448 = EDGE_CURVE ( 'NONE', #44462, #31730, #18215, .T. ) ;
#5449 = VECTOR ( 'NONE', #22660, 1000.000000000000000 ) ;
#5450 = ORIENTED_EDGE ( 'NONE', *, *, #16291, .F. ) ;
#5451 = EDGE_CURVE ( 'NONE', #11371, #27267, #50300, .T. ) ;
#5452 = CARTESIAN_POINT ( 'NONE',  ( -332.3517673607765914, -174.9833430614318388, 28.86398714850502856 ) ) ;
#5453 = ADVANCED_FACE ( 'NONE', ( #14291 ), #21915, .F. ) ;
#5454 = CARTESIAN_POINT ( 'NONE',  ( -29.73468717939733352, -183.6283474603465606, 123.5865930638411214 ) ) ;
#5456 = ORIENTED_EDGE ( 'NONE', *, *, #9300, .F. ) ;
#5455 = CARTESIAN_POINT ( 'NONE',  ( -49.40581635894068313, -175.3837268820161057, -0.3758275821142418316 ) ) ;
#5457 = ADVANCED_FACE ( 'NONE', ( #46355 ), #10339, .F. ) ;
#5458 = DIRECTION ( 'NONE',  ( 0.000000000000000000, 0.000000000000000000, 1.000000000000000000 ) ) ;
#5459 = EDGE_LOOP ( 'NONE', ( #5048, #9096, #35272, #33423 ) ) ;
#5460 = EDGE_LOOP ( 'NONE', ( #39614, #21710, #49628, #19288 ) ) ;
#5461 = ADVANCED_FACE ( 'NONE', ( #37684 ), #17977, .F. ) ;
#5462 = VERTEX_POINT ( 'NONE', #5898 ) ;
#5463 = DIRECTION ( 'NONE',  ( 0.000000000000000000, 0.000000000000000000, 1.000000000000000000 ) ) ;
#5464 = DIRECTION ( 'NONE',  ( -0.000000000000000000, 1.000000000000000000, -0.000000000000000000 ) ) ;
#5465 = AXIS2_PLACEMENT_3D ( 'NONE', #39585, #12448, #40817 ) ;
#5466 = ORIENTED_EDGE ( 'NONE', *, *, #14048, .F. ) ;
#5467 = DIRECTION ( 'NONE',  ( 1.000000000000000000, 0.000000000000000000, 0.000000000000000000 ) ) ;
#5468 = AXIS2_PLACEMENT_3D ( 'NONE', #47416, #41727, #46923 ) ;
#5469 = CARTESIAN_POINT ( 'NONE',  ( -5.732832253866456007, -189.7472609257535510, -117.4638425504666657 ) ) ;
#5470 = DIRECTION ( 'NONE',  ( 0.000000000000000000, -1.000000000000000000, 0.000000000000000000 ) ) ;
#5471 = ORIENTED_EDGE ( 'NONE', *, *, #18589, .F. ) ;
#5472 = VECTOR ( 'NONE', #45970, 1000.000000000000000 ) ;
#5473 = EDGE_CURVE ( 'NONE', #15110, #25409, #11631, .T. ) ;
#5474 = VECTOR ( 'NONE', #23585, 1000.000000000000000 ) ;
#5475 = EDGE_CURVE ( 'NONE', #12908, #49029, #23467, .T. ) ;
#5476 = LINE ( 'NONE', #49364, #25652 ) ;
#5477 = ORIENTED_EDGE ( 'NONE', *, *, #14101, .T. ) ;
#5479 = VERTEX_POINT ( 'NONE', #14815 ) ;
#5478 = CARTESIAN_POINT ( 'NONE',  ( -490.0000000000001137, -78.50000000000002842, 0.000000000000000000 ) ) ;
#5480 = ORIENTED_EDGE ( 'NONE', *, *, #42728, .F. ) ;
#5481 = VECTOR ( 'NONE', #50711, 1000.000000000000000 ) ;
#5482 = EDGE_LOOP ( 'NONE', ( #32676, #1742, #46403, #31873 ) ) ;
#5483 = CARTESIAN_POINT ( 'NONE',  ( 52.98246549829696050, -189.7472609257535510, 73.01058346660535392 ) ) ;
#5484 = FACE_OUTER_BOUND ( 'NONE', #38565, .T. ) ;
#5485 = CIRCLE ( 'NONE', #16387, 20.00000000000000000 ) ;
#5486 = ORIENTED_EDGE ( 'NONE', *, *, #50907, .F. ) ;
#5487 = DIRECTION ( 'NONE',  ( 1.043714542225393223E-14, 0.9709418174260544543, 0.2393156642875482742 ) ) ;
#5488 = DIRECTION ( 'NONE',  ( 0.000000000000000000, -1.000000000000000000, 0.000000000000000000 ) ) ;
#5489 = ORIENTED_EDGE ( 'NONE', *, *, #8679, .T. ) ;
#5490 = PLANE ( 'NONE',  #32571 ) ;
#5491 = AXIS2_PLACEMENT_3D ( 'NONE', #40733, #37060, #40218 ) ;
#5492 = VERTEX_POINT ( 'NONE', #38955 ) ;
#5493 = ORIENTED_EDGE ( 'NONE', *, *, #26912, .F. ) ;
#5494 = CARTESIAN_POINT ( 'NONE',  ( 71.15591247552653442, -193.5000000000000000, 36.22785377504035154 ) ) ;
#5495 = DIRECTION ( 'NONE',  ( 0.000000000000000000, 0.000000000000000000, 1.000000000000000000 ) ) ;
#5496 = DIRECTION ( 'NONE',  ( -0.000000000000000000, 1.000000000000000000, -0.000000000000000000 ) ) ;
#5497 = DIRECTION ( 'NONE',  ( 0.000000000000000000, 0.000000000000000000, -1.000000000000000000 ) ) ;
#5498 = ORIENTED_EDGE ( 'NONE', *, *, #14342, .F. ) ;
#5499 = DIRECTION ( 'NONE',  ( 0.000000000000000000, 0.000000000000000000, 1.000000000000000000 ) ) ;
#5500 = DIRECTION ( 'NONE',  ( -0.000000000000000000, 1.000000000000000000, -0.000000000000000000 ) ) ;
#5501 = ADVANCED_FACE ( 'NONE', ( #10859 ), #23212, .T. ) ;
#5502 = EDGE_CURVE ( 'NONE', #45026, #10698, #39229, .T. ) ;
#5503 = FACE_OUTER_BOUND ( 'NONE', #30435, .T. ) ;
#5504 = DIRECTION ( 'NONE',  ( -0.5338233779648003940, 0.000000000000000000, 0.8455960035018199594 ) ) ;
#5505 = ORIENTED_EDGE ( 'NONE', *, *, #16880, .T. ) ;
#5506 = CARTESIAN_POINT ( 'NONE',  ( 0.000000000000000000, -116.3883358649361526, -58.56982357178523557 ) ) ;
#5507 = LINE ( 'NONE', #5774, #21471 ) ;
#5508 = EDGE_CURVE ( 'NONE', #5830, #32508, #3237, .T. ) ;
#5509 = DIRECTION ( 'NONE',  ( 0.000000000000000000, 0.000000000000000000, 1.000000000000000000 ) ) ;
#5510 = ORIENTED_EDGE ( 'NONE', *, *, #9989, .T. ) ;
#5511 = CIRCLE ( 'NONE', #1282, 125.0000000000000000 ) ;
#5512 = VECTOR ( 'NONE', #2943, 1000.000000000000000 ) ;
#5513 = AXIS2_PLACEMENT_3D ( 'NONE', #45265, #17134, #5311 ) ;
#5514 = CARTESIAN_POINT ( 'NONE',  ( -48.47912675150885065, -175.3837268820161057, 6.938893903907228378E-15 ) ) ;
#5515 = DIRECTION ( 'NONE',  ( -0.9027978299657387629, 0.000000000000000000, -0.4300652022765304450 ) ) ;
#5516 = ORIENTED_EDGE ( 'NONE', *, *, #27962, .F. ) ;
#5517 = ORIENTED_EDGE ( 'NONE', *, *, #14542, .T. ) ;
#5518 = ORIENTED_EDGE ( 'NONE', *, *, #1824, .F. ) ;
#5519 = VECTOR ( 'NONE', #35938, 1000.000000000000000 ) ;
#5520 = DIRECTION ( 'NONE',  ( 1.000000000000000000, -0.000000000000000000, -0.000000000000000000 ) ) ;
#5521 = DIRECTION ( 'NONE',  ( 0.5829794791144762289, 0.000000000000000000, -0.8124868780056783146 ) ) ;
#5523 = EDGE_CURVE ( 'NONE', #28004, #41662, #34757, .T. ) ;
#5522 = VECTOR ( 'NONE', #15169, 1000.000000000000114 ) ;
#5524 = FACE_OUTER_BOUND ( 'NONE', #36809, .T. ) ;
#5525 = CARTESIAN_POINT ( 'NONE',  ( -180.0000000000000568, -123.5000000000000284, -37.63467731922663972 ) ) ;
#5526 = VECTOR ( 'NONE', #51236, 1000.000000000000227 ) ;
#5527 = PLANE ( 'NONE',  #44497 ) ;
#5528 = ORIENTED_EDGE ( 'NONE', *, *, #33302, .T. ) ;
#5529 = EDGE_CURVE ( 'NONE', #47477, #47750, #46877, .T. ) ;
#5530 = CARTESIAN_POINT ( 'NONE',  ( 74.60098876342242136, -177.1207230881787780, 21.82395850507348811 ) ) ;
#5531 = VERTEX_POINT ( 'NONE', #26871 ) ;
#5532 = CIRCLE ( 'NONE', #13043, 125.0000000000000000 ) ;
#5533 = PLANE ( 'NONE',  #29241 ) ;
#5534 = ORIENTED_EDGE ( 'NONE', *, *, #35670, .F. ) ;
#5535 = DIRECTION ( 'NONE',  ( 0.000000000000000000, -1.000000000000000000, 0.000000000000000000 ) ) ;
#5536 = ORIENTED_EDGE ( 'NONE', *, *, #41761, .F. ) ;
#5537 = CARTESIAN_POINT ( 'NONE',  ( -48.30223647638627682, -183.6283474603465606, -0.9842305779475897243 ) ) ;
#5538 = ORIENTED_EDGE ( 'NONE', *, *, #3513, .T. ) ;
#5541 = ORIENTED_EDGE ( 'NONE', *, *, #2287, .T. ) ;
#5540 = DIRECTION ( 'NONE',  ( 0.000000000000000000, 0.8229838658936596829, 0.5680647467311510379 ) ) ;
#5539 = FACE_OUTER_BOUND ( 'NONE', #47773, .T. ) ;
#5542 = VECTOR ( 'NONE', #10519, 1000.000000000000000 ) ;
#5543 = DIRECTION ( 'NONE',  ( 0.000000000000000000, -0.4647231720437604574, 0.8854560256532141294 ) ) ;
#5544 = AXIS2_PLACEMENT_3D ( 'NONE', #12581, #25454, #12837 ) ;
#5545 = ORIENTED_EDGE ( 'NONE', *, *, #21761, .T. ) ;
#5546 = DIRECTION ( 'NONE',  ( -0.000000000000000000, 0.9927088740980556381, 0.1205366802553095307 ) ) ;
#5547 = ORIENTED_EDGE ( 'NONE', *, *, #39111, .T. ) ;
#5548 = VECTOR ( 'NONE', #7871, 1000.000000000000000 ) ;
#5549 = CARTESIAN_POINT ( 'NONE',  ( -47.51449116960048968, -183.6283474603465606, 0.2635871660690785045 ) ) ;
#5552 = EDGE_LOOP ( 'NONE', ( #1172, #27171, #17097, #40327 ) ) ;
#5551 = CARTESIAN_POINT ( 'NONE',  ( -48.47912675150885065, -189.7472609257535510, 6.938893903907228378E-15 ) ) ;
#5550 = CARTESIAN_POINT ( 'NONE',  ( -339.1964088526558498, -175.5095439275177398, -27.86139516340860212 ) ) ;
#5553 = ORIENTED_EDGE ( 'NONE', *, *, #49819, .T. ) ;
#5554 = LINE ( 'NONE', #1067, #26549 ) ;
#5555 = LINE ( 'NONE', #41269, #10217 ) ;
#5556 = DIRECTION ( 'NONE',  ( 0.000000000000000000, 0.000000000000000000, -1.000000000000000000 ) ) ;
#5557 = EDGE_LOOP ( 'NONE', ( #36293, #25069, #33914, #15885 ) ) ;
#5558 = VECTOR ( 'NONE', #9093, 1000.000000000000000 ) ;
#5559 = FACE_OUTER_BOUND ( 'NONE', #34033, .T. ) ;
#5560 = CARTESIAN_POINT ( 'NONE',  ( -330.4913330509368166, -172.3400804610915031, -33.10432812419114157 ) ) ;
#5561 = DIRECTION ( 'NONE',  ( 0.000000000000000000, -1.000000000000000000, 0.000000000000000000 ) ) ;
#5562 = VECTOR ( 'NONE', #22502, 1000.000000000000000 ) ;
#5563 = LINE ( 'NONE', #33658, #14853 ) ;
#5564 = ORIENTED_EDGE ( 'NONE', *, *, #8610, .T. ) ;
#5565 = EDGE_CURVE ( 'NONE', #11626, #29097, #37485, .T. ) ;
#5566 = VECTOR ( 'NONE', #14978, 1000.000000000000000 ) ;
#5567 = CARTESIAN_POINT ( 'NONE',  ( -170.0000000000000284, -123.5000000000000284, 37.63467731922665394 ) ) ;
#5568 = LINE ( 'NONE', #9245, #46615 ) ;
#5569 = AXIS2_PLACEMENT_3D ( 'NONE', #4960, #48845, #20979 ) ;
#5570 = FACE_OUTER_BOUND ( 'NONE', #33249, .T. ) ;
#5571 = ORIENTED_EDGE ( 'NONE', *, *, #12162, .F. ) ;
#5572 = CARTESIAN_POINT ( 'NONE',  ( 70.68712318874649725, -177.1207230881787780, -37.74128873232327663 ) ) ;
#5573 = CYLINDRICAL_SURFACE ( 'NONE', #4292, 125.0000000000000000 ) ;
#5574 = DIRECTION ( 'NONE',  ( 1.000000000000000000, 7.719741424018471827E-17, -4.051632851310729971E-17 ) ) ;
#5575 = CARTESIAN_POINT ( 'NONE',  ( -48.47912675150885065, -175.3837268820161057, 6.938893903907228378E-15 ) ) ;
#5576 = DIRECTION ( 'NONE',  ( -1.000000000000000000, 5.399917434947259359E-17, 0.000000000000000000 ) ) ;
#5577 = VECTOR ( 'NONE', #46162, 1000.000000000000000 ) ;
#5578 = VECTOR ( 'NONE', #12460, 1000.000000000000000 ) ;
#5579 = DIRECTION ( 'NONE',  ( 0.000000000000000000, 1.000000000000000000, -0.000000000000000000 ) ) ;
#5580 = EDGE_CURVE ( 'NONE', #37674, #51994, #19273, .T. ) ;
#5581 = CARTESIAN_POINT ( 'NONE',  ( -330.4913330509368166, -172.3400804610915031, -33.10432812419114157 ) ) ;
#5583 = ORIENTED_EDGE ( 'NONE', *, *, #7892, .T. ) ;
#5582 = LINE ( 'NONE', #42335, #42944 ) ;
#5584 = CIRCLE ( 'NONE', #34919, 125.0000000000000000 ) ;
#5585 = AXIS2_PLACEMENT_3D ( 'NONE', #22620, #38632, #47052 ) ;
#5586 = VERTEX_POINT ( 'NONE', #43165 ) ;
#5587 = CARTESIAN_POINT ( 'NONE',  ( -172.4422607493951318, -183.6283474603465606, 16.06677968424543579 ) ) ;
#5589 = ORIENTED_EDGE ( 'NONE', *, *, #2595, .T. ) ;
#5588 = CARTESIAN_POINT ( 'NONE',  ( -47.60339180931321579, -175.3837268820161057, 0.4827922027307559594 ) ) ;
#5590 = AXIS2_PLACEMENT_3D ( 'NONE', #45310, #25070, #32681 ) ;
#5591 = EDGE_LOOP ( 'NONE', ( #43211, #45296, #40113, #2197 ) ) ;
#5592 = VECTOR ( 'NONE', #40750, 1000.000000000000000 ) ;
#5593 = ORIENTED_EDGE ( 'NONE', *, *, #21466, .F. ) ;
#5594 = ADVANCED_FACE ( 'NONE', ( #2707 ), #7443, .T. ) ;
#5595 = DIRECTION ( 'NONE',  ( -0.9960498426152165630, 0.000000000000000000, -0.08879589532293852283 ) ) ;
#5596 = VECTOR ( 'NONE', #1487, 1000.000000000000000 ) ;
#5597 = CIRCLE ( 'NONE', #44175, 60.00000000000000000 ) ;
#5598 = EDGE_CURVE ( 'NONE', #12133, #37972, #51327, .T. ) ;
#5599 = DIRECTION ( 'NONE',  ( -0.000000000000000000, -0.000000000000000000, -1.000000000000000000 ) ) ;
#5600 = CARTESIAN_POINT ( 'NONE',  ( -120.2975302769383177, -193.5000000000000000, 102.3089288139533863 ) ) ;
#5601 = VERTEX_POINT ( 'NONE', #18745 ) ;
#5602 = AXIS2_PLACEMENT_3D ( 'NONE', #1908, #18211, #5350 ) ;
#5603 = LINE ( 'NONE', #50772, #13497 ) ;
#5605 = ORIENTED_EDGE ( 'NONE', *, *, #2319, .F. ) ;
#5604 = CARTESIAN_POINT ( 'NONE',  ( -0.6536498292959314060, -177.1207230881787780, 114.4068333132749160 ) ) ;
#5606 = CIRCLE ( 'NONE', #30625, 125.0000000000000000 ) ;
#5607 = DIRECTION ( 'NONE',  ( 0.8124868780056783146, 0.000000000000000000, 0.5829794791144762289 ) ) ;
#5608 = VERTEX_POINT ( 'NONE', #6914 ) ;
#5609 = DIRECTION ( 'NONE',  ( 0.000000000000000000, -0.000000000000000000, 1.000000000000000000 ) ) ;
#5610 = ORIENTED_EDGE ( 'NONE', *, *, #32127, .T. ) ;
#5611 = CARTESIAN_POINT ( 'NONE',  ( -115.4536696835168641, -177.1207230881787780, -105.5434062319793185 ) ) ;
#5612 = CARTESIAN_POINT ( 'NONE',  ( -47.82630463331833681, -193.5000000000000000, 0.7575112421616305713 ) ) ;
#5613 = DIRECTION ( 'NONE',  ( 1.000000000000000000, 0.000000000000000000, 0.000000000000000000 ) ) ;
#5614 = ADVANCED_FACE ( 'NONE', ( #47377 ), #18486, .T. ) ;
#5615 = ORIENTED_EDGE ( 'NONE', *, *, #16077, .T. ) ;
#5616 = CIRCLE ( 'NONE', #34961, 125.0000000000000000 ) ;
#5617 = ORIENTED_EDGE ( 'NONE', *, *, #17319, .F. ) ;
#5618 = LINE ( 'NONE', #18214, #15588 ) ;
#5619 = AXIS2_PLACEMENT_3D ( 'NONE', #28997, #41101, #37152 ) ;
#5620 = DIRECTION ( 'NONE',  ( 0.8757349421956345248, 0.000000000000000000, 0.4827922027307490205 ) ) ;
#5621 = ORIENTED_EDGE ( 'NONE', *, *, #13741, .T. ) ;
#5622 = CARTESIAN_POINT ( 'NONE',  ( 75.32224018181403835, -183.6283474603465606, 7.024906801079482399 ) ) ;
#5623 = VECTOR ( 'NONE', #6841, 1000.000000000000000 ) ;
#5624 = ORIENTED_EDGE ( 'NONE', *, *, #2149, .F. ) ;
#5625 = EDGE_CURVE ( 'NONE', #14548, #37490, #43383, .T. ) ;
#5626 = CARTESIAN_POINT ( 'NONE',  ( -96.30460367372252506, -177.1207230881787780, -114.4068333132746176 ) ) ;
#5627 = EDGE_CURVE ( 'NONE', #34284, #51297, #3477, .T. ) ;
#5628 = DIRECTION ( 'NONE',  ( 0.4792266786073201557, 0.4327645661435911562, -0.7635814434633318992 ) ) ;
#5629 = EDGE_LOOP ( 'NONE', ( #22899, #38030, #37962, #5923, #47415, #25959, #8043, #1488 ) ) ;
#5630 = LINE ( 'NONE', #14022, #24944 ) ;
#5631 = ORIENTED_EDGE ( 'NONE', *, *, #39886, .T. ) ;
#5632 = AXIS2_PLACEMENT_3D ( 'NONE', #44312, #11716, #20637 ) ;
#5633 = EDGE_CURVE ( 'NONE', #25704, #15236, #35029, .T. ) ;
#5634 = CARTESIAN_POINT ( 'NONE',  ( -159.3947744408687868, -177.1207230881787780, -55.44293326708444880 ) ) ;
#5635 = CIRCLE ( 'NONE', #3930, 125.0000000000000000 ) ;
#5636 = DIRECTION ( 'NONE',  ( 0.000000000000000000, 0.000000000000000000, -1.000000000000000000 ) ) ;
#5637 = EDGE_LOOP ( 'NONE', ( #37783, #3398, #18844, #15034 ) ) ;
#5638 = AXIS2_PLACEMENT_3D ( 'NONE', #44247, #12945, #28970 ) ;
#5639 = VECTOR ( 'NONE', #41599, 1000.000000000000114 ) ;
#5640 = LINE ( 'NONE', #24812, #50869 ) ;
#5641 = FACE_OUTER_BOUND ( 'NONE', #4326, .T. ) ;
#5642 = DIRECTION ( 'NONE',  ( 0.000000000000000000, 0.000000000000000000, 1.000000000000000000 ) ) ;
#5643 = CIRCLE ( 'NONE', #22389, 4.999999999999997335 ) ;
#5644 = FACE_OUTER_BOUND ( 'NONE', #37064, .T. ) ;
#5645 = ORIENTED_EDGE ( 'NONE', *, *, #19703, .T. ) ;
#5647 = CIRCLE ( 'NONE', #17391, 9.999999999999994671 ) ;
#5646 = CARTESIAN_POINT ( 'NONE',  ( 10.73478887071927623, -193.5000000000000000, -110.0850225811106924 ) ) ;
#5648 = VERTEX_POINT ( 'NONE', #10597 ) ;
#5649 = EDGE_CURVE ( 'NONE', #27687, #38097, #26629, .T. ) ;
#5650 = CYLINDRICAL_SURFACE ( 'NONE', #44597, 4.999999999999997335 ) ;
#5652 = VERTEX_POINT ( 'NONE', #15578 ) ;
#5651 = CARTESIAN_POINT ( 'NONE',  ( -148.6149069237406195, -177.1207230881787780, -74.81861753132355375 ) ) ;
#5653 = ORIENTED_EDGE ( 'NONE', *, *, #12058, .F. ) ;
#5654 = CARTESIAN_POINT ( 'NONE',  ( -173.0003472773501301, -175.3837268820161057, 10.93003379476953363 ) ) ;
#5655 = LINE ( 'NONE', #49010, #22906 ) ;
#5656 = AXIS2_PLACEMENT_3D ( 'NONE', #2810, #50920, #14922 ) ;
#5657 = VECTOR ( 'NONE', #42595, 1000.000000000000114 ) ;
#5658 = ORIENTED_EDGE ( 'NONE', *, *, #8929, .F. ) ;
#5659 = CARTESIAN_POINT ( 'NONE',  ( 0.000000000000000000, -53.50000000000000000, 0.000000000000000000 ) ) ;
#5660 = ORIENTED_EDGE ( 'NONE', *, *, #44539, .F. ) ;
#5661 = DIRECTION ( 'NONE',  ( 0.000000000000000000, 0.000000000000000000, -1.000000000000000000 ) ) ;
#5662 = LINE ( 'NONE', #30075, #45994 ) ;
#5663 = AXIS2_PLACEMENT_3D ( 'NONE', #33160, #36853, #21078 ) ;
#5664 = LINE ( 'NONE', #37706, #28615 ) ;
#5665 = DIRECTION ( 'NONE',  ( 0.05924062789372142729, 0.000000000000000000, -0.9982437317643209074 ) ) ;
#5666 = ORIENTED_EDGE ( 'NONE', *, *, #26885, .F. ) ;
#5667 = ORIENTED_EDGE ( 'NONE', *, *, #625, .F. ) ;
#5668 = VERTEX_POINT ( 'NONE', #31593 ) ;
#5669 = LINE ( 'NONE', #21690, #51765 ) ;
#5670 = DIRECTION ( 'NONE',  ( -0.08879589532294572540, 0.000000000000000000, 0.9960498426152160079 ) ) ;
#5671 = VECTOR ( 'NONE', #3267, 1000.000000000000000 ) ;
#5672 = VECTOR ( 'NONE', #3335, 1000.000000000000114 ) ;
#5673 = CARTESIAN_POINT ( 'NONE',  ( -150.1390659022305840, -193.5000000000000000, 72.73415134496005408 ) ) ;
#5674 = CARTESIAN_POINT ( 'NONE',  ( -173.4460699164830260, -189.7472609257535510, -2.874563619423225802 ) ) ;
#5675 = VERTEX_POINT ( 'NONE', #47649 ) ;
#5676 = EDGE_CURVE ( 'NONE', #22186, #47386, #40246, .T. ) ;
#5677 = ADVANCED_FACE ( 'NONE', ( #15849 ), #57, .T. ) ;
#5678 = CIRCLE ( 'NONE', #19911, 60.00000000000000000 ) ;
#5679 = VECTOR ( 'NONE', #34224, 1000.000000000000114 ) ;
#5680 = VERTEX_POINT ( 'NONE', #23712 ) ;
#5682 = ORIENTED_EDGE ( 'NONE', *, *, #51445, .F. ) ;
#5681 = CARTESIAN_POINT ( 'NONE',  ( 75.95066919219054569, -189.7472609257535510, -11.92584929509534852 ) ) ;
#5683 = VERTEX_POINT ( 'NONE', #43942 ) ;
#5684 = FACE_OUTER_BOUND ( 'NONE', #24849, .T. ) ;
#5685 = CARTESIAN_POINT ( 'NONE',  ( 46.00000000000000711, 20.00000000000000000, -41.00000000000000000 ) ) ;
#5686 = LINE ( 'NONE', #50088, #17861 ) ;
#5687 = DIRECTION ( 'NONE',  ( 0.000000000000000000, 1.000000000000000000, 0.000000000000000000 ) ) ;
#5688 = EDGE_LOOP ( 'NONE', ( #17704, #42800, #33501, #1995 ) ) ;
#5689 = EDGE_CURVE ( 'NONE', #35564, #17216, #23965, .T. ) ;
#5690 = CARTESIAN_POINT ( 'NONE',  ( 36.10886851198520731, -183.6283474603465606, 92.03190238880812046 ) ) ;
#5691 = EDGE_LOOP ( 'NONE', ( #30462, #46109 ) ) ;
#5692 = EDGE_CURVE ( 'NONE', #28453, #40339, #14849, .T. ) ;
#5693 = ORIENTED_EDGE ( 'NONE', *, *, #44701, .F. ) ;
#5694 = CARTESIAN_POINT ( 'NONE',  ( -260.0000000000000000, -123.5000000000000284, 6.938893903907228378E-15 ) ) ;
#5695 = CIRCLE ( 'NONE', #41770, 60.00000000000000000 ) ;
#5696 = VECTOR ( 'NONE', #7358, 1000.000000000000114 ) ;
#5697 = EDGE_CURVE ( 'NONE', #2241, #4717, #24238, .T. ) ;
#5698 = CARTESIAN_POINT ( 'NONE',  ( -305.0000000000000568, -68.38646289696045244, -23.71704087764493707 ) ) ;
#5699 = EDGE_LOOP ( 'NONE', ( #23017, #27167, #41644, #2043 ) ) ;
#5700 = AXIS2_PLACEMENT_3D ( 'NONE', #48762, #7769, #23797 ) ;
#5701 = EDGE_CURVE ( 'NONE', #37855, #5355, #47897, .T. ) ;
#5702 = CARTESIAN_POINT ( 'NONE',  ( -48.47912675150885065, -189.7472609257535510, 6.938893903907228378E-15 ) ) ;
#5703 = DIRECTION ( 'NONE',  ( 0.000000000000000000, 1.119474883163699554E-13, 1.000000000000000000 ) ) ;
#5704 = FACE_OUTER_BOUND ( 'NONE', #48178, .T. ) ;
#5705 = DIRECTION ( 'NONE',  ( 0.000000000000000000, -0.2393156642875615969, -0.9709418174260511236 ) ) ;
#5706 = DIRECTION ( 'NONE',  ( 0.000000000000000000, 0.000000000000000000, -1.000000000000000000 ) ) ;
#5707 = FACE_BOUND ( 'NONE', #317, .T. ) ;
#5708 = EDGE_LOOP ( 'NONE', ( #4940, #41134, #29638, #12674 ) ) ;
#5709 = VECTOR ( 'NONE', #4341, 1000.000000000000000 ) ;
#5710 = LINE ( 'NONE', #34063, #6333 ) ;
#5711 = ORIENTED_EDGE ( 'NONE', *, *, #27958, .F. ) ;
#5712 = VECTOR ( 'NONE', #3008, 1000.000000000000000 ) ;
#5713 = ORIENTED_EDGE ( 'NONE', *, *, #23669, .T. ) ;
#5714 = CARTESIAN_POINT ( 'NONE',  ( -5.732832253866456007, -193.5000000000000000, -117.4638425504666657 ) ) ;
#5715 = ORIENTED_EDGE ( 'NONE', *, *, #4078, .F. ) ;
#5716 = AXIS2_PLACEMENT_3D ( 'NONE', #32335, #16600, #17116 ) ;
#5717 = CARTESIAN_POINT ( 'NONE',  ( -336.3521761649654422, -171.1288023355047585, 34.85916744524404720 ) ) ;
#5718 = CARTESIAN_POINT ( 'NONE',  ( -49.25565061422690150, -193.5000000000000000, 0.6300878435817109935 ) ) ;
#5720 = ORIENTED_EDGE ( 'NONE', *, *, #6762, .T. ) ;
#5719 = CARTESIAN_POINT ( 'NONE',  ( -139.0630283577175987, -177.1207230881787780, -86.13684908212448477 ) ) ;
#5721 = FACE_OUTER_BOUND ( 'NONE', #49848, .T. ) ;
#5722 = ORIENTED_EDGE ( 'NONE', *, *, #45979, .F. ) ;
#5723 = ORIENTED_EDGE ( 'NONE', *, *, #16135, .F. ) ;
#5724 = VERTEX_POINT ( 'NONE', #12127 ) ;
#5725 = EDGE_CURVE ( 'NONE', #50565, #16442, #32367, .T. ) ;
#5726 = CARTESIAN_POINT ( 'NONE',  ( -166.0019676197264005, -175.3837268820161057, 39.55227055146321646 ) ) ;
#5727 = VECTOR ( 'NONE', #51066, 1000.000000000000000 ) ;
#5728 = CARTESIAN_POINT ( 'NONE',  ( -305.0000000000000568, -67.57827586672146936, 21.74306257088660033 ) ) ;
#5729 = VECTOR ( 'NONE', #40351, 1000.000000000000000 ) ;
#5730 =( NAMED_UNIT ( * ) SI_UNIT ( $, .STERADIAN. ) SOLID_ANGLE_UNIT ( ) );
#5731 = CARTESIAN_POINT ( 'NONE',  ( -173.4190745413846457, -175.3837268820161057, -3.874202661594927211 ) ) ;
#5732 = DIRECTION ( 'NONE',  ( 0.000000000000000000, 1.000000000000000000, -0.000000000000000000 ) ) ;
#5733 = ORIENTED_EDGE ( 'NONE', *, *, #262, .T. ) ;
#5734 = VECTOR ( 'NONE', #41376, 1000.000000000000000 ) ;
#5735 = EDGE_CURVE ( 'NONE', #41896, #2959, #19761, .T. ) ;
#5736 = ADVANCED_FACE ( 'NONE', ( #575 ), #4262, .F. ) ;
#5737 = EDGE_CURVE ( 'NONE', #41712, #26081, #603, .T. ) ;
#5738 = ADVANCED_FACE ( 'NONE', ( #32882 ), #6482, .T. ) ;
#5739 = DIRECTION ( 'NONE',  ( 0.000000000000000000, 0.000000000000000000, -1.000000000000000000 ) ) ;
#5740 = LINE ( 'NONE', #29364, #29014 ) ;
#5741 = ORIENTED_EDGE ( 'NONE', *, *, #911, .F. ) ;
#5743 = EDGE_LOOP ( 'NONE', ( #18146, #6930, #2470, #10476 ) ) ;
#5742 = PLANE ( 'NONE',  #12203 ) ;
#5744 = CIRCLE ( 'NONE', #44340, 125.0000000000000000 ) ;
#5745 = ORIENTED_EDGE ( 'NONE', *, *, #39261, .F. ) ;
#5746 = EDGE_CURVE ( 'NONE', #36146, #21174, #28421, .T. ) ;
#5747 = VERTEX_POINT ( 'NONE', #48155 ) ;
#5748 = DIRECTION ( 'NONE',  ( 0.000000000000000000, 0.000000000000000000, 1.000000000000000000 ) ) ;
#5749 = DIRECTION ( 'NONE',  ( -0.000000000000000000, 0.1205366802553337752, 0.9927088740980526405 ) ) ;
#5750 = VERTEX_POINT ( 'NONE', #36058 ) ;
#5751 = DIRECTION ( 'NONE',  ( 0.000000000000000000, 0.000000000000000000, -1.000000000000000000 ) ) ;
#5752 = CARTESIAN_POINT ( 'NONE',  ( 2.066935079424583765, -175.3837268820161057, -114.3245189510257802 ) ) ;
#5753 = EDGE_LOOP ( 'NONE', ( #7508, #25857, #12183, #41979 ) ) ;
#5754 = EDGE_CURVE ( 'NONE', #12927, #38011, #3954, .T. ) ;
#5755 = DIRECTION ( 'NONE',  ( -0.000000000000000000, 1.000000000000000000, 0.000000000000000000 ) ) ;
#5756 = ORIENTED_EDGE ( 'NONE', *, *, #14737, .F. ) ;
#5757 = EDGE_CURVE ( 'NONE', #11859, #6229, #44470, .T. ) ;
#5758 = VECTOR ( 'NONE', #51241, 1000.000000000000000 ) ;
#5759 = VERTEX_POINT ( 'NONE', #36572 ) ;
#5760 = CARTESIAN_POINT ( 'NONE',  ( -48.13092511607445800, -193.5000000000000000, 0.9374196611341301111 ) ) ;
#5761 = CARTESIAN_POINT ( 'NONE',  ( 46.00000000000000711, 0.000000000000000000, 46.00000000000000000 ) ) ;
#5762 = ADVANCED_FACE ( 'NONE', ( #36844 ), #24484, .F. ) ;
#5763 = LINE ( 'NONE', #28861, #36425 ) ;
#5764 = PLANE ( 'NONE',  #10607 ) ;
#5765 = EDGE_LOOP ( 'NONE', ( #38353, #31103, #4269, #20447 ) ) ;
#5766 = DIRECTION ( 'NONE',  ( -0.4285077258200425399, -0.8746197071393964073, 0.2267630851702541195 ) ) ;
#5767 = DIRECTION ( 'NONE',  ( 0.000000000000000000, 1.000000000000000000, 0.000000000000000000 ) ) ;
#5768 = ADVANCED_FACE ( 'NONE', ( #8207 ), #32636, .F. ) ;
#5769 = ITEM_DEFINED_TRANSFORMATION ( 'NONE', 'NONE', #46920,  #31742 ) ;
#5770 = DIRECTION ( 'NONE',  ( 0.000000000000000000, 0.000000000000000000, 1.000000000000000000 ) ) ;
#5771 = DIRECTION ( 'NONE',  ( -0.000000000000000000, 1.000000000000000000, -0.000000000000000000 ) ) ;
#5772 = ORIENTED_EDGE ( 'NONE', *, *, #19487, .F. ) ;
#5773 = CARTESIAN_POINT ( 'NONE',  ( -48.88225018079680950, -189.7472609257535510, -0.9151456172430169067 ) ) ;
#5774 = CARTESIAN_POINT ( 'NONE',  ( -332.3517673607765914, -139.2044816956407089, -56.89493493766761389 ) ) ;
#5775 = EDGE_CURVE ( 'NONE', #10671, #38308, #45949, .T. ) ;
#5776 = CARTESIAN_POINT ( 'NONE',  ( -169.9131040279660567, -183.6283474603465606, 29.64437826672833864 ) ) ;
#5777 = ORIENTED_EDGE ( 'NONE', *, *, #50348, .F. ) ;
#5778 = AXIS2_PLACEMENT_3D ( 'NONE', #11027, #27055, #35721 ) ;
#5779 = ORIENTED_EDGE ( 'NONE', *, *, #27503, .F. ) ;
#5780 = VECTOR ( 'NONE', #50346, 1000.000000000000000 ) ;
#5781 = VECTOR ( 'NONE', #38082, 1000.000000000000000 ) ;
#5782 = DIRECTION ( 'NONE',  ( 0.9473263538541923934, 0.000000000000000000, -0.3202698538628350744 ) ) ;
#5783 = CIRCLE ( 'NONE', #14136, 125.0000000000000000 ) ;
#5784 = FACE_BOUND ( 'NONE', #7278, .T. ) ;
#5785 = DIRECTION ( 'NONE',  ( 0.000000000000000000, 0.000000000000000000, 1.000000000000000000 ) ) ;
#5786 = ORIENTED_EDGE ( 'NONE', *, *, #13438, .F. ) ;
#5787 = LINE ( 'NONE', #46237, #8629 ) ;
#5788 = ORIENTED_EDGE ( 'NONE', *, *, #37813, .T. ) ;
#5789 = EDGE_CURVE ( 'NONE', #7450, #24959, #1628, .T. ) ;
#5790 = VECTOR ( 'NONE', #20175, 1000.000000000000000 ) ;
#5791 = DIRECTION ( 'NONE',  ( 0.000000000000000000, -1.000000000000000000, 0.000000000000000000 ) ) ;
#5792 = DIRECTION ( 'NONE',  ( 0.000000000000000000, 0.000000000000000000, 1.000000000000000000 ) ) ;
#5793 = FACE_OUTER_BOUND ( 'NONE', #8511, .T. ) ;
#5794 = PLANE ( 'NONE',  #3993 ) ;
#5795 = CARTESIAN_POINT ( 'NONE',  ( -48.47912675150885065, -187.5000000000000284, 6.938893903907228378E-15 ) ) ;
#5796 = EDGE_LOOP ( 'NONE', ( #23948, #26673, #21207, #21353 ) ) ;
#5797 = AXIS2_PLACEMENT_3D ( 'NONE', #19622, #46715, #26731 ) ;
#5798 = DIRECTION ( 'NONE',  ( 0.000000000000000000, 0.6631226582407911962, -0.7485107481711046340 ) ) ;
#5799 = ORIENTED_EDGE ( 'NONE', *, *, #10845, .F. ) ;
#5800 = DIRECTION ( 'NONE',  ( 0.000000000000000000, 1.000000000000000000, -0.000000000000000000 ) ) ;
#5801 = ORIENTED_EDGE ( 'NONE', *, *, #9274, .T. ) ;
#5802 = LINE ( 'NONE', #21816, #49444 ) ;
#5803 = EDGE_CURVE ( 'NONE', #7481, #26682, #17665, .T. ) ;
#5804 = VERTEX_POINT ( 'NONE', #18170 ) ;
#5805 = EDGE_CURVE ( 'NONE', #12980, #23327, #50242, .T. ) ;
#5806 = EDGE_CURVE ( 'NONE', #29626, #21379, #30806, .T. ) ;
#5807 = EDGE_CURVE ( 'NONE', #29662, #1527, #41826, .T. ) ;
#5808 = CARTESIAN_POINT ( 'NONE',  ( 46.40005841627164074, -177.1207230881787780, 81.38144888055276738 ) ) ;
#5809 = CARTESIAN_POINT ( 'NONE',  ( 49.03269102277813829, 30.00000000000000355, -50.83217377521822300 ) ) ;
#5810 = ORIENTED_EDGE ( 'NONE', *, *, #23410, .F. ) ;
#5813 = ORIENTED_EDGE ( 'NONE', *, *, #18036, .F. ) ;
#5812 = LINE ( 'NONE', #29428, #24154 ) ;
#5811 = LINE ( 'NONE', #5280, #674 ) ;
#5814 = AXIS2_PLACEMENT_3D ( 'NONE', #48143, #24227, #40236 ) ;
#5815 = AXIS2_PLACEMENT_3D ( 'NONE', #33870, #5791, #29666 ) ;
#5816 = CARTESIAN_POINT ( 'NONE',  ( 57.61256176024323139, -183.6283474603465606, -64.19309449102733822 ) ) ;
#5817 = VERTEX_POINT ( 'NONE', #5845 ) ;
#5818 = CARTESIAN_POINT ( 'NONE',  ( 46.00000000000000000, 0.000000000000000000, 4.999999999999997335 ) ) ;
#5819 = VECTOR ( 'NONE', #27024, 1000.000000000000000 ) ;
#5820 = DIRECTION ( 'NONE',  ( 0.000000000000000000, -1.000000000000000000, 0.000000000000000000 ) ) ;
#5823 = VERTEX_POINT ( 'NONE', #33924 ) ;
#5822 = CYLINDRICAL_SURFACE ( 'NONE', #45160, 125.0000000000000000 ) ;
#5821 = CARTESIAN_POINT ( 'NONE',  ( -180.0000000000000568, -123.5000000000000284, 0.000000000000000000 ) ) ;
#5824 = VERTEX_POINT ( 'NONE', #21332 ) ;
#5825 = AXIS2_PLACEMENT_3D ( 'NONE', #35611, #26705, #11703 ) ;
#5826 = CARTESIAN_POINT ( 'NONE',  ( -44.48323084606168720, -177.1207230881787780, 123.9361149384469769 ) ) ;
#5827 = CARTESIAN_POINT ( 'NONE',  ( -60.00000000000000000, 20.00000000000000000, 60.00000000000000711 ) ) ;
#5828 = CARTESIAN_POINT ( 'NONE',  ( -33.64434644548590825, -189.7472609257535510, -123.1094209424468033 ) ) ;
#5829 = ADVANCED_FACE ( 'NONE', ( #25526 ), #49715, .T. ) ;
#5830 = VERTEX_POINT ( 'NONE', #10034 ) ;
#5831 = DIRECTION ( 'NONE',  ( 0.000000000000000000, 0.000000000000000000, 1.000000000000000000 ) ) ;
#5832 = DIRECTION ( 'NONE',  ( -1.000000000000000000, 0.000000000000000000, -0.000000000000000000 ) ) ;
#5833 = DIRECTION ( 'NONE',  ( 0.000000000000000000, -1.000000000000000000, 0.000000000000000000 ) ) ;
#5834 = CARTESIAN_POINT ( 'NONE',  ( -336.3521761649654422, -159.1821513111375452, -47.06073758877369073 ) ) ;
#5835 = ORIENTED_EDGE ( 'NONE', *, *, #14105, .F. ) ;
#5836 = DIRECTION ( 'NONE',  ( 0.9890401873221633666, 0.000000000000000000, 0.1476465640024850756 ) ) ;
#5837 = CARTESIAN_POINT ( 'NONE',  ( -48.47912675150885065, -189.7472609257535510, 6.938893903907228378E-15 ) ) ;
#5838 = EDGE_CURVE ( 'NONE', #23880, #49057, #26048, .T. ) ;
#5839 = VECTOR ( 'NONE', #30740, 1000.000000000000114 ) ;
#5840 = CARTESIAN_POINT ( 'NONE',  ( 0.7476021451244497795, -189.7472609257535510, -113.8100815915415609 ) ) ;
#5841 = ORIENTED_EDGE ( 'NONE', *, *, #43762, .T. ) ;
#5842 = CARTESIAN_POINT ( 'NONE',  ( -339.1964088526558498, -180.9052250602809977, -13.63415328425247885 ) ) ;
#5843 = CARTESIAN_POINT ( 'NONE',  ( 10.73478887071927623, -183.6283474603465606, -110.0850225811106924 ) ) ;
#5844 = CARTESIAN_POINT ( 'NONE',  ( -22.44626007086657182, -177.1207230881787780, 122.2591094863196730 ) ) ;
#5845 = CARTESIAN_POINT ( 'NONE',  ( -140.1460956102404509, -189.7472609257535510, 84.98333260264820410 ) ) ;
#5846 = PLANE ( 'NONE',  #32142 ) ;
#5847 = AXIS2_PLACEMENT_3D ( 'NONE', #28242, #44294, #36130 ) ;
#5848 = DIRECTION ( 'NONE',  ( -0.05924062789372142729, 0.000000000000000000, 0.9982437317643209074 ) ) ;
#5849 = LINE ( 'NONE', #28943, #30395 ) ;
#5851 = ORIENTED_EDGE ( 'NONE', *, *, #23597, .T. ) ;
#5850 = FACE_OUTER_BOUND ( 'NONE', #15935, .T. ) ;
#5852 = VECTOR ( 'NONE', #3571, 1000.000000000000227 ) ;
#5853 = ORIENTED_EDGE ( 'NONE', *, *, #46719, .T. ) ;
#5854 = CARTESIAN_POINT ( 'NONE',  ( -339.1964088526558498, -96.52406086224443982, -52.47426709956138069 ) ) ;
#5856 = VERTEX_POINT ( 'NONE', #49973 ) ;
#5855 = DIRECTION ( 'NONE',  ( 0.000000000000000000, -0.000000000000000000, -1.000000000000000000 ) ) ;
#5857 = ORIENTED_EDGE ( 'NONE', *, *, #49963, .T. ) ;
#5858 = ORIENTED_EDGE ( 'NONE', *, *, #25980, .F. ) ;
#5859 = DIRECTION ( 'NONE',  ( 0.000000000000000000, -1.000000000000000000, 0.000000000000000000 ) ) ;
#5860 = EDGE_CURVE ( 'NONE', #24862, #41328, #7332, .T. ) ;
#5861 = EDGE_CURVE ( 'NONE', #40560, #34017, #13967, .T. ) ;
#5862 = CARTESIAN_POINT ( 'NONE',  ( 67.29303306501925874, -189.7472609257535510, 47.13604789772128356 ) ) ;
#5863 = DIRECTION ( 'NONE',  ( 0.000000000000000000, 0.000000000000000000, -1.000000000000000000 ) ) ;
#5864 = EDGE_LOOP ( 'NONE', ( #40634, #40989, #4096, #31975 ) ) ;
#5865 = VECTOR ( 'NONE', #11967, 1000.000000000000000 ) ;
#5866 = DIRECTION ( 'NONE',  ( -0.000000000000000000, -1.000000000000000000, -0.000000000000000000 ) ) ;
#5868 = ORIENTED_EDGE ( 'NONE', *, *, #46874, .F. ) ;
#5867 = DIRECTION ( 'NONE',  ( -0.000000000000000000, -1.000000000000000000, 0.000000000000000000 ) ) ;
#5869 = CARTESIAN_POINT ( 'NONE',  ( -48.88225018079680950, -175.3837268820161057, -0.9151456172430169067 ) ) ;
#5870 = ORIENTED_EDGE ( 'NONE', *, *, #42970, .T. ) ;
#5871 = CARTESIAN_POINT ( 'NONE',  ( 73.62243227112294619, -183.6283474603465606, 21.61797988633237821 ) ) ;
#5872 = EDGE_LOOP ( 'NONE', ( #29122, #3420, #37191, #10143 ) ) ;
#5873 = PLANE ( 'NONE',  #25762 ) ;
#5874 = DIRECTION ( 'NONE',  ( -0.5586467658036594619, 0.000000000000000000, 0.8294056854501971054 ) ) ;
#5875 = CARTESIAN_POINT ( 'NONE',  ( 12.12533326292401803, -183.6283474603465606, 109.3256576763158989 ) ) ;
#5876 = ORIENTED_EDGE ( 'NONE', *, *, #25336, .F. ) ;
#5877 = VERTEX_POINT ( 'NONE', #6088 ) ;
#5878 = DIRECTION ( 'NONE',  ( -0.9646355819083614058, 0.000000000000000000, 0.2635871660690581320 ) ) ;
#5880 = AXIS2_PLACEMENT_3D ( 'NONE', #46493, #21550, #25743 ) ;
#5879 = DIRECTION ( 'NONE',  ( -0.000000000000000000, 1.000000000000000000, 0.000000000000000000 ) ) ;
#5881 = ORIENTED_EDGE ( 'NONE', *, *, #24044, .T. ) ;
#5882 = EDGE_CURVE ( 'NONE', #19062, #46515, #29722, .T. ) ;
#5883 = PLANE ( 'NONE',  #1370 ) ;
#5884 = ORIENTED_EDGE ( 'NONE', *, *, #20803, .T. ) ;
#5885 = FACE_OUTER_BOUND ( 'NONE', #25999, .T. ) ;
#5886 = DIRECTION ( 'NONE',  ( 0.000000000000000000, 1.000000000000000000, -0.000000000000000000 ) ) ;
#5887 = ADVANCED_FACE ( 'NONE', ( #38123 ), #17138, .T. ) ;
#5888 = PRODUCT ( 'Quick-Change Tool Holder Block', 'Quick-Change Tool Holder Block', '', ( #4984 ) ) ;
#5889 = VERTEX_POINT ( 'NONE', #13449 ) ;
#5890 = CARTESIAN_POINT ( 'NONE',  ( 60.00000000000001421, -93.50000000000002842, -4.038388177301730527E-15 ) ) ;
#5891 = ORIENTED_EDGE ( 'NONE', *, *, #6062, .T. ) ;
#5892 = DIRECTION ( 'NONE',  ( -0.000000000000000000, 1.000000000000000000, 0.000000000000000000 ) ) ;
#5893 = DIRECTION ( 'NONE',  ( -1.000000000000000000, -9.241633304753572918E-15, -4.850383327711924655E-15 ) ) ;
#5894 = DIRECTION ( 'NONE',  ( 0.000000000000000000, 0.000000000000000000, 1.000000000000000000 ) ) ;
#5895 = ORIENTED_EDGE ( 'NONE', *, *, #17945, .T. ) ;
#5896 = FACE_OUTER_BOUND ( 'NONE', #48791, .T. ) ;
#5897 = DIRECTION ( 'NONE',  ( 1.000000000000000000, -0.000000000000000000, -0.000000000000000000 ) ) ;
#5898 = CARTESIAN_POINT ( 'NONE',  ( -171.5708553757489767, -183.6283474603465606, 14.98512977653254019 ) ) ;
#5899 = ADVANCED_FACE ( 'NONE', ( #29464 ), #45514, .F. ) ;
#5900 = LINE ( 'NONE', #7110, #8981 ) ;
#5901 = AXIS2_PLACEMENT_3D ( 'NONE', #21940, #30584, #50842 ) ;
#5902 = EDGE_LOOP ( 'NONE', ( #16328, #46896, #49280, #41571 ) ) ;
#5903 = CIRCLE ( 'NONE', #37878, 125.0000000000000000 ) ;
#5904 = CARTESIAN_POINT ( 'NONE',  ( 38.46761263173351608, -193.5000000000000000, 89.80681772907068705 ) ) ;
#5905 = ORIENTED_EDGE ( 'NONE', *, *, #13377, .F. ) ;
#5906 = LINE ( 'NONE', #4868, #47117 ) ;
#5908 = ORIENTED_EDGE ( 'NONE', *, *, #30592, .F. ) ;
#5907 = LINE ( 'NONE', #45587, #44643 ) ;
#5909 = EDGE_LOOP ( 'NONE', ( #34115, #14262, #26160, #23981 ) ) ;
#5910 = EDGE_CURVE ( 'NONE', #512, #46176, #44239, .T. ) ;
#5911 = FACE_OUTER_BOUND ( 'NONE', #18914, .T. ) ;
#5912 = ORIENTED_EDGE ( 'NONE', *, *, #22122, .T. ) ;
#5913 = VECTOR ( 'NONE', #39102, 1000.000000000000000 ) ;
#5914 = LINE ( 'NONE', #21928, #31488 ) ;
#5915 = ORIENTED_EDGE ( 'NONE', *, *, #3695, .T. ) ;
#5916 = LINE ( 'NONE', #38476, #34236 ) ;
#5917 = DIRECTION ( 'NONE',  ( -0.000000000000000000, 0.000000000000000000, -1.000000000000000000 ) ) ;
#5918 = ADVANCED_FACE ( 'NONE', ( #25026 ), #37626, .F. ) ;
#5919 = EDGE_CURVE ( 'NONE', #15614, #10929, #20759, .T. ) ;
#5920 = CARTESIAN_POINT ( 'NONE',  ( -170.0000000000000284, -113.5000000000000000, 60.00000000000000711 ) ) ;
#5921 = CYLINDRICAL_SURFACE ( 'NONE', #41664, 125.0000000000000000 ) ;
#5922 = VERTEX_POINT ( 'NONE', #27329 ) ;
#5923 = ORIENTED_EDGE ( 'NONE', *, *, #44958, .F. ) ;
#5924 = ORIENTED_EDGE ( 'NONE', *, *, #41680, .T. ) ;
#5925 = CARTESIAN_POINT ( 'NONE',  ( -330.4913330509368166, -144.8891964568525452, -54.98865587491815177 ) ) ;
#5926 = CARTESIAN_POINT ( 'NONE',  ( -336.3521761649654422, -64.50000000000000000, -1.632288850093980725 ) ) ;
#5927 = EDGE_CURVE ( 'NONE', #25253, #13273, #47323, .T. ) ;
#5928 = DIRECTION ( 'NONE',  ( -0.1182731709213523247, 0.000000000000000000, -0.9929810960135185827 ) ) ;
#5929 = DIRECTION ( 'NONE',  ( -0.000000000000000000, 1.000000000000000000, -0.000000000000000000 ) ) ;
#5930 = ORIENTED_EDGE ( 'NONE', *, *, #5076, .T. ) ;
#5931 = AXIS2_PLACEMENT_3D ( 'NONE', #16061, #43404, #6877 ) ;
#5932 = AXIS2_PLACEMENT_3D ( 'NONE', #38122, #25793, #49972 ) ;
#5933 = ORIENTED_EDGE ( 'NONE', *, *, #41670, .F. ) ;
#5935 = VERTEX_POINT ( 'NONE', #38643 ) ;
#5934 = CARTESIAN_POINT ( 'NONE',  ( -170.6250538923603131, -189.7472609257535510, 26.55884942729648657 ) ) ;
#5936 = DIRECTION ( 'NONE',  ( 0.000000000000000000, 0.8660254037844354880, -0.5000000000000054401 ) ) ;
#5937 = EDGE_CURVE ( 'NONE', #39637, #27204, #22632, .T. ) ;
#5938 = CARTESIAN_POINT ( 'NONE',  ( -305.0000000000000568, -123.5000000000000142, 60.00000000000000000 ) ) ;
#5939 = CARTESIAN_POINT ( 'NONE',  ( -170.0000000000000284, -93.50000000000002842, 51.54700538379266561 ) ) ;
#5940 = DIRECTION ( 'NONE',  ( 0.000000000000000000, -1.000000000000000000, 0.000000000000000000 ) ) ;
#5941 = VERTEX_POINT ( 'NONE', #42846 ) ;
#5942 = CARTESIAN_POINT ( 'NONE',  ( -25.00456841203573077, 20.00000000000000355, 0.000000000000000000 ) ) ;
#5943 = VERTEX_POINT ( 'NONE', #42326 ) ;
#5944 = ORIENTED_EDGE ( 'NONE', *, *, #16377, .T. ) ;
#5945 = DIRECTION ( 'NONE',  ( 0.6068001458185890984, 0.000000000000000000, 0.7948544414133565938 ) ) ;
#5946 = CIRCLE ( 'NONE', #9278, 125.0000000000000000 ) ;
#5947 = CARTESIAN_POINT ( 'NONE',  ( -49.47868758801764955, -175.3837268820161057, -0.02963332782256313663 ) ) ;
#5948 = ORIENTED_EDGE ( 'NONE', *, *, #27503, .T. ) ;
#5949 = CARTESIAN_POINT ( 'NONE',  ( -165.7578939544008847, -193.5000000000000000, -43.25148278810626579 ) ) ;
#5950 = FACE_OUTER_BOUND ( 'NONE', #28430, .T. ) ;
#5951 = CARTESIAN_POINT ( 'NONE',  ( -130.2106798473772642, -193.5000000000000000, 94.57776286494217288 ) ) ;
#5952 = PLANE ( 'NONE',  #29069 ) ;
#5953 = DIRECTION ( 'NONE',  ( 0.4031234292879730674, 0.000000000000000000, -0.9151456172430181280 ) ) ;
#5954 = LINE ( 'NONE', #29851, #45062 ) ;
#5955 = ORIENTED_EDGE ( 'NONE', *, *, #23102, .T. ) ;
#5956 = DIRECTION ( 'NONE',  ( -0.000000000000000000, -0.9709418174260502354, 0.2393156642875652051 ) ) ;
#5957 = ORIENTED_EDGE ( 'NONE', *, *, #1216, .T. ) ;
#5958 = AXIS2_PLACEMENT_3D ( 'NONE', #22107, #37867, #42321 ) ;
#5959 = EDGE_CURVE ( 'NONE', #10174, #9490, #30762, .T. ) ;
#5960 = VERTEX_POINT ( 'NONE', #46813 ) ;
#5961 = LINE ( 'NONE', #1493, #31322 ) ;
#5962 = ORIENTED_EDGE ( 'NONE', *, *, #41022, .F. ) ;
#5963 = CARTESIAN_POINT ( 'NONE',  ( -48.02249751411513756, -193.5000000000000000, -0.8896570909947397743 ) ) ;
#5964 = CARTESIAN_POINT ( 'NONE',  ( -305.0000000000000568, -132.3499116637027271, -59.34373651485605450 ) ) ;
#5966 = ORIENTED_EDGE ( 'NONE', *, *, #24240, .F. ) ;
#5965 = DIRECTION ( 'NONE',  ( 0.000000000000000000, -1.000000000000000000, -0.000000000000000000 ) ) ;
#5967 = EDGE_CURVE ( 'NONE', #21665, #9485, #51517, .T. ) ;
#5968 = DIRECTION ( 'NONE',  ( -1.000000000000000000, 0.000000000000000000, 0.000000000000000000 ) ) ;
#5969 = CARTESIAN_POINT ( 'NONE',  ( 60.00000000000000000, -63.50000000000000000, 60.00000000000000711 ) ) ;
#5970 = VERTEX_POINT ( 'NONE', #7382 ) ;
#5971 = ORIENTED_EDGE ( 'NONE', *, *, #23297, .T. ) ;
#5972 = EDGE_CURVE ( 'NONE', #3044, #28776, #39209, .T. ) ;
#5973 = ORIENTED_EDGE ( 'NONE', *, *, #11033, .T. ) ;
#5974 = DIRECTION ( 'NONE',  ( 0.000000000000000000, 0.000000000000000000, -1.000000000000000000 ) ) ;
#5975 = CARTESIAN_POINT ( 'NONE',  ( -336.3521761649654422, -146.8829211657874794, -54.23253582808848705 ) ) ;
#5976 = ADVANCED_FACE ( 'NONE', ( #2905 ), #43376, .T. ) ;
#5977 = CIRCLE ( 'NONE', #45409, 125.0000000000000000 ) ;
#5978 = LINE ( 'NONE', #49864, #13374 ) ;
#5979 = CARTESIAN_POINT ( 'NONE',  ( -339.1964088526558498, -180.9052250602809977, -13.63415328425247885 ) ) ;
#5980 = CARTESIAN_POINT ( 'NONE',  ( 2.266533711611414148, -193.5000000000000000, 113.1409892739925596 ) ) ;
#5981 = ORIENTED_EDGE ( 'NONE', *, *, #1517, .T. ) ;
#5982 = DIRECTION ( 'NONE',  ( 0.000000000000000000, 0.000000000000000000, 1.000000000000000000 ) ) ;
#5983 = ORIENTED_EDGE ( 'NONE', *, *, #47689, .F. ) ;
#5985 = ORIENTED_EDGE ( 'NONE', *, *, #16336, .F. ) ;
#5984 = DIRECTION ( 'NONE',  ( -0.000000000000000000, 1.000000000000000000, 0.000000000000000000 ) ) ;
#5986 = ORIENTED_EDGE ( 'NONE', *, *, #22939, .F. ) ;
#5987 = ORIENTED_EDGE ( 'NONE', *, *, #34275, .T. ) ;
#5988 = DIRECTION ( 'NONE',  ( 0.000000000000000000, -7.285838599102589797E-14, 1.000000000000000000 ) ) ;
#5989 = VECTOR ( 'NONE', #6211, 1000.000000000000227 ) ;
#5990 = VERTEX_POINT ( 'NONE', #51270 ) ;
#5991 = LINE ( 'NONE', #38563, #1987 ) ;
#5992 = CARTESIAN_POINT ( 'NONE',  ( 75.78974234412359579, -183.6283474603465606, 13.49993235881448861 ) ) ;
#5993 = ORIENTED_EDGE ( 'NONE', *, *, #51545, .T. ) ;
#5994 = FACE_BOUND ( 'NONE', #27705, .T. ) ;
#5995 = ORIENTED_EDGE ( 'NONE', *, *, #13016, .T. ) ;
#5996 = VECTOR ( 'NONE', #11750, 999.9999999999998863 ) ;
#5997 = VERTEX_POINT ( 'NONE', #23404 ) ;
#5998 = LINE ( 'NONE', #14405, #51429 ) ;
#5999 = CARTESIAN_POINT ( 'NONE',  ( 0.000000000000000000, -123.4999999999994174, 59.00000000000002132 ) ) ;
#6000 = CARTESIAN_POINT ( 'NONE',  ( 116.9235303384055840, -213.5000000000000000, -9.999999999999971578 ) ) ;
#6001 = CARTESIAN_POINT ( 'NONE',  ( -339.1964088526558498, -171.7720157143598669, 33.92731199008546383 ) ) ;
#6002 = ORIENTED_EDGE ( 'NONE', *, *, #38659, .T. ) ;
#6003 = CARTESIAN_POINT ( 'NONE',  ( -332.3517673607765914, -182.1255794688777314, -12.76876783163923967 ) ) ;
#6004 = CARTESIAN_POINT ( 'NONE',  ( -48.47912675150885065, -189.7472609257535510, 6.938893903907228378E-15 ) ) ;
#6005 = CARTESIAN_POINT ( 'NONE',  ( -150.5816505765687907, -177.1207230881787780, 70.36529243996407956 ) ) ;
#6006 = FACE_OUTER_BOUND ( 'NONE', #41996, .T. ) ;
#6007 = ORIENTED_EDGE ( 'NONE', *, *, #34256, .T. ) ;
#6008 = DIRECTION ( 'NONE',  ( -0.000000000000000000, -0.8854560256532079121, 0.4647231720437724478 ) ) ;
#6009 = CARTESIAN_POINT ( 'NONE',  ( -339.1964088526558498, -180.6659093959932250, 14.60509510167942437 ) ) ;
#6010 = VECTOR ( 'NONE', #45986, 1000.000000000000000 ) ;
#6011 = DIRECTION ( 'NONE',  ( 0.2348860457809707758, 0.000000000000000000, 0.9720229140804138579 ) ) ;
#6012 = ORIENTED_EDGE ( 'NONE', *, *, #49755, .F. ) ;
#6013 = ORIENTED_EDGE ( 'NONE', *, *, #28931, .F. ) ;
#6014 = VECTOR ( 'NONE', #48439, 1000.000000000000114 ) ;
#6015 = DIRECTION ( 'NONE',  ( 0.000000000000000000, -1.000000000000000000, 0.000000000000000000 ) ) ;
#6016 = EDGE_CURVE ( 'NONE', #33758, #2870, #23148, .T. ) ;
#6017 = DIRECTION ( 'NONE',  ( -0.000000000000000000, 1.000000000000000000, 0.000000000000000000 ) ) ;
#6018 = LINE ( 'NONE', #41765, #46306 ) ;
#6019 = EDGE_CURVE ( 'NONE', #44261, #1781, #31270, .T. ) ;
#6020 = ORIENTED_EDGE ( 'NONE', *, *, #8147, .F. ) ;
#6021 = ADVANCED_FACE ( 'NONE', ( #3418 ), #10278, .F. ) ;
#6022 = LINE ( 'NONE', #22042, #48060 ) ;
#6023 = VERTEX_POINT ( 'NONE', #47064 ) ;
#6024 = EDGE_CURVE ( 'NONE', #50020, #4319, #38900, .T. ) ;
#6025 = DIRECTION ( 'NONE',  ( -0.000000000000000000, 1.000000000000000000, -0.000000000000000000 ) ) ;
#6026 = EDGE_CURVE ( 'NONE', #4313, #48860, #7113, .T. ) ;
#6027 = CARTESIAN_POINT ( 'NONE',  ( -305.0000000000000568, -93.31268025388605736, 51.85292399224828586 ) ) ;
#6028 = CARTESIAN_POINT ( 'NONE',  ( -160.9694636715425702, -189.7472609257535510, 54.50618404931040573 ) ) ;
#6029 = EDGE_CURVE ( 'NONE', #33953, #21286, #11039, .T. ) ;
#6030 = AXIS2_PLACEMENT_3D ( 'NONE', #9566, #25584, #37416 ) ;
#6031 = CARTESIAN_POINT ( 'NONE',  ( -336.3521761649654422, -105.0395444947681369, -56.09938080879045685 ) ) ;
#6032 = EDGE_CURVE ( 'NONE', #25657, #19312, #15517, .T. ) ;
#6033 = VECTOR ( 'NONE', #41412, 1000.000000000000000 ) ;
#6034 = LINE ( 'NONE', #17615, #16793 ) ;
#6035 = ORIENTED_EDGE ( 'NONE', *, *, #2411, .T. ) ;
#6036 = ADVANCED_FACE ( 'NONE', ( #26297 ), #6344, .T. ) ;
#6037 = AXIS2_PLACEMENT_3D ( 'NONE', #46301, #50753, #10800 ) ;
#6038 = DIRECTION ( 'NONE',  ( 0.8124868780056863082, 0.000000000000000000, -0.5829794791144649047 ) ) ;
#6039 = ORIENTED_EDGE ( 'NONE', *, *, #50259, .T. ) ;
#6040 = DIRECTION ( 'NONE',  ( -1.000000000000000000, 0.000000000000000000, 0.000000000000000000 ) ) ;
#6041 = EDGE_CURVE ( 'NONE', #17251, #51869, #34448, .T. ) ;
#6042 = ORIENTED_EDGE ( 'NONE', *, *, #35216, .F. ) ;
#6043 = FACE_OUTER_BOUND ( 'NONE', #37908, .T. ) ;
#6044 = EDGE_CURVE ( 'NONE', #44797, #31178, #6609, .T. ) ;
#6045 = VECTOR ( 'NONE', #17985, 1000.000000000000114 ) ;
#6046 = CARTESIAN_POINT ( 'NONE',  ( -98.10897907742933910, -175.3837268820161057, 114.7252272087849434 ) ) ;
#6047 = CARTESIAN_POINT ( 'NONE',  ( -172.2289551866394106, -189.7472609257535510, -17.63462396184710101 ) ) ;
#6048 = ORIENTED_EDGE ( 'NONE', *, *, #17002, .F. ) ;
#6051 = VERTEX_POINT ( 'NONE', #47839 ) ;
#6050 = LINE ( 'NONE', #25495, #17454 ) ;
#6049 = CARTESIAN_POINT ( 'NONE',  ( -1.985599386381375009, 50.94104332004447144, -21.04987985461054834 ) ) ;
#6052 = AXIS2_PLACEMENT_3D ( 'NONE', #45526, #50253, #26315 ) ;
#6053 = AXIS2_PLACEMENT_3D ( 'NONE', #10948, #19608, #2795 ) ;
#6054 = FACE_OUTER_BOUND ( 'NONE', #49791, .T. ) ;
#6055 = VERTEX_POINT ( 'NONE', #16286 ) ;
#6056 = DIRECTION ( 'NONE',  ( -1.000000000000000000, 0.000000000000000000, 0.000000000000000000 ) ) ;
#6057 = ORIENTED_EDGE ( 'NONE', *, *, #38339, .F. ) ;
#6058 = CARTESIAN_POINT ( 'NONE',  ( 0.000000000000000000, -43.50000000000000000, 60.00000000000000711 ) ) ;
#6061 = VERTEX_POINT ( 'NONE', #11809 ) ;
#6060 = DIRECTION ( 'NONE',  ( 0.000000000000000000, 0.000000000000000000, -1.000000000000000000 ) ) ;
#6059 = DIRECTION ( 'NONE',  ( 0.000000000000000000, 0.000000000000000000, 1.000000000000000000 ) ) ;
#6062 = EDGE_CURVE ( 'NONE', #15284, #8221, #3947, .T. ) ;
#6063 = ORIENTED_EDGE ( 'NONE', *, *, #27934, .F. ) ;
#6064 = CARTESIAN_POINT ( 'NONE',  ( -155.4465502054561057, -193.5000000000000000, 64.67588669375881238 ) ) ;
#6065 = ORIENTED_EDGE ( 'NONE', *, *, #21870, .T. ) ;
#6066 = CARTESIAN_POINT ( 'NONE',  ( -46.00000000000000711, 20.00000000000000000, 51.00000000000000000 ) ) ;
#6067 = LINE ( 'NONE', #42828, #45827 ) ;
#6068 = ORIENTED_EDGE ( 'NONE', *, *, #245, .T. ) ;
#6069 = FACE_OUTER_BOUND ( 'NONE', #5335, .T. ) ;
#6070 = CARTESIAN_POINT ( 'NONE',  ( 53.77560546639968919, 28.00000000000000355, -28.45764841024206504 ) ) ;
#6071 = DIRECTION ( 'NONE',  ( -0.000000000000000000, -1.000000000000000000, 0.000000000000000000 ) ) ;
#6072 = DIRECTION ( 'NONE',  ( -0.000000000000000000, -0.9927088740980530845, 0.1205366802553303057 ) ) ;
#6073 = VECTOR ( 'NONE', #13512, 1000.000000000000227 ) ;
#6074 = DIRECTION ( 'NONE',  ( 0.000000000000000000, 1.000000000000000000, -6.938893903907222461E-16 ) ) ;
#6075 = ORIENTED_EDGE ( 'NONE', *, *, #49419, .F. ) ;
#6076 =( LENGTH_UNIT ( ) NAMED_UNIT ( * ) SI_UNIT ( .MILLI., .METRE. ) );
#6077 = DIRECTION ( 'NONE',  ( 0.000000000000000000, -1.000000000000000000, 0.000000000000000000 ) ) ;
#6078 = CARTESIAN_POINT ( 'NONE',  ( -124.1938582159088327, -175.3837268820161057, -99.45993886622791536 ) ) ;
#6079 = AXIS2_PLACEMENT_3D ( 'NONE', #11818, #39421, #3423 ) ;
#6080 = EDGE_CURVE ( 'NONE', #37774, #49603, #11570, .T. ) ;
#6081 = DIRECTION ( 'NONE',  ( 0.000000000000000000, 1.000000000000000000, -0.000000000000000000 ) ) ;
#6082 = ORIENTED_EDGE ( 'NONE', *, *, #896, .T. ) ;
#6083 = LINE ( 'NONE', #21857, #3847 ) ;
#6084 = FACE_OUTER_BOUND ( 'NONE', #32766, .T. ) ;
#6085 = EDGE_CURVE ( 'NONE', #15537, #14073, #48087, .T. ) ;
#6086 = CYLINDRICAL_SURFACE ( 'NONE', #15979, 125.0000000000000000 ) ;
#6087 = EDGE_CURVE ( 'NONE', #21890, #36336, #36785, .T. ) ;
#6088 = CARTESIAN_POINT ( 'NONE',  ( -23.25236516653335528, -177.1207230881787780, -121.4073237908566654 ) ) ;
#6089 = ADVANCED_FACE ( 'NONE', ( #44139 ), #24182, .T. ) ;
#6090 = EDGE_CURVE ( 'NONE', #4175, #26454, #24966, .T. ) ;
#6091 = CIRCLE ( 'NONE', #48893, 60.00000000000000000 ) ;
#6092 = EDGE_CURVE ( 'NONE', #6218, #41928, #4207, .T. ) ;
#6093 = PLANE ( 'NONE',  #1954 ) ;
#6094 = CIRCLE ( 'NONE', #32065, 125.0000000000000000 ) ;
#6095 = ADVANCED_FACE ( 'NONE', ( #12596 ), #242, .T. ) ;
#6096 = CARTESIAN_POINT ( 'NONE',  ( -149.3265790242249125, -189.7472609257535510, 72.15117186584561182 ) ) ;
#6097 = ADVANCED_FACE ( 'NONE', ( #778 ), #7623, .F. ) ;
#6098 = PLANE ( 'NONE',  #3579 ) ;
#6099 = FACE_OUTER_BOUND ( 'NONE', #5207, .T. ) ;
#6100 = VERTEX_POINT ( 'NONE', #502 ) ;
#6101 = EDGE_CURVE ( 'NONE', #39324, #2101, #27838, .T. ) ;
#6102 = DIRECTION ( 'NONE',  ( 1.000000000000000000, -0.000000000000000000, -0.000000000000000000 ) ) ;
#6103 = ADVANCED_FACE ( 'NONE', ( #8657 ), #36004, .T. ) ;
#6104 = CARTESIAN_POINT ( 'NONE',  ( -165.7578939544008847, -183.6283474603465606, -43.25148278810625868 ) ) ;
#6106 = ORIENTED_EDGE ( 'NONE', *, *, #14754, .T. ) ;
#6105 = CARTESIAN_POINT ( 'NONE',  ( -365.0000000000001137, -78.50000000000002842, 0.000000000000000000 ) ) ;
#6107 = ORIENTED_EDGE ( 'NONE', *, *, #32288, .T. ) ;
#6108 = EDGE_CURVE ( 'NONE', #16449, #2507, #16099, .T. ) ;
#6109 = ORIENTED_EDGE ( 'NONE', *, *, #19130, .T. ) ;
#6110 = CARTESIAN_POINT ( 'NONE',  ( -170.0000000000000284, -123.5000000000000284, 15.24495751795539711 ) ) ;
#6111 = VECTOR ( 'NONE', #9424, 1000.000000000000000 ) ;
#6112 = EDGE_CURVE ( 'NONE', #19096, #37383, #28094, .T. ) ;
#6113 = CARTESIAN_POINT ( 'NONE',  ( 64.46023522152407281, -183.6283474603465606, -51.19472891551279758 ) ) ;
#6114 = CARTESIAN_POINT ( 'NONE',  ( -55.71438232577004612, -189.7472609257535510, -124.7904286264580662 ) ) ;
#6115 = EDGE_LOOP ( 'NONE', ( #44521, #33852, #47178, #1692 ) ) ;
#6116 = ADVANCED_FACE ( 'NONE', ( #32575 ), #44667, .T. ) ;
#6117 = VECTOR ( 'NONE', #4215, 1000.000000000000000 ) ;
#6118 = CARTESIAN_POINT ( 'NONE',  ( -336.3521761649654422, -179.2447759217480154, -19.39547174791710660 ) ) ;
#6119 = CARTESIAN_POINT ( 'NONE',  ( -330.4913330509368166, -68.15673923803900891, 20.45418021416622878 ) ) ;
#6122 = ORIENTED_EDGE ( 'NONE', *, *, #13376, .T. ) ;
#6121 = FACE_OUTER_BOUND ( 'NONE', #45040, .T. ) ;
#6120 = CARTESIAN_POINT ( 'NONE',  ( -260.0000000000000000, -63.50000000000000000, 60.00000000000000711 ) ) ;
#6123 = CARTESIAN_POINT ( 'NONE',  ( -305.0000000000000568, -149.9277501395804677, 53.86626052140529453 ) ) ;
#6124 = EDGE_LOOP ( 'NONE', ( #18334, #13747, #35732, #49886 ) ) ;
#6125 = DIRECTION ( 'NONE',  ( 0.000000000000000000, 0.000000000000000000, -1.000000000000000000 ) ) ;
#6126 = VERTEX_POINT ( 'NONE', #40698 ) ;
#6127 = DIRECTION ( 'NONE',  ( 0.000000000000000000, -0.8854560256532043594, 0.4647231720437789981 ) ) ;
#6128 = LINE ( 'NONE', #34234, #20429 ) ;
#6129 = DIRECTION ( 'NONE',  ( 0.000000000000000000, -0.000000000000000000, 1.000000000000000000 ) ) ;
#6130 = AXIS2_PLACEMENT_3D ( 'NONE', #21216, #5196, #21735 ) ;
#6131 = ADVANCED_FACE ( 'NONE', ( #2 ), #4722, .T. ) ;
#6132 = AXIS2_PLACEMENT_3D ( 'NONE', #15393, #35873, #47718 ) ;
#6133 = CARTESIAN_POINT ( 'NONE',  ( 0.000000000000000000, -63.50000000000000000, 60.00000000000000711 ) ) ;
#6134 = VERTEX_POINT ( 'NONE', #23900 ) ;
#6135 = CIRCLE ( 'NONE', #42192, 125.0000000000000000 ) ;
#6136 = CARTESIAN_POINT ( 'NONE',  ( -48.47912675150885065, -177.1207230881787780, 6.938893903907228378E-15 ) ) ;
#6137 = CARTESIAN_POINT ( 'NONE',  ( 76.28370911321320591, -183.6283474603465606, -7.696413904697499753 ) ) ;
#6138 = ORIENTED_EDGE ( 'NONE', *, *, #26102, .T. ) ;
#6139 = CARTESIAN_POINT ( 'NONE',  ( -332.3517673607765914, -64.61288906875131488, 4.498567634385603142 ) ) ;
#6140 = ORIENTED_EDGE ( 'NONE', *, *, #5434, .T. ) ;
#6141 = FACE_BOUND ( 'NONE', #47443, .T. ) ;
#6142 = LINE ( 'NONE', #41089, #36495 ) ;
#6143 = ORIENTED_EDGE ( 'NONE', *, *, #45690, .F. ) ;
#6144 = LINE ( 'NONE', #5890, #42526 ) ;
#6145 = VERTEX_POINT ( 'NONE', #39918 ) ;
#6146 = PLANE ( 'NONE',  #4626 ) ;
#6147 = CARTESIAN_POINT ( 'NONE',  ( -48.47912675150885065, -183.6283474603465606, 6.938893903907228378E-15 ) ) ;
#6148 = VERTEX_POINT ( 'NONE', #13641 ) ;
#6149 = AXIS2_PLACEMENT_3D ( 'NONE', #11681, #15378, #27181 ) ;
#6150 = ADVANCED_FACE ( 'NONE', ( #45453 ), #33089, .F. ) ;
#6151 = DIRECTION ( 'NONE',  ( -0.000000000000000000, 1.000000000000000000, -0.000000000000000000 ) ) ;
#6152 = CARTESIAN_POINT ( 'NONE',  ( -48.47912675150885065, -177.1207230881787780, 6.938893903907228378E-15 ) ) ;
#6153 = DIRECTION ( 'NONE',  ( 0.000000000000000000, 1.000000000000000000, 0.000000000000000000 ) ) ;
#6154 = EDGE_CURVE ( 'NONE', #2312, #16397, #49653, .T. ) ;
#6155 = ORIENTED_EDGE ( 'NONE', *, *, #7411, .T. ) ;
#6156 = CARTESIAN_POINT ( 'NONE',  ( -336.3521761649654422, -72.48138011061176655, -29.74944317415788930 ) ) ;
#6157 = ORIENTED_EDGE ( 'NONE', *, *, #8623, .F. ) ;
#6158 = CARTESIAN_POINT ( 'NONE',  ( 26.52087324849106054, -198.5000000000000000, -80.00000000000002842 ) ) ;
#6159 = LINE ( 'NONE', #18242, #23048 ) ;
#6161 = ORIENTED_EDGE ( 'NONE', *, *, #27908, .F. ) ;
#6160 = CARTESIAN_POINT ( 'NONE',  ( -169.1033029113419559, -175.3837268820161057, 32.78426643622745473 ) ) ;
#6162 = VERTEX_POINT ( 'NONE', #33611 ) ;
#6163 = DIRECTION ( 'NONE',  ( -0.1768902751225666370, 0.000000000000000000, -0.9842305779475979399 ) ) ;
#6164 = VECTOR ( 'NONE', #12329, 1000.000000000000000 ) ;
#6165 = AXIS2_PLACEMENT_3D ( 'NONE', #39032, #38263, #14117 ) ;
#6166 = DIRECTION ( 'NONE',  ( 0.000000000000000000, 0.1205366802553233113, 0.9927088740980538617 ) ) ;
#6167 = AXIS2_PLACEMENT_3D ( 'NONE', #25445, #5227, #17575 ) ;
#6168 = ORIENTED_EDGE ( 'NONE', *, *, #51976, .T. ) ;
#6169 = DIRECTION ( 'NONE',  ( 0.000000000000000000, -0.7485107481710954191, 0.6631226582408017434 ) ) ;
#6170 = EDGE_CURVE ( 'NONE', #40642, #29348, #24958, .T. ) ;
#6171 = ORIENTED_EDGE ( 'NONE', *, *, #26989, .F. ) ;
#6172 = DIRECTION ( 'NONE',  ( 0.9995608365087944591, 0.000000000000000000, -0.02963332782255633305 ) ) ;
#6173 = FACE_OUTER_BOUND ( 'NONE', #35747, .T. ) ;
#6174 = AXIS2_PLACEMENT_3D ( 'NONE', #19339, #42979, #6989 ) ;
#6175 = DIRECTION ( 'NONE',  ( -1.000000000000000000, 0.000000000000000000, 0.000000000000000000 ) ) ;
#6176 = CARTESIAN_POINT ( 'NONE',  ( -48.18706998087187543, -193.5000000000000000, -0.9564009842765152092 ) ) ;
#6177 = VERTEX_POINT ( 'NONE', #5252 ) ;
#6178 = EDGE_LOOP ( 'NONE', ( #43143, #331, #21252, #28782 ) ) ;
#6179 = EDGE_CURVE ( 'NONE', #19768, #24889, #32828, .T. ) ;
#6180 = ORIENTED_EDGE ( 'NONE', *, *, #18626, .F. ) ;
#6181 = LINE ( 'NONE', #30332, #46771 ) ;
#6182 = DIRECTION ( 'NONE',  ( 0.5586467658036535777, 0.000000000000000000, -0.8294056854502011022 ) ) ;
#6183 = FACE_OUTER_BOUND ( 'NONE', #14576, .T. ) ;
#6184 = DIRECTION ( 'NONE',  ( 0.9027978299657416494, 0.000000000000000000, 0.4300652022765245608 ) ) ;
#6185 = VECTOR ( 'NONE', #31798, 999.9999999999998863 ) ;
#6186 = ORIENTED_EDGE ( 'NONE', *, *, #15462, .F. ) ;
#6187 = CARTESIAN_POINT ( 'NONE',  ( -48.47912675150885065, -177.1207230881787780, 6.938893903907228378E-15 ) ) ;
#6188 = AXIS2_PLACEMENT_3D ( 'NONE', #13207, #29225, #45283 ) ;
#6189 = ORIENTED_EDGE ( 'NONE', *, *, #13664, .T. ) ;
#6191 = EDGE_LOOP ( 'NONE', ( #2211, #45285, #45421, #12883 ) ) ;
#6190 = CARTESIAN_POINT ( 'NONE',  ( -339.1964088526558498, -71.02573290043838483, 26.97593913775504504 ) ) ;
#6192 = CARTESIAN_POINT ( 'NONE',  ( -170.0000000000000284, -115.7896721143442278, -18.45401972188387418 ) ) ;
#6193 = FACE_OUTER_BOUND ( 'NONE', #42111, .T. ) ;
#6194 = DIRECTION ( 'NONE',  ( 0.000000000000000000, 0.000000000000000000, 1.000000000000000000 ) ) ;
#6195 = DIRECTION ( 'NONE',  ( -1.000000000000000000, 0.000000000000000000, -0.000000000000000000 ) ) ;
#6196 = ORIENTED_EDGE ( 'NONE', *, *, #47444, .T. ) ;
#6197 = DIRECTION ( 'NONE',  ( -0.000000000000000000, 1.000000000000000000, -0.000000000000000000 ) ) ;
#6198 = AXIS2_PLACEMENT_3D ( 'NONE', #27633, #15825, #24216 ) ;
#6199 = VERTEX_POINT ( 'NONE', #42006 ) ;
#6200 = APPLICATION_CONTEXT ( 'automotive_design' ) ;
#6201 = ORIENTED_EDGE ( 'NONE', *, *, #27233, .T. ) ;
#6202 = DIRECTION ( 'NONE',  ( -8.718379230999705894E-17, 0.9709418174260527890, 0.2393156642875547968 ) ) ;
#6203 = CIRCLE ( 'NONE', #28826, 125.0000000000000000 ) ;
#6204 = DIRECTION ( 'NONE',  ( -0.3482016354344059095, 0.000000000000000000, 0.9374196611341183427 ) ) ;
#6205 = ORIENTED_EDGE ( 'NONE', *, *, #19554, .T. ) ;
#6206 = LINE ( 'NONE', #30112, #38244 ) ;
#6207 = DIRECTION ( 'NONE',  ( -0.000000000000000000, 1.000000000000000000, -0.000000000000000000 ) ) ;
#6208 = CARTESIAN_POINT ( 'NONE',  ( -47.47956591500005885, -177.1207230881787780, -0.02963332782254939762 ) ) ;
#6209 = EDGE_CURVE ( 'NONE', #28959, #36297, #22754, .T. ) ;
#6210 = CARTESIAN_POINT ( 'NONE',  ( -305.0000000000000568, -128.1121410293017391, 59.82247199109905011 ) ) ;
#6211 = DIRECTION ( 'NONE',  ( -0.9473263538541876194, 0.000000000000000000, -0.3202698538628486746 ) ) ;
#6212 = ORIENTED_EDGE ( 'NONE', *, *, #21604, .T. ) ;
#6213 = LINE ( 'NONE', #33287, #17249 ) ;
#6214 = EDGE_LOOP ( 'NONE', ( #26053, #2053, #15278, #27777 ) ) ;
#6215 = VECTOR ( 'NONE', #14669, 1000.000000000000000 ) ;
#6216 = EDGE_LOOP ( 'NONE', ( #25405, #31444, #45804, #28110 ) ) ;
#6217 = CARTESIAN_POINT ( 'NONE',  ( 60.00000000000001421, 20.00000000000000000, 60.00000000000000711 ) ) ;
#6218 = VERTEX_POINT ( 'NONE', #29402 ) ;
#6219 = AXIS2_PLACEMENT_3D ( 'NONE', #7555, #29061, #5703 ) ;
#6220 = DIRECTION ( 'NONE',  ( 1.000000000000000000, -0.000000000000000000, 0.000000000000000000 ) ) ;
#6221 = DIRECTION ( 'NONE',  ( 1.000000000000000000, -0.000000000000000000, -0.000000000000000000 ) ) ;
#6222 = CARTESIAN_POINT ( 'NONE',  ( -330.4913330509368166, -123.5000000000000284, 0.000000000000000000 ) ) ;
#6223 = EDGE_CURVE ( 'NONE', #16369, #38638, #25731, .T. ) ;
#6224 = ORIENTED_EDGE ( 'NONE', *, *, #73, .T. ) ;
#6225 = CARTESIAN_POINT ( 'NONE',  ( -330.4913330509368166, -64.50000000000000000, -0.4999999999999549249 ) ) ;
#6227 = VECTOR ( 'NONE', #50769, 1000.000000000000000 ) ;
#6226 = DIRECTION ( 'NONE',  ( 1.000000000000000000, -0.000000000000000000, -0.000000000000000000 ) ) ;
#6228 = CYLINDRICAL_SURFACE ( 'NONE', #16505, 15.24495751795539000 ) ;
#6229 = VERTEX_POINT ( 'NONE', #49906 ) ;
#6230 = ORIENTED_EDGE ( 'NONE', *, *, #43566, .F. ) ;
#6231 = VERTEX_POINT ( 'NONE', #12855 ) ;
#6232 = DIRECTION ( 'NONE',  ( -0.4031234292879600778, 0.000000000000000000, -0.9151456172430237901 ) ) ;
#6233 = LINE ( 'NONE', #18327, #817 ) ;
#6234 = FILL_AREA_STYLE_COLOUR ( '', #20076 ) ;
#6235 = CYLINDRICAL_SURFACE ( 'NONE', #27005, 125.0000000000000000 ) ;
#6236 = DIRECTION ( 'NONE',  ( 0.000000000000000000, 1.000000000000000000, 0.000000000000000000 ) ) ;
#6237 = ORIENTED_EDGE ( 'NONE', *, *, #7064, .F. ) ;
#6238 = CARTESIAN_POINT ( 'NONE',  ( 32.49319223169170101, -175.3837268820161057, -95.22858582633061530 ) ) ;
#6239 = ORIENTED_EDGE ( 'NONE', *, *, #28044, .T. ) ;
#6241 = ORIENTED_EDGE ( 'NONE', *, *, #14748, .F. ) ;
#6240 = LINE ( 'NONE', #33578, #49143 ) ;
#6242 = VERTEX_POINT ( 'NONE', #9194 ) ;
#6243 = DIRECTION ( 'NONE',  ( -0.000000000000000000, 1.000000000000000000, -0.000000000000000000 ) ) ;
#6244 = EDGE_LOOP ( 'NONE', ( #2808, #40411, #9999, #22379 ) ) ;
#6245 = LINE ( 'NONE', #6771, #25803 ) ;
#6246 = CIRCLE ( 'NONE', #26383, 60.00000000000000000 ) ;
#6247 = ORIENTED_EDGE ( 'NONE', *, *, #1637, .T. ) ;
#6248 = CIRCLE ( 'NONE', #8747, 125.0000000000000000 ) ;
#6249 = ADVANCED_FACE ( 'NONE', ( #21011 ), #4995, .T. ) ;
#6250 = CARTESIAN_POINT ( 'NONE',  ( -48.47912675150885065, -132.5479369270331915, 15.00000000000000711 ) ) ;
#6251 = DIRECTION ( 'NONE',  ( -0.000000000000000000, -0.2393156642875582940, -0.9709418174260519008 ) ) ;
#6252 = VERTEX_POINT ( 'NONE', #13122 ) ;
#6253 = PLANE ( 'NONE',  #12378 ) ;
#6254 = ORIENTED_EDGE ( 'NONE', *, *, #12762, .F. ) ;
#6255 = VECTOR ( 'NONE', #8772, 1000.000000000000000 ) ;
#6256 = EDGE_CURVE ( 'NONE', #9002, #26704, #6018, .T. ) ;
#6257 = ORIENTED_EDGE ( 'NONE', *, *, #50887, .F. ) ;
#6258 = LINE ( 'NONE', #2321, #27052 ) ;
#6259 = DIRECTION ( 'NONE',  ( -0.000000000000000000, 1.000000000000000000, -0.000000000000000000 ) ) ;
#6260 = CARTESIAN_POINT ( 'NONE',  ( -48.18706998087188254, -175.3837268820161057, 0.9564009842765313074 ) ) ;
#6261 = ORIENTED_EDGE ( 'NONE', *, *, #33950, .F. ) ;
#6262 = CARTESIAN_POINT ( 'NONE',  ( -339.1964088526558498, -175.9742670995610752, 26.97593913775620678 ) ) ;
#6263 = DIRECTION ( 'NONE',  ( 0.000000000000000000, 0.000000000000000000, -1.000000000000000000 ) ) ;
#6264 = CONTEXT_DEPENDENT_SHAPE_REPRESENTATION ( #50186, #32687 ) ;
#6265 = CARTESIAN_POINT ( 'NONE',  ( 63.54086012517504400, -193.5000000000000000, -53.17445600718543375 ) ) ;
#6266 = LINE ( 'NONE', #29651, #12782 ) ;
#6267 = ADVANCED_FACE ( 'NONE', ( #28877 ), #1559, .T. ) ;
#6268 = EDGE_LOOP ( 'NONE', ( #46821, #26961, #16458, #9514 ) ) ;
#6269 = VECTOR ( 'NONE', #34786, 1000.000000000000000 ) ;
#6270 = DIRECTION ( 'NONE',  ( -0.000000000000000000, 1.000000000000000000, -0.000000000000000000 ) ) ;
#6271 = LINE ( 'NONE', #34879, #19847 ) ;
#6272 = EDGE_CURVE ( 'NONE', #49461, #3029, #33865, .T. ) ;
#6273 = DIRECTION ( 'NONE',  ( 0.000000000000000000, -1.000000000000000000, -0.000000000000000000 ) ) ;
#6274 = EDGE_LOOP ( 'NONE', ( #37030, #18109, #31849, #45930 ) ) ;
#6275 = EDGE_CURVE ( 'NONE', #29000, #44562, #1025, .T. ) ;
#6276 = CARTESIAN_POINT ( 'NONE',  ( -172.4295958414655274, -175.3837268820161057, 3.504489105735777432 ) ) ;
#6277 = SHAPE_REPRESENTATION ( 'Sliding track', ( #31742 ), #2380 ) ;
#6278 = DIRECTION ( 'NONE',  ( 0.9995608365087940150, 0.000000000000000000, 0.02963332782257007206 ) ) ;
#6279 = ORIENTED_EDGE ( 'NONE', *, *, #45493, .T. ) ;
#6280 = DIRECTION ( 'NONE',  ( 0.000000000000000000, 0.000000000000000000, 1.000000000000000000 ) ) ;
#6281 = ORIENTED_EDGE ( 'NONE', *, *, #13746, .T. ) ;
#6282 = PLANE ( 'NONE',  #47774 ) ;
#6283 = DIRECTION ( 'NONE',  ( 0.000000000000000000, 0.000000000000000000, -1.000000000000000000 ) ) ;
#6284 = LINE ( 'NONE', #23085, #11987 ) ;
#6285 = EDGE_CURVE ( 'NONE', #29184, #10769, #37053, .T. ) ;
#6286 = VECTOR ( 'NONE', #39124, 1000.000000000000000 ) ;
#6287 = VECTOR ( 'NONE', #5500, 1000.000000000000000 ) ;
#6288 = CARTESIAN_POINT ( 'NONE',  ( -339.1964088526558498, -123.5000000000000284, 0.000000000000000000 ) ) ;
#6289 = DIRECTION ( 'NONE',  ( 0.000000000000000000, 0.000000000000000000, 1.000000000000000000 ) ) ;
#6290 = ORIENTED_EDGE ( 'NONE', *, *, #9346, .F. ) ;
#6291 = VECTOR ( 'NONE', #44469, 1000.000000000000000 ) ;
#6292 = DIRECTION ( 'NONE',  ( -0.000000000000000000, 1.000000000000000000, -0.000000000000000000 ) ) ;
#6293 = EDGE_LOOP ( 'NONE', ( #40979, #41856, #10012, #10206 ) ) ;
#6294 = CARTESIAN_POINT ( 'NONE',  ( -172.2289551866394106, -189.7472609257535510, -17.63462396184707970 ) ) ;
#6295 = ORIENTED_EDGE ( 'NONE', *, *, #12471, .T. ) ;
#6296 = AXIS2_PLACEMENT_3D ( 'NONE', #50977, #27031, #39624 ) ;
#6297 = CARTESIAN_POINT ( 'NONE',  ( -305.0000000000000568, -181.6348283828473029, -14.84391218300937787 ) ) ;
#6298 = VECTOR ( 'NONE', #43472, 999.9999999999998863 ) ;
#6299 = LINE ( 'NONE', #22317, #8258 ) ;
#6300 = PRODUCT_DEFINITION_SHAPE ( 'NONE', 'NONE',  #34451 ) ;
#6301 = CARTESIAN_POINT ( 'NONE',  ( -336.3521761649654422, -65.58448481710581746, 11.56382487286456140 ) ) ;
#6302 = VERTEX_POINT ( 'NONE', #49402 ) ;
#6305 = EDGE_LOOP ( 'NONE', ( #21020, #18478 ) ) ;
#6304 = CARTESIAN_POINT ( 'NONE',  ( 6.039888445539280504, -177.1207230881787780, 111.3726929437940498 ) ) ;
#6303 = CARTESIAN_POINT ( 'NONE',  ( -3.872148122484094124, 52.31912714116830898, -19.87261434340792121 ) ) ;
#6306 = FACE_OUTER_BOUND ( 'NONE', #42503, .T. ) ;
#6307 = ORIENTED_EDGE ( 'NONE', *, *, #12124, .F. ) ;
#6308 = FACE_OUTER_BOUND ( 'NONE', #45390, .T. ) ;
#6309 = VERTEX_POINT ( 'NONE', #37029 ) ;
#6310 = EDGE_CURVE ( 'NONE', #47750, #19173, #13386, .T. ) ;
#6311 = EDGE_CURVE ( 'NONE', #15743, #32651, #21537, .T. ) ;
#6312 = FACE_OUTER_BOUND ( 'NONE', #11195, .T. ) ;
#6315 = ORIENTED_EDGE ( 'NONE', *, *, #24543, .F. ) ;
#6314 = CARTESIAN_POINT ( 'NONE',  ( 56.77503207194101265, -189.7472609257535510, -67.42819922234311036 ) ) ;
#6313 = DIRECTION ( 'NONE',  ( 0.000000000000000000, 0.000000000000000000, 1.000000000000000000 ) ) ;
#6316 = ORIENTED_EDGE ( 'NONE', *, *, #807, .F. ) ;
#6317 = CARTESIAN_POINT ( 'NONE',  ( -336.3521761649654422, -104.1045282520827300, -55.74477592174792306 ) ) ;
#6318 = ORIENTED_EDGE ( 'NONE', *, *, #31762, .F. ) ;
#6319 = CARTESIAN_POINT ( 'NONE',  ( -147.6585554144535024, -177.1207230881787780, 76.08180419845386666 ) ) ;
#6320 = VECTOR ( 'NONE', #25076, 1000.000000000000000 ) ;
#6321 = LINE ( 'NONE', #34431, #18137 ) ;
#6322 = ORIENTED_EDGE ( 'NONE', *, *, #26528, .F. ) ;
#6323 = LINE ( 'NONE', #14726, #10436 ) ;
#6324 = CARTESIAN_POINT ( 'NONE',  ( -49.32472275501067571, -183.6283474603465606, -0.5338233779647935107 ) ) ;
#6325 = FACE_OUTER_BOUND ( 'NONE', #29148, .T. ) ;
#6326 = DIRECTION ( 'NONE',  ( 0.000000000000000000, 1.000000000000000000, 0.000000000000000000 ) ) ;
#6327 = CIRCLE ( 'NONE', #35678, 125.0000000000000000 ) ;
#6328 = DIRECTION ( 'NONE',  ( 0.000000000000000000, 0.000000000000000000, 1.000000000000000000 ) ) ;
#6329 = VERTEX_POINT ( 'NONE', #37807 ) ;
#6330 = EDGE_CURVE ( 'NONE', #9868, #11130, #48820, .T. ) ;
#6331 = DIRECTION ( 'NONE',  ( -0.000000000000000000, 1.000000000000000000, 0.000000000000000000 ) ) ;
#6333 = VECTOR ( 'NONE', #21203, 1000.000000000000114 ) ;
#6332 = CARTESIAN_POINT ( 'NONE',  ( -53.47502265695602119, -183.6283474603465606, -124.9001241957025883 ) ) ;
#6334 = ADVANCED_FACE ( 'NONE', ( #48880 ), #39298, .T. ) ;
#6335 = DIRECTION ( 'NONE',  ( 0.000000000000000000, 0.000000000000000000, 1.000000000000000000 ) ) ;
#6336 = EDGE_LOOP ( 'NONE', ( #50130, #36327, #5345, #50659 ) ) ;
#6337 = EDGE_CURVE ( 'NONE', #43448, #32451, #50880, .T. ) ;
#6338 = DIRECTION ( 'NONE',  ( -0.9720229140804107493, 0.000000000000000000, -0.2348860457809842095 ) ) ;
#6339 = LINE ( 'NONE', #13964, #42029 ) ;
#6340 = VECTOR ( 'NONE', #27225, 1000.000000000000000 ) ;
#6341 = AXIS2_PLACEMENT_3D ( 'NONE', #31093, #35048, #7188 ) ;
#6342 = EDGE_CURVE ( 'NONE', #13387, #2972, #32023, .T. ) ;
#6343 = DIRECTION ( 'NONE',  ( 0.000000000000000000, 0.000000000000000000, 1.000000000000000000 ) ) ;
#6344 = CYLINDRICAL_SURFACE ( 'NONE', #31668, 125.0000000000000000 ) ;
#6345 = VERTEX_POINT ( 'NONE', #23282 ) ;
#6346 = VECTOR ( 'NONE', #5023, 1000.000000000000000 ) ;
#6347 = CARTESIAN_POINT ( 'NONE',  ( -48.47912675150885065, -175.3837268820161057, 6.938893903907228378E-15 ) ) ;
#6348 = AXIS2_PLACEMENT_3D ( 'NONE', #34789, #46647, #41718 ) ;
#6349 = DIRECTION ( 'NONE',  ( -0.000000000000000000, 1.000000000000000000, -0.000000000000000000 ) ) ;
#6350 = CARTESIAN_POINT ( 'NONE',  ( -5.732832253866456007, -189.7472609257535510, -117.4638425504666657 ) ) ;
#6351 = DIRECTION ( 'NONE',  ( 0.9266896074318343723, 0.000000000000000000, -0.3758275821142357809 ) ) ;
#6352 = ORIENTED_EDGE ( 'NONE', *, *, #29349, .T. ) ;
#6353 = CARTESIAN_POINT ( 'NONE',  ( 0.000000000000000000, -66.21443277186274656, 14.11962419296515137 ) ) ;
#6354 = LINE ( 'NONE', #14762, #47302 ) ;
#6356 = ORIENTED_EDGE ( 'NONE', *, *, #6450, .F. ) ;
#6355 = DIRECTION ( 'NONE',  ( 0.000000000000000000, 0.000000000000000000, 1.000000000000000000 ) ) ;
#6357 = ORIENTED_EDGE ( 'NONE', *, *, #51794, .F. ) ;
#6358 = VECTOR ( 'NONE', #28984, 1000.000000000000000 ) ;
#6359 = ORIENTED_EDGE ( 'NONE', *, *, #25945, .F. ) ;
#6360 = CARTESIAN_POINT ( 'NONE',  ( -336.3521761649654422, -181.4155151828941825, -11.56382487286496463 ) ) ;
#6361 = VECTOR ( 'NONE', #14012, 1000.000000000000000 ) ;
#6362 = VECTOR ( 'NONE', #4256, 1000.000000000000000 ) ;
#6363 = DIRECTION ( 'NONE',  ( 0.000000000000000000, 0.000000000000000000, 1.000000000000000000 ) ) ;
#6364 = CARTESIAN_POINT ( 'NONE',  ( 75.78974234412359579, -177.1207230881787780, 13.49993235881448861 ) ) ;
#6365 = ORIENTED_EDGE ( 'NONE', *, *, #45942, .F. ) ;
#6366 = EDGE_CURVE ( 'NONE', #20647, #17499, #16923, .T. ) ;
#6367 = CARTESIAN_POINT ( 'NONE',  ( -145.4373324222574126, -175.3837268820161057, -78.89300572996837957 ) ) ;
#6368 = LINE ( 'NONE', #50517, #30261 ) ;
#6371 = ORIENTED_EDGE ( 'NONE', *, *, #34209, .T. ) ;
#6370 = PLANE ( 'NONE',  #8995 ) ;
#6369 = CARTESIAN_POINT ( 'NONE',  ( -48.47912675150885065, -175.3837268820161057, 6.938893903907228378E-15 ) ) ;
#6372 = AXIS2_PLACEMENT_3D ( 'NONE', #8181, #32862, #20791 ) ;
#6373 = CIRCLE ( 'NONE', #22305, 60.00000000000000000 ) ;
#6374 = FACE_OUTER_BOUND ( 'NONE', #37032, .T. ) ;
#6375 = VERTEX_POINT ( 'NONE', #27720 ) ;
#6376 = CARTESIAN_POINT ( 'NONE',  ( -164.0008810331606526, -193.5000000000000000, 47.74645837849825369 ) ) ;
#6377 = EDGE_LOOP ( 'NONE', ( #40567, #46089, #36199, #39281 ) ) ;
#6378 = ADVANCED_FACE ( 'NONE', ( #30899 ), #43505, .T. ) ;
#6379 = EDGE_CURVE ( 'NONE', #4823, #44074, #6985, .T. ) ;
#6380 = ADVANCED_FACE ( 'NONE', ( #47447 ), #3302, .F. ) ;
#6381 = DIRECTION ( 'NONE',  ( 0.000000000000000000, -1.000000000000000000, -0.000000000000000000 ) ) ;
#6382 = VECTOR ( 'NONE', #27370, 1000.000000000000000 ) ;
#6383 = LINE ( 'NONE', #46329, #10384 ) ;
#6384 = PLANE ( 'NONE',  #41667 ) ;
#6385 = EDGE_CURVE ( 'NONE', #41503, #11325, #3811, .T. ) ;
#6386 = AXIS2_PLACEMENT_3D ( 'NONE', #38222, #36463, #9156 ) ;
#6387 = EDGE_LOOP ( 'NONE', ( #20848, #51335, #38619, #29608 ) ) ;
#6388 = CARTESIAN_POINT ( 'NONE',  ( -47.87232660569025455, -183.6283474603465606, -0.7948544414133454916 ) ) ;
#6389 = CARTESIAN_POINT ( 'NONE',  ( 45.36094686508022988, -193.5000000000000000, -82.57748230379237953 ) ) ;
#6390 = VERTEX_POINT ( 'NONE', #39540 ) ;
#6391 = ADVANCED_FACE ( 'NONE', ( #42976 ), #11427, .F. ) ;
#6392 = CARTESIAN_POINT ( 'NONE',  ( -46.00000000000000711, 20.00000000000000000, 41.00000000000000000 ) ) ;
#6393 = DIRECTION ( 'NONE',  ( 0.000000000000000000, -1.000000000000000000, 0.000000000000000000 ) ) ;
#6394 = VERTEX_POINT ( 'NONE', #11943 ) ;
#6395 = FACE_BOUND ( 'NONE', #32784, .T. ) ;
#6396 = EDGE_CURVE ( 'NONE', #11174, #15087, #2773, .T. ) ;
#6397 = CARTESIAN_POINT ( 'NONE',  ( -134.7293151056888973, -193.5000000000000000, -89.08931047202574405 ) ) ;
#6398 = EDGE_CURVE ( 'NONE', #23283, #41966, #3549, .T. ) ;
#6399 = ORIENTED_EDGE ( 'NONE', *, *, #42488, .F. ) ;
#6400 = CARTESIAN_POINT ( 'NONE',  ( -339.1964088526558498, -179.4217241332781043, 21.74306257088782601 ) ) ;
#6401 = ORIENTED_EDGE ( 'NONE', *, *, #31537, .T. ) ;
#6402 = VECTOR ( 'NONE', #27831, 1000.000000000000000 ) ;
#6403 = AXIS2_PLACEMENT_3D ( 'NONE', #26477, #37548, #1791 ) ;
#6404 = ADVANCED_FACE ( 'NONE', ( #19582 ), #47193, .T. ) ;
#6405 = DIRECTION ( 'NONE',  ( 0.000000000000000000, 0.000000000000000000, -1.000000000000000000 ) ) ;
#6406 = CARTESIAN_POINT ( 'NONE',  ( -49.30901192927172616, -189.7472609257535510, -124.9972451320097093 ) ) ;
#6407 = ORIENTED_EDGE ( 'NONE', *, *, #18495, .F. ) ;
#6408 = VECTOR ( 'NONE', #43149, 1000.000000000000000 ) ;
#6409 = EDGE_CURVE ( 'NONE', #43249, #41296, #11694, .T. ) ;
#6410 = DIRECTION ( 'NONE',  ( -0.000000000000000000, 0.7485107481710999711, -0.6631226582407964143 ) ) ;
#6411 = DIRECTION ( 'NONE',  ( 0.000000000000000000, 0.000000000000000000, 1.000000000000000000 ) ) ;
#6412 = DIRECTION ( 'NONE',  ( -0.5829794791144703447, 0.000000000000000000, -0.8124868780056825335 ) ) ;
#6413 = ADVANCED_FACE ( 'NONE', ( #14887 ), #27194, .T. ) ;
#6414 = ORIENTED_EDGE ( 'NONE', *, *, #22808, .F. ) ;
#6415 = CARTESIAN_POINT ( 'NONE',  ( 75.37518750349086361, -183.6283474603465606, 6.025661128238926523 ) ) ;
#6416 = EDGE_CURVE ( 'NONE', #12390, #46128, #35470, .T. ) ;
#6417 = ORIENTED_EDGE ( 'NONE', *, *, #31098, .F. ) ;
#6418 = AXIS2_PLACEMENT_3D ( 'NONE', #31847, #294, #4512 ) ;
#6419 = DIRECTION ( 'NONE',  ( 0.000000000000000000, -1.110223024625156540E-13, 1.000000000000000000 ) ) ;
#6420 = DIRECTION ( 'NONE',  ( 0.6068001458185945385, 0.000000000000000000, -0.7948544414133523750 ) ) ;
#6422 = VERTEX_POINT ( 'NONE', #7242 ) ;
#6421 = LINE ( 'NONE', #26638, #17788 ) ;
#6423 = VECTOR ( 'NONE', #34502, 1000.000000000000114 ) ;
#6424 = AXIS2_PLACEMENT_3D ( 'NONE', #46793, #7606, #19186 ) ;
#6425 = ORIENTED_EDGE ( 'NONE', *, *, #36160, .T. ) ;
#6426 = FACE_OUTER_BOUND ( 'NONE', #5384, .T. ) ;
#6427 = AXIS2_PLACEMENT_3D ( 'NONE', #39897, #7854, #14990 ) ;
#6428 = EDGE_CURVE ( 'NONE', #3536, #9877, #51155, .T. ) ;
#6429 = AXIS2_PLACEMENT_3D ( 'NONE', #22203, #20444, #1248 ) ;
#6430 = CARTESIAN_POINT ( 'NONE',  ( -336.3521761649654422, -169.4076645216271402, -37.15394033962039089 ) ) ;
#6431 = EDGE_LOOP ( 'NONE', ( #28342, #25188, #51710, #37432 ) ) ;
#6432 = DIRECTION ( 'NONE',  ( 0.000000000000000000, 1.000000000000000000, 0.000000000000000000 ) ) ;
#6433 = ORIENTED_EDGE ( 'NONE', *, *, #34379, .T. ) ;
#6434 = DIRECTION ( 'NONE',  ( -0.000000000000000000, 1.000000000000000000, -0.000000000000000000 ) ) ;
#6435 = DIRECTION ( 'NONE',  ( -0.000000000000000000, 1.000000000000000000, -0.000000000000000000 ) ) ;
#6436 = DIRECTION ( 'NONE',  ( -0.9995608365087942371, 0.000000000000000000, -0.02963332782256331357 ) ) ;
#6437 = CARTESIAN_POINT ( 'NONE',  ( -172.3973245609188041, -189.7472609257535510, 4.503971736581616092 ) ) ;
#6438 = ORIENTED_EDGE ( 'NONE', *, *, #6090, .T. ) ;
#6439 = EDGE_LOOP ( 'NONE', ( #30318, #20963, #36531, #51193 ) ) ;
#6440 = ORIENTED_EDGE ( 'NONE', *, *, #47267, .T. ) ;
#6441 = CARTESIAN_POINT ( 'NONE',  ( -44.48323084606168720, -177.1207230881787780, 124.9361149384469769 ) ) ;
#6442 = DIRECTION ( 'NONE',  ( -0.3758275821142357809, 0.000000000000000000, -0.9266896074318343723 ) ) ;
#6443 = AXIS2_PLACEMENT_3D ( 'NONE', #8579, #37480, #40898 ) ;
#6444 = AXIS2_PLACEMENT_3D ( 'NONE', #22947, #27390, #51575 ) ;
#6445 = CARTESIAN_POINT ( 'NONE',  ( 22.03849146056077757, -189.7472609257535510, 103.2098131075567267 ) ) ;
#6446 = CARTESIAN_POINT ( 'NONE',  ( -70.42295845586433245, -175.3837268820161057, -123.0587999703024877 ) ) ;
#6447 = ORIENTED_EDGE ( 'NONE', *, *, #28497, .F. ) ;
#6448 = VECTOR ( 'NONE', #8706, 1000.000000000000114 ) ;
#6449 = EDGE_CURVE ( 'NONE', #44354, #30980, #4329, .T. ) ;
#6450 = EDGE_CURVE ( 'NONE', #23517, #17429, #10319, .T. ) ;
#6451 = CARTESIAN_POINT ( 'NONE',  ( 116.9235303384055840, -213.5000000000000000, 2.819679052520814125E-14 ) ) ;
#6452 = EDGE_CURVE ( 'NONE', #27857, #13909, #36914, .T. ) ;
#6453 = EDGE_CURVE ( 'NONE', #33588, #35501, #20897, .T. ) ;
#6454 = ORIENTED_EDGE ( 'NONE', *, *, #30997, .T. ) ;
#6455 = ORIENTED_EDGE ( 'NONE', *, *, #50367, .T. ) ;
#6456 = VECTOR ( 'NONE', #19605, 1000.000000000000227 ) ;
#6457 = LINE ( 'NONE', #30343, #36561 ) ;
#6458 = DIRECTION ( 'NONE',  ( 0.000000000000000000, -0.000000000000000000, 1.000000000000000000 ) ) ;
#6459 = VECTOR ( 'NONE', #27823, 1000.000000000000114 ) ;
#6460 = FACE_OUTER_BOUND ( 'NONE', #23720, .T. ) ;
#6461 = AXIS2_PLACEMENT_3D ( 'NONE', #41940, #49327, #37993 ) ;
#6462 = AXIS2_PLACEMENT_3D ( 'NONE', #33727, #1675, #46095 ) ;
#6463 = LINE ( 'NONE', #30597, #27069 ) ;
#6464 = DIRECTION ( 'NONE',  ( 0.000000000000000000, -0.6631226582407989678, -0.7485107481710977506 ) ) ;
#6465 = ORIENTED_EDGE ( 'NONE', *, *, #46499, .F. ) ;
#6466 = PLANE ( 'NONE',  #13292 ) ;
#6467 = AXIS2_PLACEMENT_3D ( 'NONE', #28761, #16446, #32464 ) ;
#6468 = AXIS2_PLACEMENT_3D ( 'NONE', #15552, #24728, #24217 ) ;
#6469 = ORIENTED_EDGE ( 'NONE', *, *, #11964, .F. ) ;
#6470 = DIRECTION ( 'NONE',  ( -0.000000000000000000, 1.000000000000000000, -0.000000000000000000 ) ) ;
#6471 = ADVANCED_FACE ( 'NONE', ( #48749 ), #20352, .T. ) ;
#6472 = DIRECTION ( 'NONE',  ( -0.000000000000000000, 0.8854560256532157947, 0.4647231720437573488 ) ) ;
#6473 = VERTEX_POINT ( 'NONE', #900 ) ;
#6474 = LINE ( 'NONE', #10138, #5562 ) ;
#6475 = DIRECTION ( 'NONE',  ( 0.000000000000000000, -1.000000000000000000, 0.000000000000000000 ) ) ;
#6476 = FACE_OUTER_BOUND ( 'NONE', #30900, .T. ) ;
#6477 = FACE_OUTER_BOUND ( 'NONE', #9992, .T. ) ;
#6478 = EDGE_CURVE ( 'NONE', #51370, #43010, #26135, .T. ) ;
#6479 = DIRECTION ( 'NONE',  ( -0.000000000000000000, 1.000000000000000000, -0.000000000000000000 ) ) ;
#6480 = ORIENTED_EDGE ( 'NONE', *, *, #26832, .F. ) ;
#6481 = VECTOR ( 'NONE', #20889, 999.9999999999998863 ) ;
#6482 = CONICAL_SURFACE ( 'NONE', #16570, 20.00000000000000355, 0.4363323129985833826 ) ;
#6483 = LINE ( 'NONE', #11426, #18065 ) ;
#6484 = EDGE_LOOP ( 'NONE', ( #15899, #7817, #13656, #8024 ) ) ;
#6485 = AXIS2_PLACEMENT_3D ( 'NONE', #7698, #23978, #28431 ) ;
#6486 = ORIENTED_EDGE ( 'NONE', *, *, #11588, .F. ) ;
#6487 = ORIENTED_EDGE ( 'NONE', *, *, #43277, .F. ) ;
#6488 = DIRECTION ( 'NONE',  ( -0.000000000000000000, -0.000000000000000000, 1.000000000000000000 ) ) ;
#6489 = VECTOR ( 'NONE', #6697, 1000.000000000000000 ) ;
#6490 = ORIENTED_EDGE ( 'NONE', *, *, #13966, .T. ) ;
#6491 = DIRECTION ( 'NONE',  ( 0.000000000000000000, 0.000000000000000000, -1.000000000000000000 ) ) ;
#6492 = AXIS2_PLACEMENT_3D ( 'NONE', #10560, #37378, #1384 ) ;
#6493 = FACE_OUTER_BOUND ( 'NONE', #29403, .T. ) ;
#6494 = VERTEX_POINT ( 'NONE', #29284 ) ;
#6495 = DIRECTION ( 'NONE',  ( 0.000000000000000000, -0.000000000000000000, -1.000000000000000000 ) ) ;
#6496 = AXIS2_PLACEMENT_3D ( 'NONE', #28127, #44179, #37527 ) ;
#6497 = VECTOR ( 'NONE', #40523, 1000.000000000000000 ) ;
#6498 = DIRECTION ( 'NONE',  ( -0.000000000000000000, 1.000000000000000000, -0.000000000000000000 ) ) ;
#6499 = CARTESIAN_POINT ( 'NONE',  ( -50.83192613281184435, -177.1207230881787780, 123.9784823535113816 ) ) ;
#6500 = VERTEX_POINT ( 'NONE', #45336 ) ;
#6501 = ORIENTED_EDGE ( 'NONE', *, *, #14914, .T. ) ;
#6502 = ORIENTED_EDGE ( 'NONE', *, *, #34896, .F. ) ;
#6503 = AXIS2_PLACEMENT_3D ( 'NONE', #7087, #35192, #47299 ) ;
#6504 = DIRECTION ( 'NONE',  ( 0.000000000000000000, -0.1205366802553130001, 0.9927088740980553050 ) ) ;
#6505 = DIRECTION ( 'NONE',  ( 0.9374196611341231167, 0.000000000000000000, -0.3482016354343928088 ) ) ;
#6506 = DIRECTION ( 'NONE',  ( -0.000000000000000000, 1.047444401652940007E-14, 1.000000000000000000 ) ) ;
#6507 = DIRECTION ( 'NONE',  ( 1.000000000000000000, 0.000000000000000000, 0.000000000000000000 ) ) ;
#6508 = CARTESIAN_POINT ( 'NONE',  ( 0.000000000000000000, -182.5000000000000568, 0.000000000000000000 ) ) ;
#6509 = EDGE_LOOP ( 'NONE', ( #41874, #45923, #24253, #35591 ) ) ;
#6510 = EDGE_CURVE ( 'NONE', #15990, #4438, #39557, .T. ) ;
#6511 = DIRECTION ( 'NONE',  ( -1.000000000000000000, 0.000000000000000000, 0.000000000000000000 ) ) ;
#6512 = ORIENTED_EDGE ( 'NONE', *, *, #33950, .T. ) ;
#6514 = ORIENTED_EDGE ( 'NONE', *, *, #46798, .T. ) ;
#6513 = DIRECTION ( 'NONE',  ( 0.000000000000000000, 1.000000000000000000, 0.000000000000000000 ) ) ;
#6515 = AXIS2_PLACEMENT_3D ( 'NONE', #535, #31183, #6770 ) ;
#6516 = ORIENTED_EDGE ( 'NONE', *, *, #40377, .T. ) ;
#6517 = AXIS2_PLACEMENT_3D ( 'NONE', #43081, #34927, #43852 ) ;
#6518 = DIRECTION ( 'NONE',  ( -0.6528221181905119463, 0.000000000000000000, -0.7575112421616284619 ) ) ;
#6519 = EDGE_LOOP ( 'NONE', ( #39329, #13051, #26272, #5545 ) ) ;
#6520 = DIRECTION ( 'NONE',  ( -0.6965510290629882695, 0.000000000000000000, -0.7175072570443395970 ) ) ;
#6521 = DIRECTION ( 'NONE',  ( 0.000000000000000000, 0.000000000000000000, -1.000000000000000000 ) ) ;
#6522 = LINE ( 'NONE', #22550, #6649 ) ;
#6523 = ORIENTED_EDGE ( 'NONE', *, *, #39098, .F. ) ;
#6524 = LINE ( 'NONE', #10440, #3203 ) ;
#6525 = ORIENTED_EDGE ( 'NONE', *, *, #19554, .F. ) ;
#6526 = ORIENTED_EDGE ( 'NONE', *, *, #8789, .T. ) ;
#6527 = DIRECTION ( 'NONE',  ( -1.000000000000000000, -0.000000000000000000, 0.000000000000000000 ) ) ;
#6528 = AXIS2_PLACEMENT_3D ( 'NONE', #10874, #26893, #42924 ) ;
#6529 = DIRECTION ( 'NONE',  ( 0.000000000000000000, 1.000000000000000000, -0.000000000000000000 ) ) ;
#6530 = AXIS2_PLACEMENT_3D ( 'NONE', #1591, #37840, #41513 ) ;
#6531 = ADVANCED_FACE ( 'NONE', ( #40063 ), #32954, .T. ) ;
#6532 = DIRECTION ( 'NONE',  ( 0.6749830015182038956, 0.000000000000000000, 0.7378332790417333475 ) ) ;
#6533 = VERTEX_POINT ( 'NONE', #12979 ) ;
#6534 = CIRCLE ( 'NONE', #8164, 125.0000000000000000 ) ;
#6535 = DIRECTION ( 'NONE',  ( 0.9646355819083594074, 0.000000000000000000, -0.2635871660690647933 ) ) ;
#6536 = DIRECTION ( 'NONE',  ( 0.4566292373937140270, 0.000000000000000000, -0.8896570909947467687 ) ) ;
#6537 = CARTESIAN_POINT ( 'NONE',  ( -48.47912675150885065, -183.6283474603465606, 6.938893903907228378E-15 ) ) ;
#6538 = LINE ( 'NONE', #49896, #9461 ) ;
#6539 = VECTOR ( 'NONE', #1338, 1000.000000000000000 ) ;
#6540 = ORIENTED_EDGE ( 'NONE', *, *, #33153, .F. ) ;
#6541 = LINE ( 'NONE', #22566, #6215 ) ;
#6542 = CARTESIAN_POINT ( 'NONE',  ( -47.57632892154311577, -189.7472609257535510, 0.4300652022765314997 ) ) ;
#6543 = AXIS2_PLACEMENT_3D ( 'NONE', #48326, #24406, #12309 ) ;
#6544 = CARTESIAN_POINT ( 'NONE',  ( -173.0563034899574859, -175.3837268820161057, -10.27263529369816908 ) ) ;
#6545 = EDGE_LOOP ( 'NONE', ( #12020, #28109, #18932, #2744 ) ) ;
#6546 = CARTESIAN_POINT ( 'NONE',  ( -172.5669052183642123, -183.6283474603465606, 15.07392567185546994 ) ) ;
#6547 = FACE_OUTER_BOUND ( 'NONE', #42409, .T. ) ;
#6548 = ORIENTED_EDGE ( 'NONE', *, *, #40003, .F. ) ;
#6549 = CARTESIAN_POINT ( 'NONE',  ( 46.40005841627164074, -193.5000000000000000, 81.38144888055276738 ) ) ;
#6550 = EDGE_CURVE ( 'NONE', #38627, #9866, #36382, .T. ) ;
#6551 = ORIENTED_EDGE ( 'NONE', *, *, #18064, .T. ) ;
#6552 = AXIS2_PLACEMENT_3D ( 'NONE', #43986, #7732, #35574 ) ;
#6553 = CARTESIAN_POINT ( 'NONE',  ( -46.00000000000000711, 0.000000000000000000, 46.00000000000000000 ) ) ;
#6554 = AXIS2_PLACEMENT_3D ( 'NONE', #9614, #37203, #21439 ) ;
#6555 = DIRECTION ( 'NONE',  ( 0.000000000000000000, -0.5680647467311569221, -0.8229838658936556861 ) ) ;
#6556 = CARTESIAN_POINT ( 'NONE',  ( -170.0000000000000284, -93.50000000000001421, -51.54700538379269403 ) ) ;
#6557 = VECTOR ( 'NONE', #12669, 1000.000000000000000 ) ;
#6558 = DIRECTION ( 'NONE',  ( 0.000000000000000000, -3.491481338843133355E-15, -1.000000000000000000 ) ) ;
#6559 = CARTESIAN_POINT ( 'NONE',  ( -149.7090673587773040, -189.7472609257535510, -71.61357856150524981 ) ) ;
#6560 = ORIENTED_EDGE ( 'NONE', *, *, #50850, .F. ) ;
#6561 = FACE_OUTER_BOUND ( 'NONE', #21554, .T. ) ;
#6562 = EDGE_CURVE ( 'NONE', #49503, #30910, #4086, .T. ) ;
#6563 = VERTEX_POINT ( 'NONE', #29007 ) ;
#6564 = DIRECTION ( 'NONE',  ( -0.000000000000000000, 1.000000000000000000, -0.000000000000000000 ) ) ;
#6565 = CIRCLE ( 'NONE', #13270, 5.000000000000001776 ) ;
#6566 = ORIENTED_EDGE ( 'NONE', *, *, #51638, .T. ) ;
#6567 = DIRECTION ( 'NONE',  ( -0.000000000000000000, 1.000000000000000000, -0.000000000000000000 ) ) ;
#6568 = EDGE_CURVE ( 'NONE', #19715, #48288, #42083, .T. ) ;
#6569 = VECTOR ( 'NONE', #23607, 1000.000000000000114 ) ;
#6570 = CARTESIAN_POINT ( 'NONE',  ( 26.52087324849106054, -198.5000000000000000, -70.00000000000002842 ) ) ;
#6571 = PLANE ( 'NONE',  #50800 ) ;
#6572 = VERTEX_POINT ( 'NONE', #5124 ) ;
#6575 = EDGE_LOOP ( 'NONE', ( #15819, #43317, #50116, #14487 ) ) ;
#6574 = PLANE ( 'NONE',  #32307 ) ;
#6573 = CARTESIAN_POINT ( 'NONE',  ( -4.232179330832529729, 52.95513942278812181, -19.37560274765787938 ) ) ;
#6576 = ADVANCED_FACE ( 'NONE', ( #21133 ), #12205, .T. ) ;
#6577 = CARTESIAN_POINT ( 'NONE',  ( 53.18081239921338010, -189.7472609257535510, -72.73415134495935774 ) ) ;
#6578 = VERTEX_POINT ( 'NONE', #25099 ) ;
#6579 = CARTESIAN_POINT ( 'NONE',  ( 9.336583202542589888, -189.7472609257535510, 110.8257356506556306 ) ) ;
#6580 = ORIENTED_EDGE ( 'NONE', *, *, #35916, .F. ) ;
#6581 = LINE ( 'NONE', #14208, #9085 ) ;
#6584 = ORIENTED_EDGE ( 'NONE', *, *, #113, .T. ) ;
#6583 = FACE_OUTER_BOUND ( 'NONE', #2062, .T. ) ;
#6582 = DIRECTION ( 'NONE',  ( -0.000000000000000000, 0.7485107481711089639, 0.6631226582407863113 ) ) ;
#6585 = ORIENTED_EDGE ( 'NONE', *, *, #37619, .F. ) ;
#6586 = FACE_OUTER_BOUND ( 'NONE', #20715, .T. ) ;
#6587 = ORIENTED_EDGE ( 'NONE', *, *, #31167, .T. ) ;
#6588 = DIRECTION ( 'NONE',  ( 0.000000000000000000, -0.9927088740980548609, -0.1205366802553164696 ) ) ;
#6589 = VECTOR ( 'NONE', #23766, 1000.000000000000000 ) ;
#6590 = LINE ( 'NONE', #30734, #32374 ) ;
#6591 = ORIENTED_EDGE ( 'NONE', *, *, #11202, .F. ) ;
#6592 = COLOUR_RGB ( '', 0.66274510, 0.83137255, 0.94901961) ;
#6593 = EDGE_CURVE ( 'NONE', #34577, #29760, #32449, .T. ) ;
#6594 = DIRECTION ( 'NONE',  ( 0.000000000000000000, 0.8229838658936575735, 0.5680647467311540355 ) ) ;
#6595 = CARTESIAN_POINT ( 'NONE',  ( -336.3521761649654422, -77.59233547837267508, 37.15394033962009246 ) ) ;
#6596 = CARTESIAN_POINT ( 'NONE',  ( 116.9235303384055840, -213.5000000000000000, 10.00000000000000000 ) ) ;
#6597 = LINE ( 'NONE', #46284, #42758 ) ;
#6598 = AXIS2_PLACEMENT_3D ( 'NONE', #6872, #2921, #26576 ) ;
#6599 = FACE_OUTER_BOUND ( 'NONE', #50697, .T. ) ;
#6600 = ORIENTED_EDGE ( 'NONE', *, *, #45926, .F. ) ;
#6601 = CARTESIAN_POINT ( 'NONE',  ( -305.0000000000000568, -168.0775241366797275, 40.16023333901010517 ) ) ;
#6602 = DIRECTION ( 'NONE',  ( -0.000000000000000000, 1.000000000000000000, -0.000000000000000000 ) ) ;
#6603 = DIRECTION ( 'NONE',  ( -0.000000000000000000, -0.8229838658936516893, 0.5680647467311626952 ) ) ;
#6604 = ORIENTED_EDGE ( 'NONE', *, *, #43586, .F. ) ;
#6605 = AXIS2_PLACEMENT_3D ( 'NONE', #18055, #2017, #5463 ) ;
#6606 = CARTESIAN_POINT ( 'NONE',  ( 141.7825277784304205, -213.5000000000000000, 10.00000000000000178 ) ) ;
#6607 = DIRECTION ( 'NONE',  ( -0.000000000000000000, 1.000000000000000000, -0.000000000000000000 ) ) ;
#6608 = DIRECTION ( 'NONE',  ( -0.000000000000000000, -1.000000000000000000, 0.000000000000000000 ) ) ;
#6609 = LINE ( 'NONE', #18685, #40016 ) ;
#6610 = ORIENTED_EDGE ( 'NONE', *, *, #16364, .T. ) ;
#6611 = AXIS2_PLACEMENT_3D ( 'NONE', #19172, #35190, #31501 ) ;
#6612 = CARTESIAN_POINT ( 'NONE',  ( -117.6101668435555325, -189.7472609257535510, -102.9412430821794686 ) ) ;
#6613 = CARTESIAN_POINT ( 'NONE',  ( -37.67038537088846084, -177.1207230881787780, -124.5318076226586470 ) ) ;
#6614 = DIRECTION ( 'NONE',  ( -0.000000000000000000, 0.4739294676984008858, 0.8805628084623552398 ) ) ;
#6615 = ORIENTED_EDGE ( 'NONE', *, *, #42974, .T. ) ;
#6616 = ADVANCED_FACE ( 'NONE', ( #44284 ), #37161, .T. ) ;
#6617 = ADVANCED_FACE ( 'NONE', ( #36126 ), #33221, .T. ) ;
#6618 = DIRECTION ( 'NONE',  ( -0.000000000000000000, 1.000000000000000000, -0.000000000000000000 ) ) ;
#6619 = DIRECTION ( 'NONE',  ( 0.000000000000000000, -1.000000000000000000, 0.000000000000000000 ) ) ;
#6620 = VERTEX_POINT ( 'NONE', #13262 ) ;
#6621 = PRODUCT_DEFINITION_FORMATION_WITH_SPECIFIED_SOURCE ( 'ANY', '', #802, .NOT_KNOWN. ) ;
#6622 = AXIS2_PLACEMENT_3D ( 'NONE', #40552, #8762, #12179 ) ;
#6623 = VERTEX_POINT ( 'NONE', #9324 ) ;
#6624 = VECTOR ( 'NONE', #41449, 1000.000000000000000 ) ;
#6625 = VERTEX_POINT ( 'NONE', #29534 ) ;
#6626 = DIRECTION ( 'NONE',  ( -1.000000000000000000, 0.000000000000000000, 0.000000000000000000 ) ) ;
#6627 = VECTOR ( 'NONE', #50701, 1000.000000000000000 ) ;
#6628 = EDGE_CURVE ( 'NONE', #37305, #12850, #38461, .T. ) ;
#6629 = LINE ( 'NONE', #26322, #42124 ) ;
#6630 = CARTESIAN_POINT ( 'NONE',  ( 66.73972540229262052, -189.7472609257535510, 45.83253885719641829 ) ) ;
#6631 = ORIENTED_EDGE ( 'NONE', *, *, #19086, .T. ) ;
#6632 = EDGE_CURVE ( 'NONE', #40491, #19552, #25588, .T. ) ;
#6633 = CARTESIAN_POINT ( 'NONE',  ( -36.09284319799462537, -183.6283474603465606, 124.3848060646152476 ) ) ;
#6634 = DIRECTION ( 'NONE',  ( -8.718379230999707126E-17, 0.9709418174260511236, -0.2393156642875615969 ) ) ;
#6635 = AXIS2_PLACEMENT_3D ( 'NONE', #25677, #37506, #5205 ) ;
#6638 = ORIENTED_EDGE ( 'NONE', *, *, #29564, .T. ) ;
#6637 = CARTESIAN_POINT ( 'NONE',  ( -339.1964088526558498, -180.6659093959932250, 14.60509510167942437 ) ) ;
#6636 = FACE_OUTER_BOUND ( 'NONE', #48462, .T. ) ;
#6639 = EDGE_CURVE ( 'NONE', #25286, #17442, #30064, .T. ) ;
#6640 = DIRECTION ( 'NONE',  ( 0.000000000000000000, 0.000000000000000000, 1.000000000000000000 ) ) ;
#6641 = ORIENTED_EDGE ( 'NONE', *, *, #15329, .T. ) ;
#6642 = CARTESIAN_POINT ( 'NONE',  ( -117.6101668435555325, -175.3837268820161057, -102.9412430821794686 ) ) ;
#6643 = EDGE_CURVE ( 'NONE', #31627, #47473, #5381, .T. ) ;
#6644 = ORIENTED_EDGE ( 'NONE', *, *, #37671, .F. ) ;
#6645 = CARTESIAN_POINT ( 'NONE',  ( -161.4019114581580823, -193.5000000000000000, 53.60452120946281696 ) ) ;
#6646 = DIRECTION ( 'NONE',  ( -0.000000000000000000, -0.000000000000000000, -1.000000000000000000 ) ) ;
#6647 = CARTESIAN_POINT ( 'NONE',  ( -48.47912675150885065, -188.5000000000000284, -13.99999999999998224 ) ) ;
#6648 = EDGE_LOOP ( 'NONE', ( #40842, #31029, #9021, #50599 ) ) ;
#6649 = VECTOR ( 'NONE', #17820, 1000.000000000000000 ) ;
#6650 = EDGE_LOOP ( 'NONE', ( #1102, #22259, #12251, #45967 ) ) ;
#6651 = CARTESIAN_POINT ( 'NONE',  ( -305.0000000000000568, -180.4803820837415458, -18.79457521708939183 ) ) ;
#6652 = CARTESIAN_POINT ( 'NONE',  ( -160.0666658415768211, -175.3837268820161057, 54.07611884703388228 ) ) ;
#6653 = ORIENTED_EDGE ( 'NONE', *, *, #27363, .F. ) ;
#6654 = FACE_OUTER_BOUND ( 'NONE', #3331, .T. ) ;
#6655 = CARTESIAN_POINT ( 'NONE',  ( -332.3517673607765914, -83.15397741537739762, 43.07972642080338233 ) ) ;
#6656 = EDGE_LOOP ( 'NONE', ( #47850, #42641, #27122, #35908 ) ) ;
#6657 = CARTESIAN_POINT ( 'NONE',  ( -330.4913330509368166, -102.6919536717973926, 56.27632902032055284 ) ) ;
#6658 = FACE_OUTER_BOUND ( 'NONE', #36270, .T. ) ;
#6659 = ORIENTED_EDGE ( 'NONE', *, *, #8503, .F. ) ;
#6660 = LINE ( 'NONE', #30045, #19054 ) ;
#6661 = VERTEX_POINT ( 'NONE', #50044 ) ;
#6662 = CIRCLE ( 'NONE', #4148, 60.00000000000000000 ) ;
#6663 = DIRECTION ( 'NONE',  ( 1.000000000000000000, -0.000000000000000000, -0.000000000000000000 ) ) ;
#6664 = LINE ( 'NONE', #22683, #1745 ) ;
#6665 = ORIENTED_EDGE ( 'NONE', *, *, #16851, .F. ) ;
#6666 = CARTESIAN_POINT ( 'NONE',  ( 60.00000000000001421, -93.50000000000002842, 51.54700538379266561 ) ) ;
#6667 = CARTESIAN_POINT ( 'NONE',  ( -171.9838957966129556, -193.5000000000000000, 19.27620354518722579 ) ) ;
#6668 = CARTESIAN_POINT ( 'NONE',  ( -336.3521761649654422, -172.9832938399466684, -32.17247266903247294 ) ) ;
#6669 = VERTEX_POINT ( 'NONE', #49789 ) ;
#6670 = DIRECTION ( 'NONE',  ( 0.000000000000000000, 0.000000000000000000, 1.000000000000000000 ) ) ;
#6671 = CARTESIAN_POINT ( 'NONE',  ( -339.1964088526558498, -64.86990808808704401, 6.615309698014191220 ) ) ;
#6672 = FACE_OUTER_BOUND ( 'NONE', #25158, .T. ) ;
#6674 = ORIENTED_EDGE ( 'NONE', *, *, #10581, .T. ) ;
#6673 = CARTESIAN_POINT ( 'NONE',  ( -168.6933499419502596, -193.5000000000000000, 30.40954281680882687 ) ) ;
#6675 = EDGE_CURVE ( 'NONE', #19616, #44602, #25863, .T. ) ;
#6676 = ORIENTED_EDGE ( 'NONE', *, *, #24658, .F. ) ;
#6677 = EDGE_CURVE ( 'NONE', #42477, #32555, #30564, .T. ) ;
#6678 = ADVANCED_FACE ( 'NONE', ( #17482 ), #41891, .T. ) ;
#6679 = CARTESIAN_POINT ( 'NONE',  ( -365.0000000000001137, -78.50000000000002842, 5.000000000000001776 ) ) ;
#6680 = EDGE_CURVE ( 'NONE', #7888, #44388, #21670, .T. ) ;
#6681 = AXIS2_PLACEMENT_3D ( 'NONE', #14222, #17897, #30241 ) ;
#6682 = DIRECTION ( 'NONE',  ( 0.000000000000000000, 0.6631226582407885317, -0.7485107481711069655 ) ) ;
#6683 = ORIENTED_EDGE ( 'NONE', *, *, #26926, .T. ) ;
#6684 = DIRECTION ( 'NONE',  ( 0.000000000000000000, -0.8854560256532062468, 0.4647231720437755564 ) ) ;
#6685 = EDGE_CURVE ( 'NONE', #30451, #47556, #5907, .T. ) ;
#6686 = ORIENTED_EDGE ( 'NONE', *, *, #37088, .F. ) ;
#6687 = CARTESIAN_POINT ( 'NONE',  ( -90.87721961371603641, -189.7472609257535510, 116.5264228893328777 ) ) ;
#6688 = CARTESIAN_POINT ( 'NONE',  ( 71.87891646118019651, -193.5000000000000000, -33.74820638215424395 ) ) ;
#6689 = ADVANCED_FACE ( 'NONE', ( #9571 ), #37692, .T. ) ;
#6690 = ADVANCED_FACE ( 'NONE', ( #17731 ), #22445, .F. ) ;
#6691 = DIRECTION ( 'NONE',  ( 0.000000000000000000, 0.000000000000000000, -1.000000000000000000 ) ) ;
#6692 = DIRECTION ( 'NONE',  ( -1.000000000000000000, 4.850383327711829203E-15, -9.241633304753623405E-15 ) ) ;
#6693 = ORIENTED_EDGE ( 'NONE', *, *, #51586, .T. ) ;
#6694 = ORIENTED_EDGE ( 'NONE', *, *, #39111, .F. ) ;
#6695 = EDGE_CURVE ( 'NONE', #15290, #32906, #49539, .T. ) ;
#6696 = VERTEX_POINT ( 'NONE', #30313 ) ;
#6697 = DIRECTION ( 'NONE',  ( -0.6965510290629882695, 0.000000000000000000, -0.7175072570443395970 ) ) ;
#6698 = LINE ( 'NONE', #13799, #6752 ) ;
#6699 = EDGE_CURVE ( 'NONE', #26523, #43006, #9839, .T. ) ;
#6700 = VECTOR ( 'NONE', #46950, 1000.000000000000000 ) ;
#6701 = LINE ( 'NONE', #51122, #10283 ) ;
#6702 = DIRECTION ( 'NONE',  ( 0.000000000000000000, -1.000000000000000000, 0.000000000000000000 ) ) ;
#6703 = VERTEX_POINT ( 'NONE', #1946 ) ;
#6704 = EDGE_CURVE ( 'NONE', #14253, #48059, #22177, .T. ) ;
#6705 = FACE_OUTER_BOUND ( 'NONE', #27629, .T. ) ;
#6706 = FACE_OUTER_BOUND ( 'NONE', #30151, .T. ) ;
#6707 = ORIENTED_EDGE ( 'NONE', *, *, #7167, .T. ) ;
#6708 = EDGE_LOOP ( 'NONE', ( #44032, #44875 ) ) ;
#6709 = PLANE ( 'NONE',  #2165 ) ;
#6710 = CARTESIAN_POINT ( 'NONE',  ( -339.1964088526558498, -116.8846903019842927, 58.63009191191280678 ) ) ;
#6711 = CARTESIAN_POINT ( 'NONE',  ( -47.97059563285963435, -193.5000000000000000, 0.8610436117673654355 ) ) ;
#6712 = DIRECTION ( 'NONE',  ( -0.2348860457809775482, 0.000000000000000000, -0.9720229140804121926 ) ) ;
#6713 = DIRECTION ( 'NONE',  ( -0.000000000000000000, 1.000000000000000000, 0.000000000000000000 ) ) ;
#6714 = DIRECTION ( 'NONE',  ( -0.000000000000000000, 1.000000000000000000, -0.000000000000000000 ) ) ;
#6715 = ORIENTED_EDGE ( 'NONE', *, *, #26481, .F. ) ;
#6716 = CARTESIAN_POINT ( 'NONE',  ( -339.1964088526558498, -79.00630452878414189, 38.74998146212082162 ) ) ;
#6717 = EDGE_CURVE ( 'NONE', #38969, #18701, #1429, .T. ) ;
#6718 = AXIS2_PLACEMENT_3D ( 'NONE', #16189, #3321, #7265 ) ;
#6719 = CIRCLE ( 'NONE', #4201, 125.0000000000000000 ) ;
#6720 = ORIENTED_EDGE ( 'NONE', *, *, #11512, .T. ) ;
#6721 = DIRECTION ( 'NONE',  ( 0.000000000000000000, -1.000000000000000000, 0.000000000000000000 ) ) ;
#6722 = DIRECTION ( 'NONE',  ( 0.000000000000000000, 0.000000000000000000, -1.000000000000000000 ) ) ;
#6723 = VERTEX_POINT ( 'NONE', #13518 ) ;
#6724 = DIRECTION ( 'NONE',  ( 0.000000000000000000, 0.6631226582407937498, -0.7485107481711024136 ) ) ;
#6725 = DIRECTION ( 'NONE',  ( 0.000000000000000000, 0.000000000000000000, -1.000000000000000000 ) ) ;
#6726 = FACE_OUTER_BOUND ( 'NONE', #5460, .T. ) ;
#6727 = CARTESIAN_POINT ( 'NONE',  ( -173.4291566779743050, -175.3837268820161057, 3.534122433558352760 ) ) ;
#6728 = CARTESIAN_POINT ( 'NONE',  ( 66.36634345758743336, -175.3837268820161057, 46.76022031560704306 ) ) ;
#6729 = EDGE_CURVE ( 'NONE', #38762, #28636, #34511, .T. ) ;
#6730 = ORIENTED_EDGE ( 'NONE', *, *, #18555, .F. ) ;
#6731 = CIRCLE ( 'NONE', #40271, 20.00000000000000355 ) ;
#6732 = CARTESIAN_POINT ( 'NONE',  ( -63.43218022845228887, -193.5000000000000000, 124.1024020384604540 ) ) ;
#6733 = ORIENTED_EDGE ( 'NONE', *, *, #30691, .F. ) ;
#6734 = EDGE_CURVE ( 'NONE', #5146, #10970, #33743, .T. ) ;
#6735 = ORIENTED_EDGE ( 'NONE', *, *, #24458, .T. ) ;
#6736 = EDGE_CURVE ( 'NONE', #47219, #3342, #6421, .T. ) ;
#6737 = FACE_OUTER_BOUND ( 'NONE', #12223, .T. ) ;
#6738 = EDGE_CURVE ( 'NONE', #13810, #44232, #15322, .T. ) ;
#6739 = VERTEX_POINT ( 'NONE', #23218 ) ;
#6740 = EDGE_CURVE ( 'NONE', #19788, #18322, #51334, .T. ) ;
#6741 = PRODUCT_DEFINITION_SHAPE ( 'NONE', 'NONE',  #52048 ) ;
#6742 = EDGE_LOOP ( 'NONE', ( #15258, #51435, #24365, #22684 ) ) ;
#6743 = DIRECTION ( 'NONE',  ( -0.2920567706369833760, 0.000000000000000000, 0.9564009842765202052 ) ) ;
#6744 = CARTESIAN_POINT ( 'NONE',  ( 51.70113075622899856, 35.00000000000000000, -45.78969942005421956 ) ) ;
#6745 = VERTEX_POINT ( 'NONE', #30839 ) ;
#6746 = DIRECTION ( 'NONE',  ( 1.000000000000000000, -0.000000000000000000, -0.000000000000000000 ) ) ;
#6747 = ADVANCED_FACE ( 'NONE', ( #19011 ), #22954, .F. ) ;
#6748 = LINE ( 'NONE', #51417, #15205 ) ;
#6749 = LINE ( 'NONE', #18819, #49221 ) ;
#6750 = ORIENTED_EDGE ( 'NONE', *, *, #50183, .F. ) ;
#6751 = VERTEX_POINT ( 'NONE', #43172 ) ;
#6752 = VECTOR ( 'NONE', #50579, 1000.000000000000000 ) ;
#6754 = ORIENTED_EDGE ( 'NONE', *, *, #8851, .F. ) ;
#6753 = VECTOR ( 'NONE', #34194, 1000.000000000000114 ) ;
#6755 = DIRECTION ( 'NONE',  ( 0.000000000000000000, 0.000000000000000000, 1.000000000000000000 ) ) ;
#6756 = CARTESIAN_POINT ( 'NONE',  ( -149.5539421794694022, -175.3837268820161057, 73.54509967498655953 ) ) ;
#6757 = EDGE_CURVE ( 'NONE', #38633, #43006, #175, .T. ) ;
#6758 = CARTESIAN_POINT ( 'NONE',  ( -32.98951909085346301, -175.3837268820161057, 123.0287672223653033 ) ) ;
#6759 = FACE_OUTER_BOUND ( 'NONE', #14610, .T. ) ;
#6760 = DIRECTION ( 'NONE',  ( 0.000000000000000000, -0.000000000000000000, 1.000000000000000000 ) ) ;
#6761 = ORIENTED_EDGE ( 'NONE', *, *, #34984, .F. ) ;
#6762 = EDGE_CURVE ( 'NONE', #31203, #27852, #12736, .T. ) ;
#6763 = EDGE_CURVE ( 'NONE', #27989, #1866, #37090, .T. ) ;
#6764 = DIRECTION ( 'NONE',  ( 0.000000000000000000, 0.000000000000000000, -1.000000000000000000 ) ) ;
#6765 = VERTEX_POINT ( 'NONE', #38962 ) ;
#6767 = ORIENTED_EDGE ( 'NONE', *, *, #17539, .F. ) ;
#6766 = FACE_OUTER_BOUND ( 'NONE', #23483, .T. ) ;
#6768 = EDGE_LOOP ( 'NONE', ( #20772, #31362, #3501, #24923, #20227, #14783, #10605, #5835 ) ) ;
#6769 = AXIS2_PLACEMENT_3D ( 'NONE', #26438, #18050, #21219 ) ;
#6770 = DIRECTION ( 'NONE',  ( 0.000000000000000000, 0.000000000000000000, -1.000000000000000000 ) ) ;
#6771 = CARTESIAN_POINT ( 'NONE',  ( -305.0000000000000568, -75.66382151296542702, -36.21739951675945690 ) ) ;
#6772 = DIRECTION ( 'NONE',  ( -1.000000000000000000, 5.928974370888993961E-15, 8.589602288500771593E-15 ) ) ;
#6773 = PLANE ( 'NONE',  #13350 ) ;
#6774 = ORIENTED_EDGE ( 'NONE', *, *, #44624, .T. ) ;
#6775 = FACE_OUTER_BOUND ( 'NONE', #19206, .T. ) ;
#6776 = VERTEX_POINT ( 'NONE', #31084 ) ;
#6777 = EDGE_CURVE ( 'NONE', #49846, #16432, #29552, .T. ) ;
#6778 = ORIENTED_EDGE ( 'NONE', *, *, #35273, .T. ) ;
#6779 = CARTESIAN_POINT ( 'NONE',  ( -336.3521761649654422, -75.87119766449505676, -34.85916744524372746 ) ) ;
#6780 = FACE_OUTER_BOUND ( 'NONE', #23026, .T. ) ;
#6781 = CARTESIAN_POINT ( 'NONE',  ( -163.6979789053106629, -193.5000000000000000, -45.83253885719559406 ) ) ;
#6782 = CARTESIAN_POINT ( 'NONE',  ( 58.48829670243887335, -177.1207230881787780, -64.67588669375807342 ) ) ;
#6783 = ORIENTED_EDGE ( 'NONE', *, *, #11482, .F. ) ;
#6784 = LINE ( 'NONE', #14939, #2229 ) ;
#6785 = CARTESIAN_POINT ( 'NONE',  ( -47.63353074800702558, -175.3837268820161057, -0.5338233779647817423 ) ) ;
#6786 = VECTOR ( 'NONE', #28473, 1000.000000000000000 ) ;
#6787 = DIRECTION ( 'NONE',  ( -0.000000000000000000, 1.000000000000000000, -0.000000000000000000 ) ) ;
#6788 = LINE ( 'NONE', #14416, #37129 ) ;
#6789 = ORIENTED_EDGE ( 'NONE', *, *, #8732, .F. ) ;
#6790 = PLANE ( 'NONE',  #17960 ) ;
#6791 = CYLINDRICAL_SURFACE ( 'NONE', #8896, 124.9999999999999858 ) ;
#6792 = CIRCLE ( 'NONE', #881, 2.000000000000001776 ) ;
#6793 = AXIS2_PLACEMENT_3D ( 'NONE', #35217, #39657, #28093 ) ;
#6794 = FACE_BOUND ( 'NONE', #36080, .T. ) ;
#6795 = ORIENTED_EDGE ( 'NONE', *, *, #19823, .F. ) ;
#6796 = DIRECTION ( 'NONE',  ( 0.000000000000000000, 0.000000000000000000, -1.000000000000000000 ) ) ;
#6797 = PLANE ( 'NONE',  #6816 ) ;
#6798 = ORIENTED_EDGE ( 'NONE', *, *, #47021, .F. ) ;
#6799 = EDGE_CURVE ( 'NONE', #32390, #16904, #11108, .T. ) ;
#6800 = EDGE_CURVE ( 'NONE', #6329, #13947, #47385, .T. ) ;
#6801 = CARTESIAN_POINT ( 'NONE',  ( -49.45768324380835423, -189.7472609257535510, 0.2059786187410958813 ) ) ;
#6802 = ORIENTED_EDGE ( 'NONE', *, *, #32429, .F. ) ;
#6803 = CARTESIAN_POINT ( 'NONE',  ( -118.9967449635792462, -189.7472609257535510, -103.2098131075562009 ) ) ;
#6804 = VECTOR ( 'NONE', #4604, 999.9999999999998863 ) ;
#6805 = CARTESIAN_POINT ( 'NONE',  ( 48.06131630543706734, -175.3837268820161057, -79.40367028273054473 ) ) ;
#6806 = DIRECTION ( 'NONE',  ( -0.000000000000000000, 1.000000000000000000, -0.000000000000000000 ) ) ;
#6807 = DIRECTION ( 'NONE',  ( 0.000000000000000000, 0.9709418174260519008, -0.2393156642875582940 ) ) ;
#6808 = VERTEX_POINT ( 'NONE', #10604 ) ;
#6809 = ORIENTED_EDGE ( 'NONE', *, *, #6112, .T. ) ;
#6810 = DIRECTION ( 'NONE',  ( -0.000000000000000000, 1.000000000000000000, -0.000000000000000000 ) ) ;
#6811 = EDGE_LOOP ( 'NONE', ( #10708, #40354, #10931, #11264 ) ) ;
#6812 = EDGE_CURVE ( 'NONE', #6055, #6703, #15855, .T. ) ;
#6813 = LINE ( 'NONE', #46501, #27582 ) ;
#6814 = VECTOR ( 'NONE', #24480, 1000.000000000000000 ) ;
#6815 = EDGE_CURVE ( 'NONE', #39243, #503, #42118, .T. ) ;
#6816 = AXIS2_PLACEMENT_3D ( 'NONE', #7814, #51461, #19643 ) ;
#6817 = FACE_OUTER_BOUND ( 'NONE', #10091, .T. ) ;
#6818 = CARTESIAN_POINT ( 'NONE',  ( -330.4913330509368166, -116.8846903019851311, -58.63009191191288494 ) ) ;
#6819 = VERTEX_POINT ( 'NONE', #27663 ) ;
#6822 = EDGE_LOOP ( 'NONE', ( #15394, #15739, #12800, #39374 ) ) ;
#6821 = DIRECTION ( 'NONE',  ( 0.05924062789371441901, 0.000000000000000000, -0.9982437317643214625 ) ) ;
#6820 = DIRECTION ( 'NONE',  ( 0.000000000000000000, 1.000000000000000000, 0.000000000000000000 ) ) ;
#6823 = LINE ( 'NONE', #47292, #28104 ) ;
#6824 = ORIENTED_EDGE ( 'NONE', *, *, #572, .T. ) ;
#6825 = CARTESIAN_POINT ( 'NONE',  ( -163.3872488209693756, -193.5000000000000000, -49.20491319441543254 ) ) ;
#6826 = ORIENTED_EDGE ( 'NONE', *, *, #32291, .T. ) ;
#6827 = LINE ( 'NONE', #38616, #40155 ) ;
#6828 = ORIENTED_EDGE ( 'NONE', *, *, #28558, .T. ) ;
#6831 = VERTEX_POINT ( 'NONE', #51097 ) ;
#6830 = LINE ( 'NONE', #18909, #11565 ) ;
#6829 = DIRECTION ( 'NONE',  ( 0.000000000000000000, 0.000000000000000000, 1.000000000000000000 ) ) ;
#6832 = ORIENTED_EDGE ( 'NONE', *, *, #24124, .T. ) ;
#6833 = CARTESIAN_POINT ( 'NONE',  ( -26.71218532227686637, -193.5000000000000000, 122.0745693923550732 ) ) ;
#6834 = VERTEX_POINT ( 'NONE', #15586 ) ;
#6835 = LINE ( 'NONE', #43086, #50524 ) ;
#6836 = PLANE ( 'NONE',  #51719 ) ;
#6837 = EDGE_LOOP ( 'NONE', ( #48083, #17771, #3605, #23755 ) ) ;
#6838 = CARTESIAN_POINT ( 'NONE',  ( -170.0000000000000284, -123.5000000000000284, 6.938893903907228378E-15 ) ) ;
#6839 = FACE_OUTER_BOUND ( 'NONE', #13987, .T. ) ;
#6840 = LINE ( 'NONE', #14999, #32471 ) ;
#6841 = DIRECTION ( 'NONE',  ( -0.000000000000000000, 1.000000000000000000, -0.000000000000000000 ) ) ;
#6842 = ORIENTED_EDGE ( 'NONE', *, *, #39398, .F. ) ;
#6843 =( LENGTH_UNIT ( ) NAMED_UNIT ( * ) SI_UNIT ( .MILLI., .METRE. ) );
#6844 = CARTESIAN_POINT ( 'NONE',  ( 32.99469856375238663, -175.3837268820161057, 94.79987230212020677 ) ) ;
#6845 = PLANE ( 'NONE',  #23967 ) ;
#6846 = DIRECTION ( 'NONE',  ( 0.000000000000000000, -0.000000000000000000, 1.000000000000000000 ) ) ;
#6847 = ORIENTED_EDGE ( 'NONE', *, *, #5162, .T. ) ;
#6848 = CARTESIAN_POINT ( 'NONE',  ( 73.80528149577283159, -189.7472609257535510, 25.91377046305970211 ) ) ;
#6849 = CARTESIAN_POINT ( 'NONE',  ( 38.71172987070726634, -175.3837268820161057, -89.56983042009264295 ) ) ;
#6850 = VECTOR ( 'NONE', #1213, 1000.000000000000000 ) ;
#6851 = CARTESIAN_POINT ( 'NONE',  ( -48.47912675150885065, -120.5000000000000284, 6.938893903907228378E-15 ) ) ;
#6852 = LINE ( 'NONE', #43375, #21069 ) ;
#6853 = DIRECTION ( 'NONE',  ( 0.000000000000000000, 0.000000000000000000, 1.000000000000000000 ) ) ;
#6854 = EDGE_CURVE ( 'NONE', #51787, #22734, #42666, .T. ) ;
#6855 = VERTEX_POINT ( 'NONE', #43695 ) ;
#6856 = VECTOR ( 'NONE', #9366, 1000.000000000000000 ) ;
#6857 = VECTOR ( 'NONE', #4529, 1000.000000000000000 ) ;
#6858 = DIRECTION ( 'NONE',  ( -0.9929810960135185827, 0.000000000000000000, 0.1182731709213523247 ) ) ;
#6859 = CARTESIAN_POINT ( 'NONE',  ( 14.37129481273059106, -175.3837268820161057, -108.0501018472328241 ) ) ;
#6860 = DIRECTION ( 'NONE',  ( -0.000000000000000000, 1.000000000000000000, 0.000000000000000000 ) ) ;
#6861 = CARTESIAN_POINT ( 'NONE',  ( -336.3521761649654422, -172.9832938399466684, -32.17247266903247294 ) ) ;
#6862 = CARTESIAN_POINT ( 'NONE',  ( -48.47912675150885065, -189.7472609257535510, 6.938893903907228378E-15 ) ) ;
#6863 = ORIENTED_EDGE ( 'NONE', *, *, #51034, .T. ) ;
#6864 = CARTESIAN_POINT ( 'NONE',  ( -339.1964088526558498, -163.6602333390095509, 44.57752413668022484 ) ) ;
#6865 = AXIS2_PLACEMENT_3D ( 'NONE', #35287, #31340, #10864 ) ;
#6866 = DIRECTION ( 'NONE',  ( 0.000000000000000000, 0.000000000000000000, 1.000000000000000000 ) ) ;
#6867 = ORIENTED_EDGE ( 'NONE', *, *, #40944, .F. ) ;
#6868 = ORIENTED_EDGE ( 'NONE', *, *, #40757, .F. ) ;
#6869 = VECTOR ( 'NONE', #42483, 1000.000000000000000 ) ;
#6870 = ORIENTED_EDGE ( 'NONE', *, *, #1748, .T. ) ;
#6871 = ADVANCED_FACE ( 'NONE', ( #7694 ), #50817, .T. ) ;
#6872 = CARTESIAN_POINT ( 'NONE',  ( -330.4913330509368166, -74.65991953890832633, 33.10432812419081472 ) ) ;
#6873 = CARTESIAN_POINT ( 'NONE',  ( -48.47912675150885065, -188.5000000000000284, 6.938893903907228378E-15 ) ) ;
#6874 = FACE_OUTER_BOUND ( 'NONE', #51382, .T. ) ;
#6875 = VERTEX_POINT ( 'NONE', #51860 ) ;
#6876 = DIRECTION ( 'NONE',  ( 1.000000000000000000, -0.000000000000000000, -0.000000000000000000 ) ) ;
#6877 = DIRECTION ( 'NONE',  ( 0.000000000000000000, 0.9709418174260519008, -0.2393156642875582940 ) ) ;
#6880 = ORIENTED_EDGE ( 'NONE', *, *, #37885, .T. ) ;
#6879 = DIRECTION ( 'NONE',  ( 0.000000000000000000, 0.000000000000000000, -1.000000000000000000 ) ) ;
#6878 = CARTESIAN_POINT ( 'NONE',  ( -48.47912675150885065, -175.3837268820161057, 6.938893903907228378E-15 ) ) ;
#6881 = DIRECTION ( 'NONE',  ( 0.000000000000000000, 0.000000000000000000, -1.000000000000000000 ) ) ;
#6882 = VERTEX_POINT ( 'NONE', #26878 ) ;
#6883 = CARTESIAN_POINT ( 'NONE',  ( -332.3517673607765914, -73.44864141332200802, 31.34948880313848107 ) ) ;
#6884 = CIRCLE ( 'NONE', #13595, 4.000000000000003553 ) ;
#6885 = ORIENTED_EDGE ( 'NONE', *, *, #41680, .F. ) ;
#6886 = DIRECTION ( 'NONE',  ( 0.000000000000000000, -0.000000000000000000, 1.000000000000000000 ) ) ;
#6887 = LINE ( 'NONE', #14525, #19611 ) ;
#6888 = CIRCLE ( 'NONE', #15293, 60.00000000000000000 ) ;
#6889 = LINE ( 'NONE', #51059, #15687 ) ;
#6890 = ORIENTED_EDGE ( 'NONE', *, *, #25671, .F. ) ;
#6891 = CIRCLE ( 'NONE', #28697, 124.9999999999999858 ) ;
#6892 = VERTEX_POINT ( 'NONE', #31866 ) ;
#6893 = CARTESIAN_POINT ( 'NONE',  ( -330.4913330509368166, -137.1341532842531876, -57.40522506028080585 ) ) ;
#6894 = DIRECTION ( 'NONE',  ( 0.000000000000000000, -0.000000000000000000, 1.000000000000000000 ) ) ;
#6895 = ORIENTED_EDGE ( 'NONE', *, *, #10528, .T. ) ;
#6896 = LINE ( 'NONE', #42889, #19047 ) ;
#6897 = DIRECTION ( 'NONE',  ( -0.000000000000000000, 1.000000000000000000, -0.000000000000000000 ) ) ;
#6898 = ADVANCED_FACE ( 'NONE', ( #22695 ), #14824, .F. ) ;
#6899 = ORIENTED_EDGE ( 'NONE', *, *, #40521, .T. ) ;
#6900 = FACE_BOUND ( 'NONE', #14466, .T. ) ;
#6901 = VECTOR ( 'NONE', #2201, 1000.000000000000000 ) ;
#6902 = CARTESIAN_POINT ( 'NONE',  ( -40.24578378811990831, -189.7472609257535510, 124.7285535218268251 ) ) ;
#6903 = ADVANCED_FACE ( 'NONE', ( #15086 ), #45006, .F. ) ;
#6904 = ORIENTED_EDGE ( 'NONE', *, *, #22236, .T. ) ;
#6905 = CARTESIAN_POINT ( 'NONE',  ( 55.91309001144629320, -193.5000000000000000, 68.75510947788671956 ) ) ;
#6906 = ORIENTED_EDGE ( 'NONE', *, *, #27962, .T. ) ;
#6907 = AXIS2_PLACEMENT_3D ( 'NONE', #45284, #27988, #44023 ) ;
#6908 = CIRCLE ( 'NONE', #31238, 60.00000000000000000 ) ;
#6909 = DIRECTION ( 'NONE',  ( 0.000000000000000000, 0.000000000000000000, 1.000000000000000000 ) ) ;
#6910 = DIRECTION ( 'NONE',  ( 0.000000000000000000, -0.1205366802553130001, 0.9927088740980551940 ) ) ;
#6911 = ORIENTED_EDGE ( 'NONE', *, *, #42681, .T. ) ;
#6912 = CARTESIAN_POINT ( 'NONE',  ( -47.48307690889363641, -189.7472609257535510, 0.08879589532294547560 ) ) ;
#6913 = CARTESIAN_POINT ( 'NONE',  ( -170.0000000000000284, -155.0173647354142759, 14.76740078976490622 ) ) ;
#6914 = CARTESIAN_POINT ( 'NONE',  ( -7.515176836080581957, -177.1207230881787780, 117.0391155081705250 ) ) ;
#6915 = ADVANCED_FACE ( 'NONE', ( #23970 ), #25034, .F. ) ;
#6916 = EDGE_CURVE ( 'NONE', #18084, #12833, #32118, .T. ) ;
#6917 = ORIENTED_EDGE ( 'NONE', *, *, #47378, .T. ) ;
#6918 = LINE ( 'NONE', #38958, #51477 ) ;
#6919 = EDGE_CURVE ( 'NONE', #20987, #12980, #44735, .T. ) ;
#6920 = DIRECTION ( 'NONE',  ( -1.000000000000000000, 0.000000000000000000, -0.000000000000000000 ) ) ;
#6921 = LINE ( 'NONE', #46112, #51216 ) ;
#6923 = ORIENTED_EDGE ( 'NONE', *, *, #28724, .T. ) ;
#6922 = CARTESIAN_POINT ( 'NONE',  ( -336.3521761649654422, -180.1556192733800117, 16.67542351306693149 ) ) ;
#6924 = VECTOR ( 'NONE', #26991, 1000.000000000000114 ) ;
#6925 = EDGE_LOOP ( 'NONE', ( #39685, #30103, #23179, #46150 ) ) ;
#6926 = CARTESIAN_POINT ( 'NONE',  ( 50.08808042611237710, -177.1207230881787780, -76.87330921200083367 ) ) ;
#6927 = VECTOR ( 'NONE', #31280, 1000.000000000000227 ) ;
#6928 = LINE ( 'NONE', #51339, #49784 ) ;
#6929 = ORIENTED_EDGE ( 'NONE', *, *, #48371, .T. ) ;
#6930 = ORIENTED_EDGE ( 'NONE', *, *, #17989, .F. ) ;
#6931 = CARTESIAN_POINT ( 'NONE',  ( -168.3100285466275636, -193.5000000000000000, -31.88354567334998535 ) ) ;
#6932 = ORIENTED_EDGE ( 'NONE', *, *, #46192, .F. ) ;
#6933 = CARTESIAN_POINT ( 'NONE',  ( -238.7407812814481076, -213.5000000000000000, 10.00000000000000178 ) ) ;
#6934 = CARTESIAN_POINT ( 'NONE',  ( -151.1459075827612537, -177.1207230881787780, 69.53890913632950799 ) ) ;
#6935 = CARTESIAN_POINT ( 'NONE',  ( -84.82349129030166068, -175.3837268820161057, -119.5996955107802222 ) ) ;
#6936 = LINE ( 'NONE', #3498, #8135 ) ;
#6937 = EDGE_LOOP ( 'NONE', ( #25542, #14929, #6867, #28848 ) ) ;
#6938 = VECTOR ( 'NONE', #5261, 999.9999999999998863 ) ;
#6939 = VERTEX_POINT ( 'NONE', #48163 ) ;
#6940 = VECTOR ( 'NONE', #35846, 1000.000000000000000 ) ;
#6941 = ORIENTED_EDGE ( 'NONE', *, *, #42407, .T. ) ;
#6942 = CARTESIAN_POINT ( 'NONE',  ( -339.1964088526558498, -123.5000000000000284, 0.000000000000000000 ) ) ;
#6943 = CARTESIAN_POINT ( 'NONE',  ( -139.0630283577175987, -177.1207230881787780, -86.13684908212449898 ) ) ;
#6944 = VECTOR ( 'NONE', #41995, 1000.000000000000114 ) ;
#6945 = CARTESIAN_POINT ( 'NONE',  ( -330.4913330509368166, -162.2499814621210419, 44.49369547121568758 ) ) ;
#6946 = VECTOR ( 'NONE', #46880, 1000.000000000000000 ) ;
#6947 = DIRECTION ( 'NONE',  ( -0.8757349421956310831, 0.000000000000000000, -0.4827922027307550712 ) ) ;
#6948 = DIRECTION ( 'NONE',  ( -0.6965510290629932655, 0.000000000000000000, -0.7175072570443347120 ) ) ;
#6949 = ORIENTED_EDGE ( 'NONE', *, *, #5625, .F. ) ;
#6950 = VECTOR ( 'NONE', #43305, 999.9999999999998863 ) ;
#6951 = CARTESIAN_POINT ( 'NONE',  ( -169.2746641285359317, -193.5000000000000000, -32.14713283941905786 ) ) ;
#6952 = DIRECTION ( 'NONE',  ( -0.000000000000000000, 1.000000000000000000, -0.000000000000000000 ) ) ;
#6953 = EDGE_LOOP ( 'NONE', ( #23975, #31834, #26432, #41371 ) ) ;
#6954 = EDGE_LOOP ( 'NONE', ( #30383, #29281, #15917, #28967 ) ) ;
#6955 = DIRECTION ( 'NONE',  ( -0.5586467658036594619, 0.000000000000000000, 0.8294056854501971054 ) ) ;
#6956 = CARTESIAN_POINT ( 'NONE',  ( 26.52087324849106054, -173.5000000000000284, -60.00000000000003553 ) ) ;
#6957 = CARTESIAN_POINT ( 'NONE',  ( 11.16082883019764793, 28.00000000000000355, 7.004579506989120574 ) ) ;
#6958 = CARTESIAN_POINT ( 'NONE',  ( -336.3521761649654422, -181.8730728925770563, 8.732051761644092025 ) ) ;
#6959 = CIRCLE ( 'NONE', #35485, 125.0000000000000000 ) ;
#6960 = DIRECTION ( 'NONE',  ( 0.8757349421956379665, 0.000000000000000000, -0.4827922027307427477 ) ) ;
#6961 = EDGE_CURVE ( 'NONE', #24932, #34133, #40510, .T. ) ;
#6962 = ADVANCED_FACE ( 'NONE', ( #40773 ), #27913, .T. ) ;
#6963 = CARTESIAN_POINT ( 'NONE',  ( 20.93410174202488605, -175.3837268820161057, -102.7511748916624583 ) ) ;
#6964 = ORIENTED_EDGE ( 'NONE', *, *, #50308, .T. ) ;
#6965 = CARTESIAN_POINT ( 'NONE',  ( -305.0000000000000568, -108.6560878169904640, -58.13482838284724608 ) ) ;
#6966 = VECTOR ( 'NONE', #37429, 999.9999999999998863 ) ;
#6967 = ORIENTED_EDGE ( 'NONE', *, *, #17013, .F. ) ;
#6968 = DIRECTION ( 'NONE',  ( 0.000000000000000000, 1.000000000000000000, -0.000000000000000000 ) ) ;
#6969 = DIRECTION ( 'NONE',  ( -1.000000000000000000, -0.000000000000000000, -0.000000000000000000 ) ) ;
#6970 = ORIENTED_EDGE ( 'NONE', *, *, #14480, .T. ) ;
#6971 = EDGE_CURVE ( 'NONE', #471, #34929, #8722, .T. ) ;
#6972 = DIRECTION ( 'NONE',  ( 0.000000000000000000, 0.000000000000000000, -1.000000000000000000 ) ) ;
#6973 = CARTESIAN_POINT ( 'NONE',  ( -180.0000000000000568, -123.5000000000000284, 6.938893903907228378E-15 ) ) ;
#6974 = CARTESIAN_POINT ( 'NONE',  ( -49.25565061422690150, -183.6283474603465606, 0.6300878435817109935 ) ) ;
#6975 = EDGE_CURVE ( 'NONE', #42318, #21717, #48423, .T. ) ;
#6976 = AXIS2_PLACEMENT_3D ( 'NONE', #9760, #50237, #6335 ) ;
#6977 = CARTESIAN_POINT ( 'NONE',  ( -339.1964088526558498, -66.09477493971894546, 13.63415328425207917 ) ) ;
#6978 = VECTOR ( 'NONE', #8856, 1000.000000000000000 ) ;
#6979 = EDGE_CURVE ( 'NONE', #49449, #46206, #28427, .T. ) ;
#6980 = LINE ( 'NONE', #2519, #50493 ) ;
#6981 = EDGE_LOOP ( 'NONE', ( #31500, #43473, #28838, #9855 ) ) ;
#6982 = VECTOR ( 'NONE', #17669, 1000.000000000000000 ) ;
#6983 = EDGE_CURVE ( 'NONE', #28151, #33835, #36580, .T. ) ;
#6984 = DIRECTION ( 'NONE',  ( -0.000000000000000000, 1.000000000000000000, -0.000000000000000000 ) ) ;
#6986 = ORIENTED_EDGE ( 'NONE', *, *, #6209, .T. ) ;
#6985 = LINE ( 'NONE', #19336, #46415 ) ;
#6987 = EDGE_CURVE ( 'NONE', #6563, #602, #32372, .T. ) ;
#6988 = ORIENTED_EDGE ( 'NONE', *, *, #5037, .F. ) ;
#6989 = DIRECTION ( 'NONE',  ( 0.9266896074318370369, 0.000000000000000000, -0.3758275821142292306 ) ) ;
#6990 = VECTOR ( 'NONE', #15144, 1000.000000000000000 ) ;
#6991 = VERTEX_POINT ( 'NONE', #316 ) ;
#6992 = CARTESIAN_POINT ( 'NONE',  ( -164.3791542526839180, -193.5000000000000000, 46.82076062204521349 ) ) ;
#6993 = VERTEX_POINT ( 'NONE', #11881 ) ;
#6994 = DIRECTION ( 'NONE',  ( 0.000000000000000000, 0.000000000000000000, 1.000000000000000000 ) ) ;
#6995 = CARTESIAN_POINT ( 'NONE',  ( 62.13187335169531167, -183.6283474603465606, -58.22548115875872554 ) ) ;
#6996 = ORIENTED_EDGE ( 'NONE', *, *, #47394, .T. ) ;
#6997 = CARTESIAN_POINT ( 'NONE',  ( -105.4063847101409692, -175.3837268820161057, -111.2847127925096231 ) ) ;
#6998 = AXIS2_PLACEMENT_3D ( 'NONE', #8254, #30244, #14734 ) ;
#6999 = DIRECTION ( 'NONE',  ( -0.000000000000000000, 1.000000000000000000, -0.000000000000000000 ) ) ;
#7000 = DIRECTION ( 'NONE',  ( -0.000000000000000000, 0.2393156642875547968, -0.9709418174260527890 ) ) ;
#7001 = ORIENTED_EDGE ( 'NONE', *, *, #46337, .F. ) ;
#7002 = ORIENTED_EDGE ( 'NONE', *, *, #38834, .F. ) ;
#7003 = CIRCLE ( 'NONE', #11194, 124.9999999999999858 ) ;
#7004 = EDGE_LOOP ( 'NONE', ( #31399, #9392, #35994, #17993 ) ) ;
#7005 = DIRECTION ( 'NONE',  ( 0.000000000000000000, 0.000000000000000000, 1.000000000000000000 ) ) ;
#7006 = EDGE_CURVE ( 'NONE', #40482, #41226, #48942, .T. ) ;
#7007 = LINE ( 'NONE', #26444, #47008 ) ;
#7008 = PLANE ( 'NONE',  #21780 ) ;
#7009 = LINE ( 'NONE', #10691, #40460 ) ;
#7010 = DIRECTION ( 'NONE',  ( -0.000000000000000000, 1.000000000000000000, -0.000000000000000000 ) ) ;
#7011 = ORIENTED_EDGE ( 'NONE', *, *, #16934, .T. ) ;
#7012 = AXIS2_PLACEMENT_3D ( 'NONE', #35000, #41859, #26850 ) ;
#7013 = DIRECTION ( 'NONE',  ( -0.000000000000000000, 0.5680647467311656929, 0.8229838658936495799 ) ) ;
#7014 = ADVANCED_FACE ( 'NONE', ( #20824 ), #43947, .F. ) ;
#7015 = ORIENTED_EDGE ( 'NONE', *, *, #2157, .F. ) ;
#7017 = EDGE_LOOP ( 'NONE', ( #40676, #47491, #15886, #28575 ) ) ;
#7016 = LINE ( 'NONE', #23040, #6340 ) ;
#7018 = VERTEX_POINT ( 'NONE', #24247 ) ;
#7019 = CARTESIAN_POINT ( 'NONE',  ( 63.54086012517504400, -175.3837268820161057, -53.17445600718542664 ) ) ;
#7020 = DIRECTION ( 'NONE',  ( 1.000000000000000000, 0.000000000000000000, -0.000000000000000000 ) ) ;
#7021 = EDGE_CURVE ( 'NONE', #31777, #5941, #21156, .T. ) ;
#7022 = ADVANCED_FACE ( 'NONE', ( #16633 ), #28683, .T. ) ;
#7023 = CARTESIAN_POINT ( 'NONE',  ( -81.14588623932559130, -177.1207230881787780, 120.6560517527618117 ) ) ;
#7024 = EDGE_CURVE ( 'NONE', #26963, #19552, #7937, .T. ) ;
#7025 = EDGE_CURVE ( 'NONE', #7418, #32022, #49672, .T. ) ;
#7026 = CARTESIAN_POINT ( 'NONE',  ( -171.5592422664403216, -183.6283474603465606, -21.82395850507258928 ) ) ;
#7027 = ORIENTED_EDGE ( 'NONE', *, *, #23771, .T. ) ;
#7028 = DIRECTION ( 'NONE',  ( -8.718379230999707126E-17, 0.4647231720437631775, -0.8854560256532126861 ) ) ;
#7029 = ORIENTED_EDGE ( 'NONE', *, *, #31081, .T. ) ;
#7030 = EDGE_CURVE ( 'NONE', #8616, #13126, #5582, .T. ) ;
#7031 = EDGE_LOOP ( 'NONE', ( #17174, #29421, #33522, #780 ) ) ;
#7032 = CARTESIAN_POINT ( 'NONE',  ( -330.4913330509368166, -178.4886558749184076, -21.38919645685194837 ) ) ;
#7033 = CARTESIAN_POINT ( 'NONE',  ( -153.4237445717492392, -189.7472609257535510, 66.05018866041348247 ) ) ;
#7034 = ADVANCED_FACE ( 'NONE', ( #9511 ), #37360, .F. ) ;
#7035 = LINE ( 'NONE', #42241, #19660 ) ;
#7036 = DIRECTION ( 'NONE',  ( -0.000000000000000000, 1.000000000000000000, -0.000000000000000000 ) ) ;
#7037 = ORIENTED_EDGE ( 'NONE', *, *, #10062, .F. ) ;
#7038 = DIRECTION ( 'NONE',  ( 0.05924062789370748011, 0.000000000000000000, 0.9982437317643217956 ) ) ;
#7039 = VECTOR ( 'NONE', #43295, 1000.000000000000000 ) ;
#7040 = CARTESIAN_POINT ( 'NONE',  ( -130.7087404384255080, -189.7472609257535510, -94.14505102712755047 ) ) ;
#7041 = CARTESIAN_POINT ( 'NONE',  ( -159.8192355313504152, -183.6283474603465606, -56.81883646197837834 ) ) ;
#7042 = DIRECTION ( 'NONE',  ( 0.000000000000000000, -1.000000000000000000, 0.000000000000000000 ) ) ;
#7043 = ADVANCED_FACE ( 'NONE', ( #50249 ), #29221, .T. ) ;
#7044 = ORIENTED_EDGE ( 'NONE', *, *, #9704, .F. ) ;
#7045 = DIRECTION ( 'NONE',  ( 0.000000000000000000, 0.000000000000000000, -1.000000000000000000 ) ) ;
#7046 = DIRECTION ( 'NONE',  ( -0.4300652022765183435, 0.000000000000000000, -0.9027978299657446470 ) ) ;
#7047 = AXIS2_PLACEMENT_3D ( 'NONE', #14604, #11160, #10391 ) ;
#7048 = EDGE_CURVE ( 'NONE', #19062, #16981, #41295, .T. ) ;
#7049 = DIRECTION ( 'NONE',  ( 0.000000000000000000, -1.000000000000000000, 0.000000000000000000 ) ) ;
#7050 = EDGE_LOOP ( 'NONE', ( #22447, #33533, #14657, #2476 ) ) ;
#7051 = EDGE_CURVE ( 'NONE', #13015, #23682, #33157, .T. ) ;
#7052 = LINE ( 'NONE', #43300, #32304 ) ;
#7053 = FACE_OUTER_BOUND ( 'NONE', #9680, .T. ) ;
#7054 = EDGE_CURVE ( 'NONE', #50634, #10587, #4348, .T. ) ;
#7055 = ORIENTED_EDGE ( 'NONE', *, *, #27386, .F. ) ;
#7056 = LINE ( 'NONE', #34393, #45567 ) ;
#7057 = VECTOR ( 'NONE', #22253, 1000.000000000000227 ) ;
#7058 = VERTEX_POINT ( 'NONE', #21864 ) ;
#7059 = ADVANCED_FACE ( 'NONE', ( #6099 ), #5321, .T. ) ;
#7060 = CARTESIAN_POINT ( 'NONE',  ( -336.3521761649654422, -98.41210887299327226, -53.46519113769058151 ) ) ;
#7061 = FACE_BOUND ( 'NONE', #31927, .T. ) ;
#7062 = CARTESIAN_POINT ( 'NONE',  ( -51.89154260666836649, -177.1207230881787780, 124.9534129907280828 ) ) ;
#7063 = CARTESIAN_POINT ( 'NONE',  ( -330.0000000000000568, -123.5000000000000284, -60.00000000000000000 ) ) ;
#7064 = EDGE_CURVE ( 'NONE', #42669, #42461, #49204, .T. ) ;
#7065 = EDGE_LOOP ( 'NONE', ( #18910, #14599, #39610, #48035 ) ) ;
#7066 = EDGE_CURVE ( 'NONE', #51627, #1228, #9259, .T. ) ;
#7067 = ORIENTED_EDGE ( 'NONE', *, *, #12673, .F. ) ;
#7068 = CARTESIAN_POINT ( 'NONE',  ( 46.00000000000000711, 0.000000000000000000, -46.00000000000000000 ) ) ;
#7069 = ORIENTED_EDGE ( 'NONE', *, *, #43461, .F. ) ;
#7070 = CYLINDRICAL_SURFACE ( 'NONE', #19226, 125.0000000000000000 ) ;
#7071 = CIRCLE ( 'NONE', #49877, 125.0000000000000000 ) ;
#7072 = AXIS2_PLACEMENT_3D ( 'NONE', #28078, #3401, #15501 ) ;
#7073 = FACE_OUTER_BOUND ( 'NONE', #40219, .T. ) ;
#7074 = DIRECTION ( 'NONE',  ( -1.000000000000000000, 0.000000000000000000, 0.000000000000000000 ) ) ;
#7075 = ORIENTED_EDGE ( 'NONE', *, *, #44591, .T. ) ;
#7078 = ORIENTED_EDGE ( 'NONE', *, *, #37052, .F. ) ;
#7077 = DIRECTION ( 'NONE',  ( -8.718379230999705894E-17, 0.3546048870425300148, -0.9350162426854169428 ) ) ;
#7076 = CARTESIAN_POINT ( 'NONE',  ( -4.008990953134272672, 52.52292218020331660, -19.70988118881478712 ) ) ;
#7079 = LINE ( 'NONE', #3134, #5526 ) ;
#7080 = EDGE_LOOP ( 'NONE', ( #15158, #22484, #18835, #21624 ) ) ;
#7081 = LINE ( 'NONE', #18654, #21358 ) ;
#7082 = EDGE_LOOP ( 'NONE', ( #27727, #23227, #43906, #33346, #11271, #33177 ) ) ;
#7083 = ADVANCED_FACE ( 'NONE', ( #33438 ), #33682, .T. ) ;
#7084 = EDGE_CURVE ( 'NONE', #76, #47574, #25532, .T. ) ;
#7085 = FACE_OUTER_BOUND ( 'NONE', #31288, .T. ) ;
#7086 = VERTEX_POINT ( 'NONE', #37631 ) ;
#7088 = CARTESIAN_POINT ( 'NONE',  ( -305.0000000000000568, -176.3931552210900691, 28.32515014536862807 ) ) ;
#7087 = CARTESIAN_POINT ( 'NONE',  ( -149.9407190013152160, -193.5000000000000000, -73.01058346660458653 ) ) ;
#7089 = CIRCLE ( 'NONE', #29733, 125.0000000000000000 ) ;
#7090 = ORIENTED_EDGE ( 'NONE', *, *, #35313, .F. ) ;
#7091 = EDGE_CURVE ( 'NONE', #43619, #46084, #1633, .T. ) ;
#7092 = ADVANCED_FACE ( 'NONE', ( #13710 ), #22372, .T. ) ;
#7093 = CARTESIAN_POINT ( 'NONE',  ( 3.686287386450715076E-15, 20.00000000000000000, -46.00000000000000711 ) ) ;
#7094 = ORIENTED_EDGE ( 'NONE', *, *, #32043, .T. ) ;
#7095 = DIRECTION ( 'NONE',  ( 0.000000000000000000, -1.000000000000000000, 0.000000000000000000 ) ) ;
#7096 = DIRECTION ( 'NONE',  ( 0.000000000000000000, -0.3546048870425426158, -0.9350162426854120579 ) ) ;
#7097 = ORIENTED_EDGE ( 'NONE', *, *, #7453, .F. ) ;
#7098 = CYLINDRICAL_SURFACE ( 'NONE', #15478, 125.0000000000000000 ) ;
#7099 = DIRECTION ( 'NONE',  ( 0.000000000000000000, -0.8854560256532126861, -0.4647231720437631775 ) ) ;
#7100 = LINE ( 'NONE', #42833, #13158 ) ;
#7101 = CARTESIAN_POINT ( 'NONE',  ( -339.1964088526558498, -138.1050951016792681, -57.16590939599323917 ) ) ;
#7102 = ORIENTED_EDGE ( 'NONE', *, *, #45720, .T. ) ;
#7103 = CARTESIAN_POINT ( 'NONE',  ( -336.3521761649654422, -161.2787550547969033, 46.61293454085098631 ) ) ;
#7104 = DIRECTION ( 'NONE',  ( 0.000000000000000000, -0.4647231720437573488, 0.8854560256532157947 ) ) ;
#7105 = LINE ( 'NONE', #38637, #12858 ) ;
#7106 = ORIENTED_EDGE ( 'NONE', *, *, #8083, .F. ) ;
#7107 = CARTESIAN_POINT ( 'NONE',  ( -332.3517673607765914, -176.9651911376907094, -25.08789112700655721 ) ) ;
#7108 = LINE ( 'NONE', #22629, #19379 ) ;
#7109 = AXIS2_PLACEMENT_3D ( 'NONE', #36030, #29, #44177 ) ;
#7110 = CARTESIAN_POINT ( 'NONE',  ( -260.0000000000000000, -113.5000000000000000, 60.00000000000000711 ) ) ;
#7111 = VECTOR ( 'NONE', #5767, 1000.000000000000000 ) ;
#7112 = DIRECTION ( 'NONE',  ( -0.000000000000000000, 1.000000000000000000, -0.000000000000000000 ) ) ;
#7113 = LINE ( 'NONE', #14746, #26604 ) ;
#7114 = ORIENTED_EDGE ( 'NONE', *, *, #50340, .F. ) ;
#7115 = CIRCLE ( 'NONE', #36460, 125.0000000000000000 ) ;
#7116 = ADVANCED_FACE ( 'NONE', ( #5850 ), #37882, .T. ) ;
#7117 = PLANE ( 'NONE',  #32963 ) ;
#7118 = CARTESIAN_POINT ( 'NONE',  ( -148.0127667507368585, -177.1207230881787780, -75.61781872352626976 ) ) ;
#7119 = CARTESIAN_POINT ( 'NONE',  ( -332.3517673607765914, -87.81784868886214213, 47.06073758877343494 ) ) ;
#7120 = PLANE ( 'NONE',  #43869 ) ;
#7121 = DIRECTION ( 'NONE',  ( 0.000000000000000000, 1.000000000000000000, 0.000000000000000000 ) ) ;
#7122 = ORIENTED_EDGE ( 'NONE', *, *, #13614, .T. ) ;
#7123 = CIRCLE ( 'NONE', #49113, 124.9999999999999858 ) ;
#7124 = DIRECTION ( 'NONE',  ( -1.000000000000000000, -0.000000000000000000, -0.000000000000000000 ) ) ;
#7125 = VERTEX_POINT ( 'NONE', #46052 ) ;
#7126 = EDGE_LOOP ( 'NONE', ( #30101, #33075, #43603, #25151 ) ) ;
#7127 = ORIENTED_EDGE ( 'NONE', *, *, #23402, .T. ) ;
#7128 = CARTESIAN_POINT ( 'NONE',  ( 0.000000000000000000, -64.93017642821482127, -7.111664135064078351 ) ) ;
#7129 = DIRECTION ( 'NONE',  ( 0.000000000000000000, 0.000000000000000000, 1.000000000000000000 ) ) ;
#7130 = ORIENTED_EDGE ( 'NONE', *, *, #42614, .T. ) ;
#7131 = DIRECTION ( 'NONE',  ( 1.000000000000000000, 0.000000000000000000, 0.000000000000000000 ) ) ;
#7132 = CARTESIAN_POINT ( 'NONE',  ( -332.3517673607765914, -106.8245764869328980, 56.65561927337994064 ) ) ;
#7135 = VERTEX_POINT ( 'NONE', #10040 ) ;
#7134 = CARTESIAN_POINT ( 'NONE',  ( 39.56636334395316368, -193.5000000000000000, -87.31661597576083977 ) ) ;
#7133 = LINE ( 'NONE', #2669, #50176 ) ;
#7136 = CIRCLE ( 'NONE', #33993, 125.0000000000000000 ) ;
#7137 = PLANE ( 'NONE',  #38209 ) ;
#7138 = CIRCLE ( 'NONE', #17240, 125.0000000000000000 ) ;
#7139 = ORIENTED_EDGE ( 'NONE', *, *, #9639, .F. ) ;
#7140 = LINE ( 'NONE', #34997, #51560 ) ;
#7141 = ORIENTED_EDGE ( 'NONE', *, *, #41980, .F. ) ;
#7142 = VECTOR ( 'NONE', #38178, 1000.000000000000000 ) ;
#7143 = EDGE_CURVE ( 'NONE', #4089, #44109, #26052, .T. ) ;
#7144 = FACE_OUTER_BOUND ( 'NONE', #5155, .T. ) ;
#7145 = LINE ( 'NONE', #19241, #45631 ) ;
#7146 = LINE ( 'NONE', #47355, #3018 ) ;
#7147 = ORIENTED_EDGE ( 'NONE', *, *, #1996, .F. ) ;
#7148 = FACE_OUTER_BOUND ( 'NONE', #15957, .T. ) ;
#7149 = ORIENTED_EDGE ( 'NONE', *, *, #48869, .T. ) ;
#7150 = DIRECTION ( 'NONE',  ( 0.000000000000000000, -0.000000000000000000, -1.000000000000000000 ) ) ;
#7151 = LINE ( 'NONE', #39210, #1553 ) ;
#7152 = ORIENTED_EDGE ( 'NONE', *, *, #46733, .F. ) ;
#7153 = VECTOR ( 'NONE', #23108, 1000.000000000000000 ) ;
#7154 = PLANE ( 'NONE',  #37492 ) ;
#7155 = CIRCLE ( 'NONE', #43234, 125.0000000000000000 ) ;
#7156 = CARTESIAN_POINT ( 'NONE',  ( -339.1964088526558498, -180.9052250602807703, 13.63415328425337236 ) ) ;
#7157 = ORIENTED_EDGE ( 'NONE', *, *, #50884, .F. ) ;
#7158 = FACE_BOUND ( 'NONE', #45802, .T. ) ;
#7159 = CIRCLE ( 'NONE', #5491, 125.0000000000000000 ) ;
#7160 = DIRECTION ( 'NONE',  ( -0.000000000000000000, 1.000000000000000000, -0.000000000000000000 ) ) ;
#7161 = CIRCLE ( 'NONE', #27287, 4.999999999999997335 ) ;
#7162 = ORIENTED_EDGE ( 'NONE', *, *, #47228, .T. ) ;
#7163 = FACE_OUTER_BOUND ( 'NONE', #21012, .T. ) ;
#7164 = ORIENTED_EDGE ( 'NONE', *, *, #25715, .T. ) ;
#7165 = PLANE ( 'NONE',  #31516 ) ;
#7166 = FACE_OUTER_BOUND ( 'NONE', #48284, .T. ) ;
#7167 = EDGE_CURVE ( 'NONE', #32303, #51023, #36261, .T. ) ;
#7168 = ORIENTED_EDGE ( 'NONE', *, *, #43198, .F. ) ;
#7169 = CARTESIAN_POINT ( 'NONE',  ( -118.4510020108455706, -189.7472609257535510, 103.5805805771131105 ) ) ;
#7170 = LINE ( 'NONE', #48154, #28930 ) ;
#7171 = DIRECTION ( 'NONE',  ( 0.000000000000000000, 1.000000000000000000, 0.000000000000000000 ) ) ;
#7172 = CARTESIAN_POINT ( 'NONE',  ( 38.46761263173353740, -175.3837268820161057, 89.80681772907070126 ) ) ;
#7173 = DIRECTION ( 'NONE',  ( -1.000000000000000000, 0.000000000000000000, 0.000000000000000000 ) ) ;
#7174 = CIRCLE ( 'NONE', #44964, 124.9999999999999858 ) ;
#7175 = CARTESIAN_POINT ( 'NONE',  ( -146.0653709326077490, -189.7472609257535510, -78.11481899503409920 ) ) ;
#7176 = CARTESIAN_POINT ( 'NONE',  ( -330.4913330509368166, -123.5000000000000284, 0.000000000000000000 ) ) ;
#7178 = VERTEX_POINT ( 'NONE', #43635 ) ;
#7177 = DIRECTION ( 'NONE',  ( 1.000000000000000000, -6.525800561035029935E-17, -5.781354811211807281E-17 ) ) ;
#7179 = CIRCLE ( 'NONE', #38231, 125.0000000000000000 ) ;
#7180 = VECTOR ( 'NONE', #28154, 999.9999999999998863 ) ;
#7181 = VERTEX_POINT ( 'NONE', #38649 ) ;
#7182 = DIRECTION ( 'NONE',  ( 0.000000000000000000, 0.000000000000000000, 1.000000000000000000 ) ) ;
#7183 = EDGE_CURVE ( 'NONE', #28621, #13545, #43831, .T. ) ;
#7184 = CARTESIAN_POINT ( 'NONE',  ( 76.43863189440992301, -189.7472609257535510, -4.533605064403313456 ) ) ;
#7185 = ORIENTED_EDGE ( 'NONE', *, *, #47029, .F. ) ;
#7186 = ORIENTED_EDGE ( 'NONE', *, *, #35206, .F. ) ;
#7187 = ADVANCED_FACE ( 'NONE', ( #27076 ), #2652, .T. ) ;
#7188 = DIRECTION ( 'NONE',  ( 0.000000000000000000, 0.000000000000000000, 1.000000000000000000 ) ) ;
#7189 = AXIS2_PLACEMENT_3D ( 'NONE', #28522, #41918, #17234 ) ;
#7190 = EDGE_LOOP ( 'NONE', ( #45835, #26788, #46611, #13586 ) ) ;
#7191 = DIRECTION ( 'NONE',  ( -0.000000000000000000, 1.000000000000000000, -0.000000000000000000 ) ) ;
#7192 = DIRECTION ( 'NONE',  ( 0.000000000000000000, 1.000000000000000000, -0.000000000000000000 ) ) ;
#7193 = AXIS2_PLACEMENT_3D ( 'NONE', #9715, #45724, #5268 ) ;
#7195 = VECTOR ( 'NONE', #12302, 1000.000000000000000 ) ;
#7194 = CARTESIAN_POINT ( 'NONE',  ( 48.47907891923915003, -189.7472609257535510, 78.89300572996904748 ) ) ;
#7196 = CARTESIAN_POINT ( 'NONE',  ( 63.31225588004632243, -193.5000000000000000, 55.92572546981597981 ) ) ;
#7197 = ORIENTED_EDGE ( 'NONE', *, *, #39008, .F. ) ;
#7198 = ORIENTED_EDGE ( 'NONE', *, *, #25301, .F. ) ;
#7199 = EDGE_LOOP ( 'NONE', ( #4781, #46901, #43427, #21591 ) ) ;
#7200 = ADVANCED_FACE ( 'NONE', ( #50503 ), #47070, .F. ) ;
#7201 = VECTOR ( 'NONE', #28325, 1000.000000000000000 ) ;
#7202 = CARTESIAN_POINT ( 'NONE',  ( -330.4913330509368166, -123.9999999999993747, 59.00000000000002132 ) ) ;
#7203 = DIRECTION ( 'NONE',  ( 0.000000000000000000, -1.000000000000000000, 0.000000000000000000 ) ) ;
#7204 = CARTESIAN_POINT ( 'NONE',  ( -339.1964088526558498, -183.1207326066166559, 6.735595255827131922 ) ) ;
#7205 = CARTESIAN_POINT ( 'NONE',  ( -172.7479958471414250, -193.5000000000000000, -13.49993235881364129 ) ) ;
#7206 = DIRECTION ( 'NONE',  ( -1.000000000000000000, 0.000000000000000000, 0.000000000000000000 ) ) ;
#7207 = VERTEX_POINT ( 'NONE', #26566 ) ;
#7208 = EDGE_CURVE ( 'NONE', #37674, #13133, #14500, .T. ) ;
#7209 = CARTESIAN_POINT ( 'NONE',  ( 60.00000000000001421, -63.50000000000000000, 60.00000000000000711 ) ) ;
#7210 = CARTESIAN_POINT ( 'NONE',  ( -70.42295845586433245, -175.3837268820161057, -123.0587999703025019 ) ) ;
#7211 = ADVANCED_FACE ( 'NONE', ( #47330 ), #10540, .T. ) ;
#7212 = ORIENTED_EDGE ( 'NONE', *, *, #9952, .T. ) ;
#7213 = VERTEX_POINT ( 'NONE', #18694 ) ;
#7214 = EDGE_CURVE ( 'NONE', #37437, #46596, #34706, .T. ) ;
#7215 = VECTOR ( 'NONE', #20032, 1000.000000000000114 ) ;
#7216 = CARTESIAN_POINT ( 'NONE',  ( -92.78132261338707565, -193.5000000000000000, -116.8859077982276773 ) ) ;
#7217 = CARTESIAN_POINT ( 'NONE',  ( -336.3521761649654422, -118.0087234915157381, -58.76657425099333665 ) ) ;
#7218 = ORIENTED_EDGE ( 'NONE', *, *, #45451, .F. ) ;
#7219 = DIRECTION ( 'NONE',  ( -0.000000000000000000, 0.000000000000000000, -1.000000000000000000 ) ) ;
#7220 = CIRCLE ( 'NONE', #19809, 125.0000000000000000 ) ;
#7221 = PLANE ( 'NONE',  #15308 ) ;
#7222 = DIRECTION ( 'NONE',  ( 0.000000000000000000, 0.000000000000000000, -1.000000000000000000 ) ) ;
#7223 = EDGE_LOOP ( 'NONE', ( #13047, #6610, #42610, #48108 ) ) ;
#7224 = DIRECTION ( 'NONE',  ( 0.000000000000000000, -1.000000000000000000, 0.000000000000000000 ) ) ;
#7225 = EDGE_LOOP ( 'NONE', ( #263, #22309, #3050, #45337 ) ) ;
#7226 = CARTESIAN_POINT ( 'NONE',  ( -92.78132261338707565, -189.7472609257535510, -116.8859077982276773 ) ) ;
#7227 = CIRCLE ( 'NONE', #21484, 125.0000000000000000 ) ;
#7228 = CARTESIAN_POINT ( 'NONE',  ( -336.3521761649654422, -67.40061919120938683, 18.46045550523129819 ) ) ;
#7229 = ADVANCED_FACE ( 'NONE', ( #7633 ), #30505, .F. ) ;
#7230 = ORIENTED_EDGE ( 'NONE', *, *, #11124, .F. ) ;
#7231 = VECTOR ( 'NONE', #24546, 1000.000000000000000 ) ;
#7232 = LINE ( 'NONE', #23272, #17292 ) ;
#7233 = DIRECTION ( 'NONE',  ( -1.000000000000000000, 0.000000000000000000, 0.000000000000000000 ) ) ;
#7234 = DIRECTION ( 'NONE',  ( 0.8757349421956379665, 0.000000000000000000, -0.4827922027307427477 ) ) ;
#7235 = VECTOR ( 'NONE', #21841, 1000.000000000000114 ) ;
#7236 = DIRECTION ( 'NONE',  ( 0.000000000000000000, -1.000000000000000000, 0.000000000000000000 ) ) ;
#7238 = AXIS2_PLACEMENT_3D ( 'NONE', #33544, #14098, #2515 ) ;
#7237 = DIRECTION ( 'NONE',  ( 0.000000000000000000, 0.5680647467311485954, -0.8229838658936613482 ) ) ;
#7239 = ORIENTED_EDGE ( 'NONE', *, *, #40386, .T. ) ;
#7240 = ORIENTED_EDGE ( 'NONE', *, *, #48747, .F. ) ;
#7241 = DIRECTION ( 'NONE',  ( 0.000000000000000000, 0.000000000000000000, -1.000000000000000000 ) ) ;
#7243 = EDGE_LOOP ( 'NONE', ( #46841, #31688, #51861, #45046 ) ) ;
#7242 = CARTESIAN_POINT ( 'NONE',  ( 72.14504940832448199, -189.7472609257535510, -32.78426643622660919 ) ) ;
#7244 = ORIENTED_EDGE ( 'NONE', *, *, #26130, .T. ) ;
#7245 = DIRECTION ( 'NONE',  ( 0.000000000000000000, 0.000000000000000000, -1.000000000000000000 ) ) ;
#7246 = VERTEX_POINT ( 'NONE', #27340 ) ;
#7247 = ADVANCED_FACE ( 'NONE', ( #22637 ), #43113, .T. ) ;
#7248 = FACE_OUTER_BOUND ( 'NONE', #43339, .T. ) ;
#7249 = AXIS2_PLACEMENT_3D ( 'NONE', #27770, #48016, #12001 ) ;
#7250 = CIRCLE ( 'NONE', #1358, 125.0000000000000000 ) ;
#7251 = ORIENTED_EDGE ( 'NONE', *, *, #22156, .F. ) ;
#7252 = CARTESIAN_POINT ( 'NONE',  ( 31.84037011350117297, -193.5000000000000000, -94.47107458416898851 ) ) ;
#7253 = LINE ( 'NONE', #23293, #27104 ) ;
#7254 = EDGE_LOOP ( 'NONE', ( #49417, #39039, #23901, #23868 ) ) ;
#7255 = CARTESIAN_POINT ( 'NONE',  ( -48.47912675150885065, -189.7472609257535510, 6.938893903907228378E-15 ) ) ;
#7256 = VECTOR ( 'NONE', #7013, 1000.000000000000114 ) ;
#7257 = EDGE_CURVE ( 'NONE', #43502, #18318, #3425, .T. ) ;
#7258 = EDGE_CURVE ( 'NONE', #17693, #22066, #42601, .T. ) ;
#7259 = DIRECTION ( 'NONE',  ( -0.000000000000000000, 1.000000000000000000, -0.000000000000000000 ) ) ;
#7260 = DIRECTION ( 'NONE',  ( -1.000000000000000000, 0.000000000000000000, 0.000000000000000000 ) ) ;
#7261 = ORIENTED_EDGE ( 'NONE', *, *, #22182, .T. ) ;
#7262 = ORIENTED_EDGE ( 'NONE', *, *, #16746, .F. ) ;
#7263 = EDGE_LOOP ( 'NONE', ( #403, #2990, #50450, #1494 ) ) ;
#7264 = DIRECTION ( 'NONE',  ( -0.000000000000000000, -1.000000000000000000, -0.000000000000000000 ) ) ;
#7265 = DIRECTION ( 'NONE',  ( 0.000000000000000000, -0.000000000000000000, -1.000000000000000000 ) ) ;
#7266 = AXIS2_PLACEMENT_3D ( 'NONE', #4056, #36890, #20327 ) ;
#7267 = VECTOR ( 'NONE', #51834, 1000.000000000000000 ) ;
#7268 = AXIS2_PLACEMENT_3D ( 'NONE', #39594, #11233, #23342 ) ;
#7270 = CIRCLE ( 'NONE', #32434, 60.00000000000000000 ) ;
#7269 = PLANE ( 'NONE',  #1012 ) ;
#7271 = DIRECTION ( 'NONE',  ( 0.000000000000000000, 0.5680647467311510379, -0.8229838658936596829 ) ) ;
#7272 = ORIENTED_EDGE ( 'NONE', *, *, #26945, .T. ) ;
#7273 = EDGE_CURVE ( 'NONE', #22800, #9678, #35475, .T. ) ;
#7274 = VECTOR ( 'NONE', #21684, 1000.000000000000000 ) ;
#7275 = EDGE_CURVE ( 'NONE', #15941, #32812, #34455, .T. ) ;
#7276 = VECTOR ( 'NONE', #49234, 1000.000000000000227 ) ;
#7277 = DIRECTION ( 'NONE',  ( 0.9785564922995032555, 0.000000000000000000, 0.2059786187411021818 ) ) ;
#7278 = EDGE_LOOP ( 'NONE', ( #48814, #44338 ) ) ;
#7280 = ORIENTED_EDGE ( 'NONE', *, *, #13146, .T. ) ;
#7279 = DIRECTION ( 'NONE',  ( 0.000000000000000000, 0.000000000000000000, 1.000000000000000000 ) ) ;
#7281 = ORIENTED_EDGE ( 'NONE', *, *, #37473, .T. ) ;
#7282 = ADVANCED_FACE ( 'NONE', ( #26822 ), #42853, .T. ) ;
#7283 = DIRECTION ( 'NONE',  ( -0.000000000000000000, 1.000000000000000000, -0.000000000000000000 ) ) ;
#7284 = CARTESIAN_POINT ( 'NONE',  ( -144.8751831225492595, -189.7472609257535510, 77.99872144864770007 ) ) ;
#7285 = EDGE_CURVE ( 'NONE', #19813, #46894, #47595, .T. ) ;
#7286 = CARTESIAN_POINT ( 'NONE',  ( -339.1964088526558498, -137.1341532842531876, -57.40522506028080585 ) ) ;
#7287 = ORIENTED_EDGE ( 'NONE', *, *, #30693, .T. ) ;
#7288 = DIRECTION ( 'NONE',  ( 0.000000000000000000, 0.000000000000000000, -1.000000000000000000 ) ) ;
#7289 = ORIENTED_EDGE ( 'NONE', *, *, #46256, .F. ) ;
#7290 = EDGE_CURVE ( 'NONE', #45084, #18433, #39669, .T. ) ;
#7291 = ORIENTED_EDGE ( 'NONE', *, *, #37033, .F. ) ;
#7292 = CARTESIAN_POINT ( 'NONE',  ( 54.18765407974403558, -177.1207230881787780, -69.53890913632879744 ) ) ;
#7293 = VECTOR ( 'NONE', #28230, 1000.000000000000114 ) ;
#7294 = LINE ( 'NONE', #3082, #28088 ) ;
#7295 = VECTOR ( 'NONE', #17472, 1000.000000000000000 ) ;
#7296 = DIRECTION ( 'NONE',  ( 1.000000000000000000, -8.654812430365586465E-17, -1.050884489711573024E-17 ) ) ;
#7297 = DIRECTION ( 'NONE',  ( -0.000000000000000000, 1.000000000000000000, -0.000000000000000000 ) ) ;
#7298 = FACE_OUTER_BOUND ( 'NONE', #27077, .T. ) ;
#7299 = VECTOR ( 'NONE', #40514, 1000.000000000000114 ) ;
#7300 = CARTESIAN_POINT ( 'NONE',  ( -2.700932609314997457, -183.6283474603465606, -116.3157639405751809 ) ) ;
#7301 = FACE_OUTER_BOUND ( 'NONE', #42002, .T. ) ;
#7302 = ORIENTED_EDGE ( 'NONE', *, *, #18717, .T. ) ;
#7303 = CARTESIAN_POINT ( 'NONE',  ( -125.5794209599708751, -177.1207230881787780, 97.11716833071891131 ) ) ;
#7304 = PLANE ( 'NONE',  #17322 ) ;
#7305 = DIRECTION ( 'NONE',  ( -0.000000000000000000, 1.000000000000000000, -0.000000000000000000 ) ) ;
#7306 = ORIENTED_EDGE ( 'NONE', *, *, #27782, .T. ) ;
#7307 = VECTOR ( 'NONE', #2688, 999.9999999999998863 ) ;
#7308 = VECTOR ( 'NONE', #19433, 1000.000000000000114 ) ;
#7309 = DIRECTION ( 'NONE',  ( -0.9995608365087944591, 0.000000000000000000, 0.02963332782255633305 ) ) ;
#7310 = CIRCLE ( 'NONE', #30783, 125.0000000000000000 ) ;
#7311 = VECTOR ( 'NONE', #30820, 1000.000000000000000 ) ;
#7312 = LINE ( 'NONE', #18864, #29465 ) ;
#7313 = ORIENTED_EDGE ( 'NONE', *, *, #21739, .T. ) ;
#7314 = PLANE ( 'NONE',  #3604 ) ;
#7315 = AXIS2_PLACEMENT_3D ( 'NONE', #1108, #5338, #21352 ) ;
#7316 = ORIENTED_EDGE ( 'NONE', *, *, #127, .F. ) ;
#7317 = VECTOR ( 'NONE', #48914, 1000.000000000000000 ) ;
#7318 = CARTESIAN_POINT ( 'NONE',  ( 12.99855592850622443, -193.5000000000000000, 108.8370090194294875 ) ) ;
#7319 = FACE_BOUND ( 'NONE', #20636, .T. ) ;
#7320 = ADVANCED_FACE ( 'NONE', ( #34968 ), #15022, .T. ) ;
#7322 = ORIENTED_EDGE ( 'NONE', *, *, #31324, .T. ) ;
#7321 = LINE ( 'NONE', #14683, #41367 ) ;
#7323 = ADVANCED_FACE ( 'NONE', ( #19708 ), #24191, .T. ) ;
#7324 = EDGE_CURVE ( 'NONE', #26956, #20647, #7881, .T. ) ;
#7325 = EDGE_CURVE ( 'NONE', #21917, #22206, #27850, .T. ) ;
#7326 = FACE_OUTER_BOUND ( 'NONE', #50786, .T. ) ;
#7327 = ORIENTED_EDGE ( 'NONE', *, *, #2986, .T. ) ;
#7328 = ADVANCED_FACE ( 'NONE', ( #4471 ), #48100, .T. ) ;
#7329 = VERTEX_POINT ( 'NONE', #12342 ) ;
#7330 = DIRECTION ( 'NONE',  ( 0.7765238627180437447, 0.000000000000000000, -0.6300878435817094392 ) ) ;
#7331 = CIRCLE ( 'NONE', #22451, 125.0000000000000000 ) ;
#7332 = CIRCLE ( 'NONE', #10664, 125.0000000000000000 ) ;
#7333 = VERTEX_POINT ( 'NONE', #15802 ) ;
#7334 = ADVANCED_FACE ( 'NONE', ( #32309 ), #40203, .F. ) ;
#7335 = DIRECTION ( 'NONE',  ( 0.000000000000000000, 0.000000000000000000, -1.000000000000000000 ) ) ;
#7336 = CIRCLE ( 'NONE', #1481, 60.00000000000000000 ) ;
#7337 = EDGE_CURVE ( 'NONE', #7798, #24942, #15306, .T. ) ;
#7338 = EDGE_CURVE ( 'NONE', #20222, #50025, #32583, .T. ) ;
#7339 = FACE_OUTER_BOUND ( 'NONE', #35181, .T. ) ;
#7340 = LINE ( 'NONE', #19663, #29814 ) ;
#7341 = ORIENTED_EDGE ( 'NONE', *, *, #44171, .F. ) ;
#7344 = ORIENTED_EDGE ( 'NONE', *, *, #559, .T. ) ;
#7343 = LINE ( 'NONE', #34914, #18039 ) ;
#7342 = DIRECTION ( 'NONE',  ( 1.000000000000000000, -0.000000000000000000, -0.000000000000000000 ) ) ;
#7345 = CIRCLE ( 'NONE', #14893, 125.0000000000000000 ) ;
#7346 = EDGE_CURVE ( 'NONE', #51078, #33364, #20235, .T. ) ;
#7347 = AXIS2_PLACEMENT_3D ( 'NONE', #20308, #25298, #8479 ) ;
#7348 = AXIS2_PLACEMENT_3D ( 'NONE', #11210, #51438, #40105 ) ;
#7349 = PLANE ( 'NONE',  #10534 ) ;
#7350 = ORIENTED_EDGE ( 'NONE', *, *, #37180, .T. ) ;
#7351 = FACE_OUTER_BOUND ( 'NONE', #23757, .T. ) ;
#7352 = ORIENTED_EDGE ( 'NONE', *, *, #32645, .F. ) ;
#7353 = EDGE_CURVE ( 'NONE', #12905, #30781, #4216, .T. ) ;
#7354 = CIRCLE ( 'NONE', #40083, 12.00000000000000000 ) ;
#7355 = CARTESIAN_POINT ( 'NONE',  ( -8.461066480258370603, -183.6283474603465606, 117.3655938605930231 ) ) ;
#7356 = ORIENTED_EDGE ( 'NONE', *, *, #48637, .T. ) ;
#7358 = DIRECTION ( 'NONE',  ( -0.000000000000000000, -0.6631226582407964143, -0.7485107481710999711 ) ) ;
#7357 = DIRECTION ( 'NONE',  ( 0.000000000000000000, -0.4647231720437631775, 0.8854560256532126861 ) ) ;
#7359 = ORIENTED_EDGE ( 'NONE', *, *, #44731, .T. ) ;
#7360 = EDGE_CURVE ( 'NONE', #3383, #14589, #6091, .T. ) ;
#7361 = VECTOR ( 'NONE', #46321, 1000.000000000000227 ) ;
#7362 = DIRECTION ( 'NONE',  ( -0.000000000000000000, -0.8229838658936596829, -0.5680647467311510379 ) ) ;
#7363 = ORIENTED_EDGE ( 'NONE', *, *, #34386, .T. ) ;
#7364 = CARTESIAN_POINT ( 'NONE',  ( -48.36085358058748085, -193.5000000000000000, -0.9929810960135100339 ) ) ;
#7365 = FACE_OUTER_BOUND ( 'NONE', #37162, .T. ) ;
#7366 = CARTESIAN_POINT ( 'NONE',  ( -171.7300019102062265, -183.6283474603465606, -20.83798868929513759 ) ) ;
#7367 = CARTESIAN_POINT ( 'NONE',  ( -339.1964088526558498, -182.0095552316575152, 7.608018572113563138 ) ) ;
#7368 = CARTESIAN_POINT ( 'NONE',  ( -98.10897907742933910, -189.7472609257535510, 114.7252272087849434 ) ) ;
#7369 = CARTESIAN_POINT ( 'NONE',  ( -103.4012653778457320, -177.1207230881787780, -112.2878385610366649 ) ) ;
#7370 = VERTEX_POINT ( 'NONE', #16296 ) ;
#7371 = CARTESIAN_POINT ( 'NONE',  ( 22.37192613399954411, -3.469446951953614189E-15, -6.938893903907228378E-15 ) ) ;
#7372 = CARTESIAN_POINT ( 'NONE',  ( -49.21696003055058810, -175.3837268820161057, 0.6749830015182108900 ) ) ;
#7373 = ADVANCED_FACE ( 'NONE', ( #9 ), #48360, .T. ) ;
#7374 = DIRECTION ( 'NONE',  ( 0.000000000000000000, 1.000000000000000000, 0.000000000000000000 ) ) ;
#7375 = DIRECTION ( 'NONE',  ( -0.000000000000000000, 1.000000000000000000, -0.000000000000000000 ) ) ;
#7376 = ORIENTED_EDGE ( 'NONE', *, *, #3632, .T. ) ;
#7377 = AXIS2_PLACEMENT_3D ( 'NONE', #45813, #28719, #13235 ) ;
#7378 = CARTESIAN_POINT ( 'NONE',  ( -171.2727421180348415, -183.6283474603465606, 23.38221600314376047 ) ) ;
#7379 = DIRECTION ( 'NONE',  ( -0.1768902751225802927, 0.000000000000000000, 0.9842305779475953864 ) ) ;
#7380 = VECTOR ( 'NONE', #34279, 1000.000000000000000 ) ;
#7381 = FACE_OUTER_BOUND ( 'NONE', #33340, .T. ) ;
#7383 = ORIENTED_EDGE ( 'NONE', *, *, #9598, .F. ) ;
#7382 = CARTESIAN_POINT ( 'NONE',  ( -330.4913330509368166, -64.50000000000000000, 0.4999999999999551470 ) ) ;
#7384 = VERTEX_POINT ( 'NONE', #12071 ) ;
#7385 = ORIENTED_EDGE ( 'NONE', *, *, #911, .T. ) ;
#7386 = EDGE_CURVE ( 'NONE', #40758, #12830, #26207, .T. ) ;
#7387 = AXIS2_PLACEMENT_3D ( 'NONE', #33233, #49281, #5661 ) ;
#7388 = DIRECTION ( 'NONE',  ( 0.000000000000000000, -1.350771346627273875E-13, 1.000000000000000000 ) ) ;
#7389 = CARTESIAN_POINT ( 'NONE',  ( -332.3517673607765914, -91.32752733096738496, -49.48329383994654052 ) ) ;
#7390 = DIRECTION ( 'NONE',  ( -1.000000000000000000, -0.000000000000000000, 0.000000000000000000 ) ) ;
#7391 = CARTESIAN_POINT ( 'NONE',  ( 14.37129481273059106, -189.7472609257535510, -108.0501018472328241 ) ) ;
#7392 = ORIENTED_EDGE ( 'NONE', *, *, #38552, .F. ) ;
#7393 = ADVANCED_FACE ( 'NONE', ( #786 ), #44423, .F. ) ;
#7394 = EDGE_CURVE ( 'NONE', #15211, #30309, #44937, .T. ) ;
#7395 = CARTESIAN_POINT ( 'NONE',  ( 2.248499775674169587, 57.57581846653669544, -16.67809192707658639 ) ) ;
#7396 = EDGE_CURVE ( 'NONE', #24085, #27896, #8580, .T. ) ;
#7397 = VECTOR ( 'NONE', #14707, 1000.000000000000114 ) ;
#7398 = EDGE_CURVE ( 'NONE', #25917, #14780, #36299, .T. ) ;
#7399 = ORIENTED_EDGE ( 'NONE', *, *, #32888, .F. ) ;
#7400 = ORIENTED_EDGE ( 'NONE', *, *, #12054, .F. ) ;
#7401 = ORIENTED_EDGE ( 'NONE', *, *, #51445, .T. ) ;
#7402 = CARTESIAN_POINT ( 'NONE',  ( -332.3517673607765914, -136.0347666902908372, 57.67619951860663718 ) ) ;
#7403 = CARTESIAN_POINT ( 'NONE',  ( -330.4913330509368166, -89.82879061784626629, 49.66134974749640207 ) ) ;
#7404 = ORIENTED_EDGE ( 'NONE', *, *, #22270, .T. ) ;
#7405 = DIRECTION ( 'NONE',  ( 0.7765238627180393038, 0.000000000000000000, 0.6300878435817147682 ) ) ;
#7406 = DIRECTION ( 'NONE',  ( 0.000000000000000000, 6.245004513516505540E-15, 1.000000000000000000 ) ) ;
#7409 = ORIENTED_EDGE ( 'NONE', *, *, #44071, .F. ) ;
#7408 = PLANE ( 'NONE',  #30000 ) ;
#7407 = CARTESIAN_POINT ( 'NONE',  ( -48.30223647638628393, -193.5000000000000000, 0.9842305779476049343 ) ) ;
#7410 = AXIS2_PLACEMENT_3D ( 'NONE', #39579, #7028, #42770 ) ;
#7411 = EDGE_CURVE ( 'NONE', #7901, #33568, #41774, .T. ) ;
#7412 = VECTOR ( 'NONE', #12084, 1000.000000000000000 ) ;
#7413 = CARTESIAN_POINT ( 'NONE',  ( -332.3517673607765914, -181.1761995186066088, -12.53476669029101842 ) ) ;
#7414 = ADVANCED_BREP_SHAPE_REPRESENTATION ( '', ( #2369, #31742 ), #3199 ) ;
#7415 = ORIENTED_EDGE ( 'NONE', *, *, #6085, .F. ) ;
#7416 = PLANE ( 'NONE',  #12109 ) ;
#7417 = VECTOR ( 'NONE', #28111, 1000.000000000000000 ) ;
#7418 = VERTEX_POINT ( 'NONE', #37037 ) ;
#7419 = EDGE_CURVE ( 'NONE', #29336, #9008, #11947, .T. ) ;
#7420 = FACE_OUTER_BOUND ( 'NONE', #2762, .T. ) ;
#7421 = DIRECTION ( 'NONE',  ( -0.000000000000000000, 1.000000000000000000, -0.000000000000000000 ) ) ;
#7423 = CARTESIAN_POINT ( 'NONE',  ( -138.3664773286545824, -177.1207230881787780, -85.41934182508016704 ) ) ;
#7422 = DIRECTION ( 'NONE',  ( -0.000000000000000000, 1.000000000000000000, 0.000000000000000000 ) ) ;
#7424 = ORIENTED_EDGE ( 'NONE', *, *, #50605, .T. ) ;
#7425 = ADVANCED_FACE ( 'NONE', ( #5793 ), #21019, .F. ) ;
#7426 = VECTOR ( 'NONE', #6810, 1000.000000000000000 ) ;
#7427 = CARTESIAN_POINT ( 'NONE',  ( -132.6364218684650211, -177.1207230881787780, 92.42591454022807795 ) ) ;
#7428 = CARTESIAN_POINT ( 'NONE',  ( -48.47912675150885065, -177.1207230881787780, 6.938893903907228378E-15 ) ) ;
#7429 = VERTEX_POINT ( 'NONE', #40985 ) ;
#7430 = DIRECTION ( 'NONE',  ( -0.4031234292879600778, 0.000000000000000000, -0.9151456172430237901 ) ) ;
#7431 = LINE ( 'NONE', #19491, #20645 ) ;
#7432 = EDGE_LOOP ( 'NONE', ( #14473, #11227, #18639, #30654 ) ) ;
#7433 = DIRECTION ( 'NONE',  ( -0.000000000000000000, 1.000000000000000000, -0.000000000000000000 ) ) ;
#7434 = LINE ( 'NONE', #2694, #51679 ) ;
#7435 = AXIS2_PLACEMENT_3D ( 'NONE', #3647, #39128, #16013 ) ;
#7436 = ORIENTED_EDGE ( 'NONE', *, *, #46958, .T. ) ;
#7437 = DIRECTION ( 'NONE',  ( 0.000000000000000000, 0.000000000000000000, 1.000000000000000000 ) ) ;
#7438 = VERTEX_POINT ( 'NONE', #50191 ) ;
#7439 = DIRECTION ( 'NONE',  ( 0.000000000000000000, 0.000000000000000000, 1.000000000000000000 ) ) ;
#7440 = CARTESIAN_POINT ( 'NONE',  ( 44.41590053910517355, 28.88712326890129845, -48.99342751026321707 ) ) ;
#7441 = CARTESIAN_POINT ( 'NONE',  ( -330.4913330509368166, -182.5000000000000568, 0.4999999999999549249 ) ) ;
#7442 = CARTESIAN_POINT ( 'NONE',  ( -86.93810158023208601, -193.5000000000000000, 117.8859915627477193 ) ) ;
#7443 = PLANE ( 'NONE',  #29070 ) ;
#7444 = CARTESIAN_POINT ( 'NONE',  ( -82.43766229206461560, -193.5000000000000000, -119.2602935412679841 ) ) ;
#7445 = AXIS2_PLACEMENT_3D ( 'NONE', #26681, #26925, #11408 ) ;
#7446 = STYLED_ITEM ( 'NONE', ( #27799 ), #36582 ) ;
#7447 = DIRECTION ( 'NONE',  ( 0.4827922027307490205, 0.000000000000000000, -0.8757349421956345248 ) ) ;
#7448 = CARTESIAN_POINT ( 'NONE',  ( -336.3521761649654422, -135.2893155068536828, 58.83036664750492406 ) ) ;
#7450 = VERTEX_POINT ( 'NONE', #13913 ) ;
#7449 = DIRECTION ( 'NONE',  ( 0.000000000000000000, 0.000000000000000000, -1.000000000000000000 ) ) ;
#7451 = COLOUR_RGB ( '', 0.08235294, 0.09019608, 0.10196078) ;
#7452 = ORIENTED_EDGE ( 'NONE', *, *, #22331, .T. ) ;
#7453 = EDGE_CURVE ( 'NONE', #48867, #44102, #9454, .T. ) ;
#7454 = EDGE_CURVE ( 'NONE', #11814, #5285, #16171, .T. ) ;
#7455 = CARTESIAN_POINT ( 'NONE',  ( 64.44365795514079309, -175.3837268820161057, -53.60452120946194299 ) ) ;
#7456 = PLANE ( 'NONE',  #17889 ) ;
#7457 = ORIENTED_EDGE ( 'NONE', *, *, #41879, .F. ) ;
#7458 = ORIENTED_EDGE ( 'NONE', *, *, #28375, .F. ) ;
#7459 = DIRECTION ( 'NONE',  ( 0.000000000000000000, 0.000000000000000000, -1.000000000000000000 ) ) ;
#7460 = VERTEX_POINT ( 'NONE', #17092 ) ;
#7461 = DIRECTION ( 'NONE',  ( -8.718379230999707126E-17, 0.000000000000000000, 1.000000000000000000 ) ) ;
#7462 = DIRECTION ( 'NONE',  ( -5.399917434947259359E-17, -1.000000000000000000, 0.000000000000000000 ) ) ;
#7463 = DIRECTION ( 'NONE',  ( 0.3482016354343928088, 0.000000000000000000, 0.9374196611341231167 ) ) ;
#7464 = PLANE ( 'NONE',  #40038 ) ;
#7465 = VERTEX_POINT ( 'NONE', #25224 ) ;
#7466 = VERTEX_POINT ( 'NONE', #49415 ) ;
#7467 = VERTEX_POINT ( 'NONE', #30202 ) ;
#7468 = CIRCLE ( 'NONE', #50278, 125.0000000000000000 ) ;
#7469 = CARTESIAN_POINT ( 'NONE',  ( -155.4465502054561057, -177.1207230881787780, 64.67588669375881238 ) ) ;
#7470 = DIRECTION ( 'NONE',  ( 1.000000000000000000, -0.000000000000000000, -0.000000000000000000 ) ) ;
#7471 = PLANE ( 'NONE',  #33297 ) ;
#7472 = EDGE_CURVE ( 'NONE', #14905, #4633, #41493, .T. ) ;
#7473 = CARTESIAN_POINT ( 'NONE',  ( -1.771278280434274155, -183.6283474603465606, -115.9455772817710226 ) ) ;
#7474 = DIRECTION ( 'NONE',  ( 0.000000000000000000, 1.000000000000000000, 0.000000000000000000 ) ) ;
#7475 = ORIENTED_EDGE ( 'NONE', *, *, #29964, .F. ) ;
#7476 = PRODUCT_DEFINITION_CONTEXT ( 'detailed design', #35726, 'design' ) ;
#7477 = CARTESIAN_POINT ( 'NONE',  ( -49.13194886969938580, -183.6283474603465606, 0.7575112421616214675 ) ) ;
#7478 = PLANE ( 'NONE',  #11423 ) ;
#7479 = EDGE_CURVE ( 'NONE', #14630, #563, #22882, .T. ) ;
#7480 = ORIENTED_EDGE ( 'NONE', *, *, #17258, .T. ) ;
#7481 = VERTEX_POINT ( 'NONE', #5525 ) ;
#7482 = ORIENTED_EDGE ( 'NONE', *, *, #16794, .T. ) ;
#7483 = DIRECTION ( 'NONE',  ( -0.000000000000000000, 1.000000000000000000, -0.000000000000000000 ) ) ;
#7485 = VECTOR ( 'NONE', #42011, 1000.000000000000000 ) ;
#7484 = CARTESIAN_POINT ( 'NONE',  ( -336.3521761649654422, -118.0087234915157381, -58.76657425099333665 ) ) ;
#7486 = EDGE_LOOP ( 'NONE', ( #17888, #47227, #7625, #15498 ) ) ;
#7487 = CARTESIAN_POINT ( 'NONE',  ( -339.1964088526558498, -108.8949048983204051, 57.16590939599314680 ) ) ;
#7488 = VECTOR ( 'NONE', #38142, 1000.000000000000000 ) ;
#7489 = PLANE ( 'NONE',  #3554 ) ;
#7490 = CARTESIAN_POINT ( 'NONE',  ( -82.43766229206461560, -177.1207230881787780, -119.2602935412679983 ) ) ;
#7491 = EDGE_LOOP ( 'NONE', ( #3558, #36708, #51194, #12288 ) ) ;
#7492 = CARTESIAN_POINT ( 'NONE',  ( 76.28370911321320591, -183.6283474603465606, -7.696413904697499753 ) ) ;
#7493 = ORIENTED_EDGE ( 'NONE', *, *, #3836, .T. ) ;
#7494 = LINE ( 'NONE', #47179, #42245 ) ;
#7495 = CARTESIAN_POINT ( 'NONE',  ( -121.0298553105864414, -177.1207230881787780, -100.5610240384919081 ) ) ;
#7496 = ORIENTED_EDGE ( 'NONE', *, *, #10889, .F. ) ;
#7497 = CYLINDRICAL_SURFACE ( 'NONE', #35759, 4.999999999999997335 ) ;
#7498 = PLANE ( 'NONE',  #38124 ) ;
#7499 = CARTESIAN_POINT ( 'NONE',  ( -172.1767935149754294, -193.5000000000000000, 8.665274887906335266 ) ) ;
#7500 = DIRECTION ( 'NONE',  ( -0.6528221181905280446, 0.000000000000000000, 0.7575112421616145841 ) ) ;
#7501 = VECTOR ( 'NONE', #24021, 1000.000000000000000 ) ;
#7502 = EDGE_CURVE ( 'NONE', #39834, #34082, #37572, .T. ) ;
#7503 = LINE ( 'NONE', #8008, #28662 ) ;
#7504 = ORIENTED_EDGE ( 'NONE', *, *, #50052, .F. ) ;
#7505 = VERTEX_POINT ( 'NONE', #45716 ) ;
#7506 = DIRECTION ( 'NONE',  ( 0.000000000000000000, 0.000000000000000000, 1.000000000000000000 ) ) ;
#7508 = ORIENTED_EDGE ( 'NONE', *, *, #10450, .T. ) ;
#7507 = DIRECTION ( 'NONE',  ( -0.000000000000000000, 0.8229838658936634577, 0.5680647467311457088 ) ) ;
#7509 = VERTEX_POINT ( 'NONE', #38070 ) ;
#7510 = DIRECTION ( 'NONE',  ( 0.000000000000000000, -1.000000000000000000, 0.000000000000000000 ) ) ;
#7511 = EDGE_CURVE ( 'NONE', #16448, #12506, #46243, .T. ) ;
#7512 = CARTESIAN_POINT ( 'NONE',  ( -47.74129347246713451, -177.1207230881787780, 0.6749830015182212151 ) ) ;
#7513 = EDGE_CURVE ( 'NONE', #20061, #11975, #13397, .T. ) ;
#7514 = ORIENTED_EDGE ( 'NONE', *, *, #22895, .T. ) ;
#7515 = AXIS2_PLACEMENT_3D ( 'NONE', #20167, #36186, #40914 ) ;
#7516 = FACE_BOUND ( 'NONE', #18343, .T. ) ;
#7517 = CARTESIAN_POINT ( 'NONE',  ( -330.4913330509368166, -157.4273119900845757, 48.27201571436049932 ) ) ;
#7518 = ORIENTED_EDGE ( 'NONE', *, *, #4188, .T. ) ;
#7519 = DIRECTION ( 'NONE',  ( -0.000000000000000000, -0.8229838658936596829, -0.5680647467311510379 ) ) ;
#7520 = DIRECTION ( 'NONE',  ( -0.000000000000000000, 1.000000000000000000, -0.000000000000000000 ) ) ;
#7521 = CIRCLE ( 'NONE', #36891, 125.0000000000000000 ) ;
#7522 = PLANE ( 'NONE',  #12635 ) ;
#7523 = CARTESIAN_POINT ( 'NONE',  ( -162.9896759831412965, -177.1207230881787780, -50.12318939043961308 ) ) ;
#7524 = ORIENTED_EDGE ( 'NONE', *, *, #44163, .F. ) ;
#7525 = ORIENTED_EDGE ( 'NONE', *, *, #6272, .F. ) ;
#7526 = ORIENTED_EDGE ( 'NONE', *, *, #12854, .T. ) ;
#7527 = DIRECTION ( 'NONE',  ( 0.000000000000000000, 0.000000000000000000, 1.000000000000000000 ) ) ;
#7528 = CARTESIAN_POINT ( 'NONE',  ( -330.4913330509368166, -182.5000000000000568, 0.4999999999999549249 ) ) ;
#7529 = EDGE_CURVE ( 'NONE', #29784, #17455, #43021, .T. ) ;
#7530 = LINE ( 'NONE', #39563, #51990 ) ;
#7531 = PLANE ( 'NONE',  #6053 ) ;
#7532 = CARTESIAN_POINT ( 'NONE',  ( -336.3521761649654422, -177.7325358280884586, 23.38292116578760726 ) ) ;
#7533 = VERTEX_POINT ( 'NONE', #9709 ) ;
#7534 = VECTOR ( 'NONE', #32787, 1000.000000000000114 ) ;
#7535 = CARTESIAN_POINT ( 'NONE',  ( -49.17567778057185990, -183.6283474603465606, 0.7175072570443320474 ) ) ;
#7536 = ORIENTED_EDGE ( 'NONE', *, *, #24433, .F. ) ;
#7538 = ORIENTED_EDGE ( 'NONE', *, *, #33519, .T. ) ;
#7537 = FACE_OUTER_BOUND ( 'NONE', #25242, .T. ) ;
#7539 = EDGE_LOOP ( 'NONE', ( #22858, #5471, #13616, #44308 ) ) ;
#7540 = FACE_OUTER_BOUND ( 'NONE', #41794, .T. ) ;
#7541 = CARTESIAN_POINT ( 'NONE',  ( -339.1964088526558498, -124.0000000000002700, -59.00000000000002132 ) ) ;
#7542 = LINE ( 'NONE', #31713, #42267 ) ;
#7543 = PLANE ( 'NONE',  #5797 ) ;
#7544 = ORIENTED_EDGE ( 'NONE', *, *, #24257, .F. ) ;
#7545 = LINE ( 'NONE', #31190, #17480 ) ;
#7546 = VERTEX_POINT ( 'NONE', #21548 ) ;
#7547 = ORIENTED_EDGE ( 'NONE', *, *, #36563, .F. ) ;
#7548 = DIRECTION ( 'NONE',  ( 0.6068001458185890984, 0.000000000000000000, 0.7948544414133565938 ) ) ;
#7549 = PLANE ( 'NONE',  #40691 ) ;
#7550 = AXIS2_PLACEMENT_3D ( 'NONE', #14188, #13918, #18634 ) ;
#7551 = DIRECTION ( 'NONE',  ( 0.9929810960135161402, 0.000000000000000000, 0.1182731709213730997 ) ) ;
#7552 = DIRECTION ( 'NONE',  ( 0.000000000000000000, 0.5680647467311540355, -0.8229838658936575735 ) ) ;
#7553 = DIRECTION ( 'NONE',  ( 0.6068001458185945385, 0.000000000000000000, -0.7948544414133523750 ) ) ;
#7554 = EDGE_CURVE ( 'NONE', #49617, #16076, #17611, .T. ) ;
#7555 = CARTESIAN_POINT ( 'NONE',  ( -336.3521761649654422, -123.5000000000000284, 0.000000000000000000 ) ) ;
#7556 = CARTESIAN_POINT ( 'NONE',  ( -131.9398708394020332, -193.5000000000000000, 91.70840728318374602 ) ) ;
#7557 = ORIENTED_EDGE ( 'NONE', *, *, #37236, .T. ) ;
#7558 = DIRECTION ( 'NONE',  ( -1.000000000000000000, 0.000000000000000000, 0.000000000000000000 ) ) ;
#7559 = DIRECTION ( 'NONE',  ( -0.000000000000000000, 0.9350162426854146114, -0.3546048870425363986 ) ) ;
#7560 = CARTESIAN_POINT ( 'NONE',  ( -48.47912675150885065, -175.3837268820161057, 6.938893903907228378E-15 ) ) ;
#7561 = ORIENTED_EDGE ( 'NONE', *, *, #31698, .F. ) ;
#7562 = CARTESIAN_POINT ( 'NONE',  ( -173.4190745413846741, -189.7472609257535510, -3.874202661595026687 ) ) ;
#7563 = FACE_OUTER_BOUND ( 'NONE', #22219, .T. ) ;
#7564 = ORIENTED_EDGE ( 'NONE', *, *, #24403, .F. ) ;
#7565 = DIRECTION ( 'NONE',  ( 0.000000000000000000, -0.4647231720437604574, 0.8854560256532141294 ) ) ;
#7566 = ADVANCED_FACE ( 'NONE', ( #1814 ), #34140, .T. ) ;
#7567 = ORIENTED_EDGE ( 'NONE', *, *, #39485, .T. ) ;
#7568 = EDGE_CURVE ( 'NONE', #25658, #40221, #33371, .T. ) ;
#7569 = EDGE_CURVE ( 'NONE', #20596, #32896, #42014, .T. ) ;
#7570 = AXIS2_PLACEMENT_3D ( 'NONE', #37377, #21091, #12676 ) ;
#7571 = VECTOR ( 'NONE', #10666, 1000.000000000000000 ) ;
#7572 = CARTESIAN_POINT ( 'NONE',  ( -330.4913330509368166, -163.6602333390095509, 44.57752413668021774 ) ) ;
#7573 = ADVANCED_FACE ( 'NONE', ( #25477 ), #46753, .T. ) ;
#7574 = FACE_BOUND ( 'NONE', #43085, .T. ) ;
#7575 = PLANE ( 'NONE',  #30447 ) ;
#7576 = DIRECTION ( 'NONE',  ( 0.000000000000000000, 1.000000000000000000, 0.000000000000000000 ) ) ;
#7577 = ORIENTED_EDGE ( 'NONE', *, *, #31900, .F. ) ;
#7578 = EDGE_LOOP ( 'NONE', ( #11648, #40783, #16733, #14126 ) ) ;
#7579 = CARTESIAN_POINT ( 'NONE',  ( 116.9235303384055840, -193.5000000000000000, 2.819679052520814125E-14 ) ) ;
#7580 = VECTOR ( 'NONE', #40383, 1000.000000000000000 ) ;
#7581 = ORIENTED_EDGE ( 'NONE', *, *, #2266, .T. ) ;
#7582 = LINE ( 'NONE', #19928, #16690 ) ;
#7583 = DIRECTION ( 'NONE',  ( 0.000000000000000000, -0.4647231720437604574, 0.8854560256532141294 ) ) ;
#7584 = DIRECTION ( 'NONE',  ( 0.1182731709213660498, 0.000000000000000000, -0.9929810960135169173 ) ) ;
#7585 = ORIENTED_EDGE ( 'NONE', *, *, #43170, .T. ) ;
#7588 = ORIENTED_EDGE ( 'NONE', *, *, #45633, .T. ) ;
#7587 =( LENGTH_UNIT ( ) NAMED_UNIT ( * ) SI_UNIT ( .MILLI., .METRE. ) );
#7586 = CARTESIAN_POINT ( 'NONE',  ( 0.000000000000000000, -53.50000000000000000, 0.000000000000000000 ) ) ;
#7589 = ORIENTED_EDGE ( 'NONE', *, *, #32049, .T. ) ;
#7590 = CARTESIAN_POINT ( 'NONE',  ( -48.47912675150885065, -177.1207230881787780, 6.938893903907228378E-15 ) ) ;
#7591 = ORIENTED_EDGE ( 'NONE', *, *, #9974, .F. ) ;
#7592 = CARTESIAN_POINT ( 'NONE',  ( -169.6719064342497632, -193.5000000000000000, 30.61552143554992256 ) ) ;
#7593 = ORIENTED_EDGE ( 'NONE', *, *, #42921, .F. ) ;
#7594 = DIRECTION ( 'NONE',  ( 0.000000000000000000, 0.1205366802553303057, 0.9927088740980530845 ) ) ;
#7595 = EDGE_LOOP ( 'NONE', ( #21054, #22514, #45764, #46747 ) ) ;
#7597 = DIRECTION ( 'NONE',  ( 0.000000000000000000, 0.000000000000000000, 1.000000000000000000 ) ) ;
#7596 = FACE_OUTER_BOUND ( 'NONE', #9269, .T. ) ;
#7598 = ORIENTED_EDGE ( 'NONE', *, *, #46092, .F. ) ;
#7599 = AXIS2_PLACEMENT_3D ( 'NONE', #41849, #5866, #37901 ) ;
#7600 = CIRCLE ( 'NONE', #21034, 125.0000000000000000 ) ;
#7601 = PLANE ( 'NONE',  #31566 ) ;
#7602 = VERTEX_POINT ( 'NONE', #18630 ) ;
#7603 = CARTESIAN_POINT ( 'NONE',  ( 53.18081239921338721, -193.5000000000000000, -72.73415134495935774 ) ) ;
#7604 = DIRECTION ( 'NONE',  ( 0.1476465640024851034, 0.000000000000000000, -0.9890401873221634776 ) ) ;
#7605 = DIRECTION ( 'NONE',  ( -1.000000000000000000, 0.000000000000000000, 0.000000000000000000 ) ) ;
#7606 = DIRECTION ( 'NONE',  ( 0.000000000000000000, -1.000000000000000000, -0.000000000000000000 ) ) ;
#7607 = LINE ( 'NONE', #48337, #24078 ) ;
#7608 = CARTESIAN_POINT ( 'NONE',  ( -48.47912675150885065, -132.5479369270331915, 6.938893903907228378E-15 ) ) ;
#7609 = EDGE_CURVE ( 'NONE', #39961, #15284, #2597, .T. ) ;
#7610 = EDGE_CURVE ( 'NONE', #19801, #34735, #46489, .T. ) ;
#7611 = ORIENTED_EDGE ( 'NONE', *, *, #36528, .F. ) ;
#7612 = EDGE_CURVE ( 'NONE', #47296, #8540, #34400, .T. ) ;
#7613 = DIRECTION ( 'NONE',  ( 1.000000000000000000, 0.000000000000000000, 0.000000000000000000 ) ) ;
#7614 = CARTESIAN_POINT ( 'NONE',  ( 46.00000000000000711, -42.50000000000000000, -46.00000000000000000 ) ) ;
#7615 = DIRECTION ( 'NONE',  ( -1.000000000000000000, -0.000000000000000000, -0.000000000000000000 ) ) ;
#7616 = EDGE_CURVE ( 'NONE', #33685, #37521, #42187, .T. ) ;
#7617 = CARTESIAN_POINT ( 'NONE',  ( -339.1964088526558498, -167.3305728129748786, -39.49849221029221269 ) ) ;
#7618 = ORIENTED_EDGE ( 'NONE', *, *, #24791, .F. ) ;
#7619 = AXIS2_PLACEMENT_3D ( 'NONE', #49018, #28254, #43766 ) ;
#7620 = FACE_OUTER_BOUND ( 'NONE', #29471, .T. ) ;
#7621 = EDGE_CURVE ( 'NONE', #49340, #1605, #249, .T. ) ;
#7622 = FACE_OUTER_BOUND ( 'NONE', #36688, .T. ) ;
#7624 = ORIENTED_EDGE ( 'NONE', *, *, #44298, .F. ) ;
#7623 = PLANE ( 'NONE',  #9022 ) ;
#7625 = ORIENTED_EDGE ( 'NONE', *, *, #31760, .F. ) ;
#7626 = EDGE_CURVE ( 'NONE', #12568, #44736, #6284, .T. ) ;
#7627 = ORIENTED_EDGE ( 'NONE', *, *, #18153, .T. ) ;
#7628 = EDGE_CURVE ( 'NONE', #36353, #43146, #10741, .T. ) ;
#7629 = PLANE ( 'NONE',  #15354 ) ;
#7630 = EDGE_CURVE ( 'NONE', #3016, #34125, #19397, .T. ) ;
#7631 = CARTESIAN_POINT ( 'NONE',  ( -105.4063847101409692, -193.5000000000000000, -111.2847127925096231 ) ) ;
#7632 = CARTESIAN_POINT ( 'NONE',  ( -332.3517673607765914, -147.2170408776451609, -55.11353710303946940 ) ) ;
#7633 = FACE_OUTER_BOUND ( 'NONE', #42194, .T. ) ;
#7634 = VECTOR ( 'NONE', #14741, 1000.000000000000000 ) ;
#7635 = EDGE_CURVE ( 'NONE', #8800, #31552, #7321, .T. ) ;
#7636 = ORIENTED_EDGE ( 'NONE', *, *, #5318, .F. ) ;
#7637 = CARTESIAN_POINT ( 'NONE',  ( -1.600401561467127700E-24, 58.14470866581338271, -16.45750525699328293 ) ) ;
#7638 = AXIS2_PLACEMENT_3D ( 'NONE', #13905, #9973, #46480 ) ;
#7639 = VERTEX_POINT ( 'NONE', #30699 ) ;
#7640 = EDGE_LOOP ( 'NONE', ( #9583, #33327, #8863, #351 ) ) ;
#7641 = VERTEX_POINT ( 'NONE', #18873 ) ;
#7642 = CARTESIAN_POINT ( 'NONE',  ( -47.92047998570519951, -175.3837268820161057, -0.8294056854501942189 ) ) ;
#7643 = ORIENTED_EDGE ( 'NONE', *, *, #31432, .F. ) ;
#7644 = EDGE_CURVE ( 'NONE', #33465, #47404, #19151, .T. ) ;
#7645 = LINE ( 'NONE', #272, #33449 ) ;
#7646 = LINE ( 'NONE', #11316, #39476 ) ;
#7649 = VERTEX_POINT ( 'NONE', #38334 ) ;
#7648 = LINE ( 'NONE', #31556, #2280 ) ;
#7647 = LINE ( 'NONE', #19469, #38404 ) ;
#7650 = VECTOR ( 'NONE', #39252, 1000.000000000000114 ) ;
#7651 = LINE ( 'NONE', #23670, #43237 ) ;
#7652 = ORIENTED_EDGE ( 'NONE', *, *, #14279, .T. ) ;
#7653 = PLANE ( 'NONE',  #39830 ) ;
#7654 = ORIENTED_EDGE ( 'NONE', *, *, #12911, .F. ) ;
#7655 = CARTESIAN_POINT ( 'NONE',  ( -48.88225018079683082, -175.3837268820161057, 0.9151456172430223468 ) ) ;
#7656 = CARTESIAN_POINT ( 'NONE',  ( -339.1964088526558498, -102.6919536717973784, 56.27632902032055284 ) ) ;
#7658 = CARTESIAN_POINT ( 'NONE',  ( -332.3517673607765914, -66.51961791625839737, 18.79457521708899392 ) ) ;
#7657 = DIRECTION ( 'NONE',  ( 0.4566292373937140270, 0.000000000000000000, -0.8896570909947467687 ) ) ;
#7659 = ORIENTED_EDGE ( 'NONE', *, *, #19340, .T. ) ;
#7660 = ADVANCED_FACE ( 'NONE', ( #15468 ), #50963, .T. ) ;
#7661 = DIRECTION ( 'NONE',  ( -1.000000000000000000, 0.000000000000000000, 0.000000000000000000 ) ) ;
#7662 = CARTESIAN_POINT ( 'NONE',  ( 46.00000000000000000, 20.00000000000000000, 4.999999999999997335 ) ) ;
#7663 = ORIENTED_EDGE ( 'NONE', *, *, #32111, .F. ) ;
#7664 = CARTESIAN_POINT ( 'NONE',  ( -98.31070548515600649, -175.3837268820161057, -113.5465278748093283 ) ) ;
#7665 = DIRECTION ( 'NONE',  ( -1.000000000000000000, -0.000000000000000000, 0.000000000000000000 ) ) ;
#7666 = VECTOR ( 'NONE', #25148, 1000.000000000000000 ) ;
#7667 = CARTESIAN_POINT ( 'NONE',  ( 24.07160180756802248, -177.1207230881787780, 100.5610240384924481 ) ) ;
#7668 = EDGE_CURVE ( 'NONE', #33506, #13423, #50444, .T. ) ;
#7669 = EDGE_CURVE ( 'NONE', #30653, #36591, #22828, .T. ) ;
#7670 = EDGE_CURVE ( 'NONE', #21917, #37982, #47012, .T. ) ;
#7671 = ORIENTED_EDGE ( 'NONE', *, *, #33572, .F. ) ;
#7672 = EDGE_CURVE ( 'NONE', #37490, #2274, #35165, .T. ) ;
#7673 = CARTESIAN_POINT ( 'NONE',  ( -111.8989814360438828, -175.3837268820161057, -107.7168604805787027 ) ) ;
#7674 = FACE_OUTER_BOUND ( 'NONE', #141, .T. ) ;
#7675 = EDGE_CURVE ( 'NONE', #6739, #36835, #47273, .T. ) ;
#7676 = AXIS2_PLACEMENT_3D ( 'NONE', #26636, #31082, #11106 ) ;
#7677 = ORIENTED_EDGE ( 'NONE', *, *, #41308, .F. ) ;
#7678 = CARTESIAN_POINT ( 'NONE',  ( -332.3517673607765914, -154.8494888031386836, 50.05135858667791382 ) ) ;
#7679 = ORIENTED_EDGE ( 'NONE', *, *, #14775, .F. ) ;
#7680 = DIRECTION ( 'NONE',  ( -1.000000000000000000, -0.000000000000000000, -0.000000000000000000 ) ) ;
#7681 = EDGE_CURVE ( 'NONE', #30840, #3547, #43311, .T. ) ;
#7682 = LINE ( 'NONE', #2702, #3426 ) ;
#7683 = PLANE ( 'NONE',  #50430 ) ;
#7684 = DIRECTION ( 'NONE',  ( 0.000000000000000000, 0.000000000000000000, 1.000000000000000000 ) ) ;
#7685 = DIRECTION ( 'NONE',  ( 0.000000000000000000, 1.000000000000000000, -0.000000000000000000 ) ) ;
#7686 = EDGE_CURVE ( 'NONE', #45092, #41614, #42270, .T. ) ;
#7687 = AXIS2_PLACEMENT_3D ( 'NONE', #37291, #8919, #33361 ) ;
#7688 = EDGE_CURVE ( 'NONE', #31493, #33271, #16772, .T. ) ;
#7689 = CARTESIAN_POINT ( 'NONE',  ( -108.4791267515088435, -173.5000000000000284, -60.00000000000002842 ) ) ;
#7690 = AXIS2_PLACEMENT_3D ( 'NONE', #6873, #31035, #19227 ) ;
#7691 = EDGE_CURVE ( 'NONE', #47822, #40259, #35951, .T. ) ;
#7692 = DIRECTION ( 'NONE',  ( -1.000000000000000000, -0.000000000000000000, 0.000000000000000000 ) ) ;
#7693 = LINE ( 'NONE', #4018, #30576 ) ;
#7695 = ORIENTED_EDGE ( 'NONE', *, *, #2585, .T. ) ;
#7694 = FACE_OUTER_BOUND ( 'NONE', #20998, .T. ) ;
#7696 = EDGE_CURVE ( 'NONE', #11813, #50878, #27538, .T. ) ;
#7697 = ORIENTED_EDGE ( 'NONE', *, *, #20787, .T. ) ;
#7698 = CARTESIAN_POINT ( 'NONE',  ( -48.47912675150885065, -177.1207230881787780, 6.938893903907228378E-15 ) ) ;
#7699 = EDGE_CURVE ( 'NONE', #30689, #22103, #8353, .T. ) ;
#7700 = DIRECTION ( 'NONE',  ( -0.000000000000000000, 1.000000000000000000, -0.000000000000000000 ) ) ;
#7701 = EDGE_LOOP ( 'NONE', ( #43956, #43100, #44629, #42896 ) ) ;
#7702 = ORIENTED_EDGE ( 'NONE', *, *, #12861, .F. ) ;
#7703 = CARTESIAN_POINT ( 'NONE',  ( -17.07133635870350474, -193.5000000000000000, -119.9572859573364809 ) ) ;
#7704 = VERTEX_POINT ( 'NONE', #727 ) ;
#7705 = CARTESIAN_POINT ( 'NONE',  ( -171.4559849729830603, -177.1207230881787780, 22.39848972532370297 ) ) ;
#7706 = CARTESIAN_POINT ( 'NONE',  ( 24.63024857337166296, -183.6283474603465606, 101.3904297239426597 ) ) ;
#7707 = VECTOR ( 'NONE', #12463, 1000.000000000000000 ) ;
#7708 = DIRECTION ( 'NONE',  ( 0.000000000000000000, -0.9709418174260492362, 0.2393156642875685636 ) ) ;
#7709 = CARTESIAN_POINT ( 'NONE',  ( -305.0000000000000568, -101.7569374291123268, 55.92172413327813274 ) ) ;
#7710 = VECTOR ( 'NONE', #29326, 1000.000000000000114 ) ;
#7711 = ORIENTED_EDGE ( 'NONE', *, *, #39866, .F. ) ;
#7712 = ORIENTED_EDGE ( 'NONE', *, *, #23677, .F. ) ;
#7714 = ORIENTED_EDGE ( 'NONE', *, *, #9588, .T. ) ;
#7713 = CIRCLE ( 'NONE', #41282, 60.00000000000000000 ) ;
#7715 = EDGE_CURVE ( 'NONE', #8493, #18723, #3620, .T. ) ;
#7716 = DIRECTION ( 'NONE',  ( 0.000000000000000000, 0.000000000000000000, 1.000000000000000000 ) ) ;
#7717 = FACE_OUTER_BOUND ( 'NONE', #27801, .T. ) ;
#7718 = DIRECTION ( 'NONE',  ( 0.000000000000000000, 0.000000000000000000, 1.000000000000000000 ) ) ;
#7719 = DIRECTION ( 'NONE',  ( -0.000000000000000000, 1.000000000000000000, -0.000000000000000000 ) ) ;
#7720 = DIRECTION ( 'NONE',  ( 0.000000000000000000, 0.000000000000000000, -1.000000000000000000 ) ) ;
#7721 = EDGE_LOOP ( 'NONE', ( #49434, #14352, #28270, #36379 ) ) ;
#7722 = LINE ( 'NONE', #44244, #17162 ) ;
#7723 = PLANE ( 'NONE',  #16438 ) ;
#7724 = DIRECTION ( 'NONE',  ( -1.000000000000000000, -0.000000000000000000, -0.000000000000000000 ) ) ;
#7725 = VECTOR ( 'NONE', #41042, 1000.000000000000000 ) ;
#7726 = ORIENTED_EDGE ( 'NONE', *, *, #51596, .F. ) ;
#7727 = ORIENTED_EDGE ( 'NONE', *, *, #17837, .T. ) ;
#7728 = AXIS2_PLACEMENT_3D ( 'NONE', #45974, #22286, #18609 ) ;
#7729 = ORIENTED_EDGE ( 'NONE', *, *, #2352, .T. ) ;
#7730 = VECTOR ( 'NONE', #26394, 1000.000000000000114 ) ;
#7731 = DIRECTION ( 'NONE',  ( 0.000000000000000000, 0.000000000000000000, 1.000000000000000000 ) ) ;
#7732 = DIRECTION ( 'NONE',  ( 0.2059786187411021818, 0.000000000000000000, -0.9785564922995032555 ) ) ;
#7733 = ORIENTED_EDGE ( 'NONE', *, *, #7905, .F. ) ;
#7734 = PLANE ( 'NONE',  #32428 ) ;
#7735 = PLANE ( 'NONE',  #40495 ) ;
#7736 = ADVANCED_FACE ( 'NONE', ( #28042 ), #4399, .T. ) ;
#7738 = ADVANCED_FACE ( 'NONE', ( #23851 ), #48034, .T. ) ;
#7737 = CARTESIAN_POINT ( 'NONE',  ( -330.4913330509368166, -138.3439121830100191, -58.13482838284712528 ) ) ;
#7739 = VERTEX_POINT ( 'NONE', #12014 ) ;
#7740 = DIRECTION ( 'NONE',  ( 0.3482016354343928088, 0.000000000000000000, 0.9374196611341231167 ) ) ;
#7741 = VERTEX_POINT ( 'NONE', #40381 ) ;
#7742 = DIRECTION ( 'NONE',  ( 0.000000000000000000, -1.000000000000000000, 0.000000000000000000 ) ) ;
#7743 = PLANE ( 'NONE',  #12725 ) ;
#7744 = ORIENTED_EDGE ( 'NONE', *, *, #31762, .T. ) ;
#7745 = CARTESIAN_POINT ( 'NONE',  ( -336.3521761649654422, -92.15051119686104641, -50.05135858667769355 ) ) ;
#7746 = LINE ( 'NONE', #44273, #33104 ) ;
#7747 = CARTESIAN_POINT ( 'NONE',  ( -60.86541030502398542, -193.5000000000000000, -124.3848060646151623 ) ) ;
#7748 = CARTESIAN_POINT ( 'NONE',  ( -336.3521761649654422, -171.3361784870343740, 36.21739951675978375 ) ) ;
#7749 = EDGE_LOOP ( 'NONE', ( #39788, #5617, #9091, #44000 ) ) ;
#7750 = DIRECTION ( 'NONE',  ( 0.000000000000000000, -0.000000000000000000, -1.000000000000000000 ) ) ;
#7751 = EDGE_LOOP ( 'NONE', ( #26655, #25101, #16756, #872 ) ) ;
#7752 = VERTEX_POINT ( 'NONE', #51729 ) ;
#7753 = ADVANCED_FACE ( 'NONE', ( #28566 ), #15738, .F. ) ;
#7755 = ORIENTED_EDGE ( 'NONE', *, *, #25028, .T. ) ;
#7754 = DIRECTION ( 'NONE',  ( 0.000000000000000000, 0.000000000000000000, 1.000000000000000000 ) ) ;
#7756 = VERTEX_POINT ( 'NONE', #8089 ) ;
#7757 = CARTESIAN_POINT ( 'NONE',  ( -330.4913330509368166, -64.86990808808717190, -6.615309698015095385 ) ) ;
#7758 = AXIS2_PLACEMENT_3D ( 'NONE', #28101, #8153, #28372 ) ;
#7759 = VECTOR ( 'NONE', #40814, 1000.000000000000000 ) ;
#7760 = ADVANCED_FACE ( 'NONE', ( #20425 ), #12278, .T. ) ;
#7761 = CARTESIAN_POINT ( 'NONE',  ( -339.1964088526558498, -75.22798428563991990, -33.92731199008514409 ) ) ;
#7762 = VECTOR ( 'NONE', #13037, 1000.000000000000000 ) ;
#7763 = CIRCLE ( 'NONE', #37131, 60.00000000000000000 ) ;
#7764 = VERTEX_POINT ( 'NONE', #40142 ) ;
#7765 = PLANE ( 'NONE',  #14213 ) ;
#7766 = CARTESIAN_POINT ( 'NONE',  ( -145.6517069852672535, -175.3837268820161057, 78.62880929222946236 ) ) ;
#7767 = ORIENTED_EDGE ( 'NONE', *, *, #10184, .F. ) ;
#7768 = CARTESIAN_POINT ( 'NONE',  ( -48.47912675150885065, -173.5000000000000284, 6.938893903907228378E-15 ) ) ;
#7769 = DIRECTION ( 'NONE',  ( 0.000000000000000000, -1.000000000000000000, 0.000000000000000000 ) ) ;
#7770 = CARTESIAN_POINT ( 'NONE',  ( -330.4913330509368166, -66.33409060400670398, -14.60509510167892522 ) ) ;
#7771 = FACE_OUTER_BOUND ( 'NONE', #190, .T. ) ;
#7772 = ORIENTED_EDGE ( 'NONE', *, *, #39805, .F. ) ;
#7773 = ORIENTED_EDGE ( 'NONE', *, *, #50142, .F. ) ;
#7774 = EDGE_LOOP ( 'NONE', ( #9567, #13765, #29041, #7306 ) ) ;
#7775 = CARTESIAN_POINT ( 'NONE',  ( -49.47868758801764955, -183.6283474603465606, 0.02963332782255607284 ) ) ;
#7776 = PLANE ( 'NONE',  #18452 ) ;
#7777 = CARTESIAN_POINT ( 'NONE',  ( 12.12533326292403935, -177.1207230881787780, 109.3256576763158989 ) ) ;
#7778 = DIRECTION ( 'NONE',  ( -0.000000000000000000, 1.000000000000000000, 0.000000000000000000 ) ) ;
#7779 = CARTESIAN_POINT ( 'NONE',  ( -49.44376233341721161, -189.7472609257535510, 0.2635871660690650709 ) ) ;
#7780 = VECTOR ( 'NONE', #15705, 1000.000000000000114 ) ;
#7781 = ORIENTED_EDGE ( 'NONE', *, *, #1926, .F. ) ;
#7782 = AXIS2_PLACEMENT_3D ( 'NONE', #21547, #9451, #1567 ) ;
#7783 = LINE ( 'NONE', #44041, #26567 ) ;
#7784 = VERTEX_POINT ( 'NONE', #4159 ) ;
#7786 = ORIENTED_EDGE ( 'NONE', *, *, #39934, .F. ) ;
#7785 = DIRECTION ( 'NONE',  ( 0.000000000000000000, -0.4647231720437755564, -0.8854560256532062468 ) ) ;
#7787 = VERTEX_POINT ( 'NONE', #32249 ) ;
#7788 = DIRECTION ( 'NONE',  ( -0.000000000000000000, -0.4647231720437724478, -0.8854560256532078011 ) ) ;
#7789 = CARTESIAN_POINT ( 'NONE',  ( -171.5592422664403216, -177.1207230881787780, -21.82395850507255730 ) ) ;
#7790 = CARTESIAN_POINT ( 'NONE',  ( 0.000000000000000000, -84.37576316379318087, -44.16213414209506283 ) ) ;
#7791 = EDGE_CURVE ( 'NONE', #37919, #5531, #445, .T. ) ;
#7792 = DIRECTION ( 'NONE',  ( 0.7948544414133481562, 0.000000000000000000, 0.6068001458186002006 ) ) ;
#7793 = EDGE_LOOP ( 'NONE', ( #12139, #28740, #44840, #9937 ) ) ;
#7794 = DIRECTION ( 'NONE',  ( -0.2920567706369628924, 0.000000000000000000, -0.9564009842765264224 ) ) ;
#7795 = AXIS2_PLACEMENT_3D ( 'NONE', #29986, #17658, #26554 ) ;
#7796 = ORIENTED_EDGE ( 'NONE', *, *, #27978, .T. ) ;
#7797 = VECTOR ( 'NONE', #33033, 1000.000000000000000 ) ;
#7798 = VERTEX_POINT ( 'NONE', #32521 ) ;
#7799 = CARTESIAN_POINT ( 'NONE',  ( -336.3521761649654422, -93.75055682584159911, 51.01861988938794923 ) ) ;
#7800 = CIRCLE ( 'NONE', #252, 125.0000000000000000 ) ;
#7801 = CARTESIAN_POINT ( 'NONE',  ( -171.9838957966129556, -175.3837268820161057, 19.27620354518722579 ) ) ;
#7802 = PLANE ( 'NONE',  #26520 ) ;
#7803 = DIRECTION ( 'NONE',  ( -0.000000000000000000, 1.000000000000000000, 0.000000000000000000 ) ) ;
#7804 = FACE_OUTER_BOUND ( 'NONE', #35519, .T. ) ;
#7805 = DIRECTION ( 'NONE',  ( -0.000000000000000000, 0.9350162426854146114, -0.3546048870425363986 ) ) ;
#7806 = ORIENTED_EDGE ( 'NONE', *, *, #26435, .F. ) ;
#7807 = DIRECTION ( 'NONE',  ( 0.000000000000000000, 0.000000000000000000, -1.000000000000000000 ) ) ;
#7808 = CARTESIAN_POINT ( 'NONE',  ( -330.4913330509368166, -123.5000000000000284, 0.000000000000000000 ) ) ;
#7809 = FACE_BOUND ( 'NONE', #36195, .T. ) ;
#7810 = VERTEX_POINT ( 'NONE', #48570 ) ;
#7811 = ADVANCED_FACE ( 'NONE', ( #31747 ), #19917, .T. ) ;
#7812 = DIRECTION ( 'NONE',  ( 0.000000000000000000, -0.1205366802553268363, -0.9927088740980534176 ) ) ;
#7813 = AXIS2_PLACEMENT_3D ( 'NONE', #35332, #11154, #31910 ) ;
#7814 = CARTESIAN_POINT ( 'NONE',  ( -339.1964088526558498, -167.3305728129742249, 39.49849221029288060 ) ) ;
#7815 = ORIENTED_EDGE ( 'NONE', *, *, #28313, .T. ) ;
#7816 = DIRECTION ( 'NONE',  ( 0.000000000000000000, -1.387778780781445182E-16, 1.000000000000000000 ) ) ;
#7817 = ORIENTED_EDGE ( 'NONE', *, *, #23921, .T. ) ;
#7818 = VECTOR ( 'NONE', #11116, 1000.000000000000000 ) ;
#7819 = EDGE_CURVE ( 'NONE', #13356, #5724, #36189, .T. ) ;
#7820 = FACE_OUTER_BOUND ( 'NONE', #2838, .T. ) ;
#7821 = FACE_BOUND ( 'NONE', #51422, .T. ) ;
#7822 = CARTESIAN_POINT ( 'NONE',  ( -118.4510020108455137, -175.3837268820161057, 103.5805805771131674 ) ) ;
#7824 = AXIS2_PLACEMENT_3D ( 'NONE', #16735, #32741, #49495 ) ;
#7823 = DIRECTION ( 'NONE',  ( 0.000000000000000000, 1.000000000000000000, 0.000000000000000000 ) ) ;
#7825 = ORIENTED_EDGE ( 'NONE', *, *, #25536, .T. ) ;
#7826 = ORIENTED_EDGE ( 'NONE', *, *, #20880, .F. ) ;
#7827 = CARTESIAN_POINT ( 'NONE',  ( -339.1964088526558498, -89.57268800991437274, 48.27201571435973904 ) ) ;
#7828 = AXIS2_PLACEMENT_3D ( 'NONE', #8055, #4124, #20138 ) ;
#7829 = ORIENTED_EDGE ( 'NONE', *, *, #16681, .T. ) ;
#7830 = DIRECTION ( 'NONE',  ( 0.000000000000000000, 0.000000000000000000, 1.000000000000000000 ) ) ;
#7831 = CYLINDRICAL_SURFACE ( 'NONE', #35581, 124.9999999999999858 ) ;
#7832 = EDGE_CURVE ( 'NONE', #43249, #29810, #4664, .T. ) ;
#7833 = VECTOR ( 'NONE', #13841, 1000.000000000000114 ) ;
#7834 = ADVANCED_FACE ( 'NONE', ( #43574 ), #7575, .F. ) ;
#7835 = DIRECTION ( 'NONE',  ( -0.000000000000000000, 0.5680647467311656929, 0.8229838658936495799 ) ) ;
#7836 = CARTESIAN_POINT ( 'NONE',  ( -238.7407812814481076, -193.5000000000000000, 41.45482488023466772 ) ) ;
#7837 = EDGE_LOOP ( 'NONE', ( #44372, #24003, #15933, #3287 ) ) ;
#7840 = ORIENTED_EDGE ( 'NONE', *, *, #42644, .T. ) ;
#7839 = CARTESIAN_POINT ( 'NONE',  ( -332.3517673607765914, -79.68838513426354098, -40.99441916720346768 ) ) ;
#7838 = DIRECTION ( 'NONE',  ( -0.000000000000000000, -0.7485107481711046340, -0.6631226582407911962 ) ) ;
#7841 = ORIENTED_EDGE ( 'NONE', *, *, #6568, .F. ) ;
#7842 = CARTESIAN_POINT ( 'NONE',  ( 74.49773146996547268, -193.5000000000000000, -22.39848972532282190 ) ) ;
#7843 = ORIENTED_EDGE ( 'NONE', *, *, #37059, .F. ) ;
#7844 = DIRECTION ( 'NONE',  ( -1.000000000000000000, 0.000000000000000000, -0.000000000000000000 ) ) ;
#7845 = AXIS2_PLACEMENT_3D ( 'NONE', #9437, #24951, #49127 ) ;
#7846 = ORIENTED_EDGE ( 'NONE', *, *, #51029, .F. ) ;
#7847 = EDGE_CURVE ( 'NONE', #38856, #7810, #4939, .T. ) ;
#7848 = CARTESIAN_POINT ( 'NONE',  ( -336.3521761649654422, -77.59233547837267508, 37.15394033962009246 ) ) ;
#7849 = VERTEX_POINT ( 'NONE', #45922 ) ;
#7851 = FACE_OUTER_BOUND ( 'NONE', #20598, .T. ) ;
#7850 = FACE_OUTER_BOUND ( 'NONE', #46171, .T. ) ;
#7852 = EDGE_CURVE ( 'NONE', #18828, #30731, #13334, .T. ) ;
#7853 = VECTOR ( 'NONE', #9958, 1000.000000000000000 ) ;
#7854 = DIRECTION ( 'NONE',  ( 0.000000000000000000, 1.000000000000000000, 0.000000000000000000 ) ) ;
#7855 = EDGE_LOOP ( 'NONE', ( #14842, #46364, #9836, #22020 ) ) ;
#7856 = CYLINDRICAL_SURFACE ( 'NONE', #23673, 125.0000000000000000 ) ;
#7857 = EDGE_CURVE ( 'NONE', #22679, #47261, #37168, .T. ) ;
#7858 = FACE_OUTER_BOUND ( 'NONE', #27571, .T. ) ;
#7859 = DIRECTION ( 'NONE',  ( -0.000000000000000000, 1.000000000000000000, -0.000000000000000000 ) ) ;
#7860 = DIRECTION ( 'NONE',  ( -1.000000000000000000, -0.000000000000000000, 0.000000000000000000 ) ) ;
#7861 = CARTESIAN_POINT ( 'NONE',  ( -330.4913330509368166, -78.92247586332024412, -40.16023333900999859 ) ) ;
#7862 = DIRECTION ( 'NONE',  ( 0.000000000000000000, -0.3546048870425267951, 0.9350162426854181641 ) ) ;
#7863 = ORIENTED_EDGE ( 'NONE', *, *, #17738, .T. ) ;
#7864 =( NAMED_UNIT ( * ) SI_UNIT ( $, .STERADIAN. ) SOLID_ANGLE_UNIT ( ) );
#7865 = AXIS2_PLACEMENT_3D ( 'NONE', #40931, #5470, #17294 ) ;
#7866 = PLANE ( 'NONE',  #50668 ) ;
#7867 = DIRECTION ( 'NONE',  ( 0.8294056854501971054, 0.000000000000000000, 0.5586467658036594619 ) ) ;
#7868 = LINE ( 'NONE', #40189, #48091 ) ;
#7869 = ORIENTED_EDGE ( 'NONE', *, *, #24146, .T. ) ;
#7870 = APPLICATION_CONTEXT ( 'automotive_design' ) ;
#7871 = DIRECTION ( 'NONE',  ( 0.000000000000000000, -0.1205366802553303196, -0.9927088740980530845 ) ) ;
#7872 = EDGE_CURVE ( 'NONE', #43059, #34819, #12795, .T. ) ;
#7873 = DIRECTION ( 'NONE',  ( -0.6068001458185834363, 0.000000000000000000, -0.7948544414133608127 ) ) ;
#7874 = DIRECTION ( 'NONE',  ( 0.000000000000000000, -0.000000000000000000, 1.000000000000000000 ) ) ;
#7875 = EDGE_LOOP ( 'NONE', ( #36761, #339, #6733, #36169 ) ) ;
#7876 = EDGE_LOOP ( 'NONE', ( #28812, #8689, #30986, #23421 ) ) ;
#7877 = ORIENTED_EDGE ( 'NONE', *, *, #31260, .F. ) ;
#7878 = LINE ( 'NONE', #23905, #18692 ) ;
#7879 = CARTESIAN_POINT ( 'NONE',  ( -128.2395503755045638, -193.5000000000000000, -96.24590808611419845 ) ) ;
#7880 = CARTESIAN_POINT ( 'NONE',  ( -123.6678354051270361, -175.3837268820161057, 99.85818990449065780 ) ) ;
#7881 = LINE ( 'NONE', #51796, #10279 ) ;
#7882 = AXIS2_PLACEMENT_3D ( 'NONE', #40897, #5179, #4920 ) ;
#7883 = EDGE_LOOP ( 'NONE', ( #30706, #18480, #34853, #9386 ) ) ;
#7884 = VECTOR ( 'NONE', #31790, 1000.000000000000114 ) ;
#7885 = CARTESIAN_POINT ( 'NONE',  ( 4.238395535310755413, 55.36142218126918380, -17.76894564376730656 ) ) ;
#7886 = AXIS2_PLACEMENT_3D ( 'NONE', #33543, #17000, #49322 ) ;
#7887 = VERTEX_POINT ( 'NONE', #28818 ) ;
#7888 = VERTEX_POINT ( 'NONE', #37240 ) ;
#7889 = ORIENTED_EDGE ( 'NONE', *, *, #24198, .F. ) ;
#7890 = DIRECTION ( 'NONE',  ( 0.000000000000000000, -1.000000000000000000, 0.000000000000000000 ) ) ;
#7891 = EDGE_CURVE ( 'NONE', #50412, #4631, #33810, .T. ) ;
#7892 = EDGE_CURVE ( 'NONE', #38978, #177, #48826, .T. ) ;
#7894 = ORIENTED_EDGE ( 'NONE', *, *, #7453, .T. ) ;
#7893 = VECTOR ( 'NONE', #9862, 1000.000000000000000 ) ;
#7895 = CARTESIAN_POINT ( 'NONE',  ( 52.59568867645217694, -175.3837268820161057, -73.54509967498590584 ) ) ;
#7896 = DIRECTION ( 'NONE',  ( 1.000000000000000000, -0.000000000000000000, 0.000000000000000000 ) ) ;
#7899 = VERTEX_POINT ( 'NONE', #45656 ) ;
#7898 = DIRECTION ( 'NONE',  ( -0.5451229641719399499, -0.8383561021024406035, 6.675830932148835542E-17 ) ) ;
#7897 = DIRECTION ( 'NONE',  ( 5.399917434947259359E-17, 1.000000000000000000, -0.000000000000000000 ) ) ;
#7900 = CARTESIAN_POINT ( 'NONE',  ( -167.8725343822893308, -189.7472609257535510, 33.48461921608600278 ) ) ;
#7901 = VERTEX_POINT ( 'NONE', #45400 ) ;
#7902 = DIRECTION ( 'NONE',  ( 0.000000000000000000, 0.6631226582407964143, 0.7485107481710999711 ) ) ;
#7903 = ORIENTED_EDGE ( 'NONE', *, *, #32107, .F. ) ;
#7904 = FACE_OUTER_BOUND ( 'NONE', #31705, .T. ) ;
#7905 = EDGE_CURVE ( 'NONE', #6134, #46591, #9391, .T. ) ;
#7906 = CARTESIAN_POINT ( 'NONE',  ( -280.0000000000000000, -153.5000000000000284, 60.00000000000002132 ) ) ;
#7908 = DIRECTION ( 'NONE',  ( -0.000000000000000000, 1.000000000000000000, -0.000000000000000000 ) ) ;
#7907 = CARTESIAN_POINT ( 'NONE',  ( -5.113431607746556473, -175.3837268820161057, 117.2365833888819537 ) ) ;
#7909 = ADVANCED_FACE ( 'NONE', ( #17547 ), #49597, .T. ) ;
#7910 = DIRECTION ( 'NONE',  ( -0.000000000000000000, 1.000000000000000000, -0.000000000000000000 ) ) ;
#7911 = FACE_OUTER_BOUND ( 'NONE', #11583, .T. ) ;
#7912 = EDGE_CURVE ( 'NONE', #34872, #5675, #44867, .T. ) ;
#7913 = EDGE_LOOP ( 'NONE', ( #14974, #46672, #40570, #40143 ) ) ;
#7914 =( NAMED_UNIT ( * ) SI_UNIT ( $, .STERADIAN. ) SOLID_ANGLE_UNIT ( ) );
#7915 = DIRECTION ( 'NONE',  ( 0.000000000000000000, -1.000000000000000000, 0.000000000000000000 ) ) ;
#7916 = AXIS2_PLACEMENT_3D ( 'NONE', #34165, #49941, #2091 ) ;
#7917 = DIRECTION ( 'NONE',  ( 0.000000000000000000, 0.000000000000000000, 1.000000000000000000 ) ) ;
#7918 = EDGE_CURVE ( 'NONE', #4861, #47386, #9911, .T. ) ;
#7919 = AXIS2_PLACEMENT_3D ( 'NONE', #47573, #11555, #24172 ) ;
#7920 = ORIENTED_EDGE ( 'NONE', *, *, #42864, .F. ) ;
#7921 = CARTESIAN_POINT ( 'NONE',  ( -48.47912675150885065, -183.6283474603465606, 6.938893903907228378E-15 ) ) ;
#7923 = VECTOR ( 'NONE', #26628, 1000.000000000000000 ) ;
#7922 = LINE ( 'NONE', #40237, #9697 ) ;
#7924 = ORIENTED_EDGE ( 'NONE', *, *, #5144, .T. ) ;
#7925 = CARTESIAN_POINT ( 'NONE',  ( -112.1919339979530150, -193.5000000000000000, 107.5438431188761683 ) ) ;
#7926 = ORIENTED_EDGE ( 'NONE', *, *, #5015, .T. ) ;
#7927 = EDGE_CURVE ( 'NONE', #19399, #34600, #8612, .T. ) ;
#7928 = CARTESIAN_POINT ( 'NONE',  ( 62.86098202833237281, -177.1207230881787780, 56.81883646197908178 ) ) ;
#7929 = DIRECTION ( 'NONE',  ( 0.000000000000000000, 0.000000000000000000, 1.000000000000000000 ) ) ;
#7930 = DIRECTION ( 'NONE',  ( 0.000000000000000000, -0.5000000000000054401, 0.8660254037844354880 ) ) ;
#7931 = CYLINDRICAL_SURFACE ( 'NONE', #8788, 20.00000000000000000 ) ;
#7932 = DIRECTION ( 'NONE',  ( -0.000000000000000000, 0.9709418174260519008, -0.2393156642875582940 ) ) ;
#7933 = VECTOR ( 'NONE', #5929, 1000.000000000000000 ) ;
#7934 = DIRECTION ( 'NONE',  ( 0.000000000000000000, 0.000000000000000000, 1.000000000000000000 ) ) ;
#7935 = CARTESIAN_POINT ( 'NONE',  ( -173.3968853974275817, -193.5000000000000000, 4.533605064404221174 ) ) ;
#7936 = DIRECTION ( 'NONE',  ( -0.4106364553079954738, -0.8746197071393962963, -0.2577170336929270333 ) ) ;
#7938 = ORIENTED_EDGE ( 'NONE', *, *, #22212, .T. ) ;
#7937 = LINE ( 'NONE', #16359, #34570 ) ;
#7939 = EDGE_LOOP ( 'NONE', ( #47860, #40135, #36916, #37177 ) ) ;
#7940 = LINE ( 'NONE', #48167, #38346 ) ;
#7941 = ADVANCED_FACE ( 'NONE', ( #25415 ), #9136, .F. ) ;
#7942 = CARTESIAN_POINT ( 'NONE',  ( -332.3517673607765914, -67.99860710409808462, -22.79463504017392950 ) ) ;
#7943 = EDGE_LOOP ( 'NONE', ( #45610, #39335, #1304, #15720 ) ) ;
#7944 = ORIENTED_EDGE ( 'NONE', *, *, #7635, .T. ) ;
#7945 = VECTOR ( 'NONE', #44781, 1000.000000000000000 ) ;
#7946 = VERTEX_POINT ( 'NONE', #13582 ) ;
#7947 = DIRECTION ( 'NONE',  ( -1.000000000000000000, -0.000000000000000000, 0.000000000000000000 ) ) ;
#7948 = CARTESIAN_POINT ( 'NONE',  ( -151.4272465800706016, -193.5000000000000000, 70.89911581792887318 ) ) ;
#7949 = AXIS2_PLACEMENT_3D ( 'NONE', #23873, #28336, #35439 ) ;
#7950 = VECTOR ( 'NONE', #21910, 1000.000000000000000 ) ;
#7951 = EDGE_CURVE ( 'NONE', #44345, #13008, #41951, .T. ) ;
#7952 = EDGE_CURVE ( 'NONE', #3318, #6819, #37991, .T. ) ;
#7953 = EDGE_CURVE ( 'NONE', #49860, #44109, #15346, .T. ) ;
#7954 = CARTESIAN_POINT ( 'NONE',  ( -33.64434644548592246, -193.5000000000000000, -123.1094209424468033 ) ) ;
#7955 = DIRECTION ( 'NONE',  ( -0.000000000000000000, 0.6631226582407937498, -0.7485107481711024136 ) ) ;
#7956 = ORIENTED_EDGE ( 'NONE', *, *, #32233, .T. ) ;
#7957 = ORIENTED_EDGE ( 'NONE', *, *, #8033, .T. ) ;
#7958 = VECTOR ( 'NONE', #51574, 1000.000000000000000 ) ;
#7959 = EDGE_CURVE ( 'NONE', #13211, #3068, #33562, .T. ) ;
#7960 = ORIENTED_EDGE ( 'NONE', *, *, #22546, .T. ) ;
#7961 = LINE ( 'NONE', #27682, #47641 ) ;
#7962 = FACE_OUTER_BOUND ( 'NONE', #51343, .T. ) ;
#7963 = DIRECTION ( 'NONE',  ( -0.000000000000000000, -0.3546048870425300148, 0.9350162426854169428 ) ) ;
#7964 = EDGE_CURVE ( 'NONE', #36635, #34754, #35469, .T. ) ;
#7965 = CIRCLE ( 'NONE', #33147, 125.0000000000000000 ) ;
#7966 = CARTESIAN_POINT ( 'NONE',  ( 71.09073365861578964, -193.5000000000000000, 32.84887689123991095 ) ) ;
#7967 = VECTOR ( 'NONE', #8022, 1000.000000000000114 ) ;
#7968 = DIRECTION ( 'NONE',  ( 0.000000000000000000, -1.000000000000000000, 0.000000000000000000 ) ) ;
#7969 = ORIENTED_EDGE ( 'NONE', *, *, #28044, .F. ) ;
#7970 = CARTESIAN_POINT ( 'NONE',  ( -69.77312546433407192, -189.7472609257535510, 123.1729094355500109 ) ) ;
#7971 = DIRECTION ( 'NONE',  ( 0.000000000000000000, 0.000000000000000000, -1.000000000000000000 ) ) ;
#7972 = EDGE_CURVE ( 'NONE', #44682, #8048, #38005, .T. ) ;
#7973 = AXIS2_PLACEMENT_3D ( 'NONE', #1656, #30529, #6640 ) ;
#7974 = LINE ( 'NONE', #51614, #21460 ) ;
#7975 = PLANE ( 'NONE',  #2257 ) ;
#7976 = EDGE_CURVE ( 'NONE', #43746, #18062, #2281, .T. ) ;
#7977 = VECTOR ( 'NONE', #15752, 1000.000000000000000 ) ;
#7978 = ORIENTED_EDGE ( 'NONE', *, *, #47786, .T. ) ;
#7979 = ORIENTED_EDGE ( 'NONE', *, *, #21, .T. ) ;
#7980 = VERTEX_POINT ( 'NONE', #30131 ) ;
#7981 = CARTESIAN_POINT ( 'NONE',  ( 54.46899307705341187, -183.6283474603465606, -70.89911581792813422 ) ) ;
#7982 = EDGE_CURVE ( 'NONE', #41636, #11274, #51473, .T. ) ;
#7983 = CARTESIAN_POINT ( 'NONE',  ( -47.92047998570520662, -193.5000000000000000, 0.8294056854502119824 ) ) ;
#7984 = ORIENTED_EDGE ( 'NONE', *, *, #11823, .F. ) ;
#7985 = DIRECTION ( 'NONE',  ( 0.000000000000000000, 0.9927088740980530845, -0.1205366802553303057 ) ) ;
#7986 = EDGE_CURVE ( 'NONE', #49622, #18571, #1951, .T. ) ;
#7987 = FACE_OUTER_BOUND ( 'NONE', #34257, .T. ) ;
#7988 = CARTESIAN_POINT ( 'NONE',  ( -147.0463339291295881, -193.5000000000000000, 76.87330921200150158 ) ) ;
#7989 = VERTEX_POINT ( 'NONE', #46175 ) ;
#7990 = DIRECTION ( 'NONE',  ( -0.000000000000000000, 1.000000000000000000, -0.000000000000000000 ) ) ;
#7991 = ADVANCED_FACE ( 'NONE', ( #10153 ), #2534, .T. ) ;
#7992 = ORIENTED_EDGE ( 'NONE', *, *, #38355, .F. ) ;
#7993 = CARTESIAN_POINT ( 'NONE',  ( -56.71246971489870958, -175.3837268820161057, -124.7285535218267682 ) ) ;
#7994 = ORIENTED_EDGE ( 'NONE', *, *, #39488, .T. ) ;
#7995 = PLANE ( 'NONE',  #1096 ) ;
#7996 = AXIS2_PLACEMENT_3D ( 'NONE', #6078, #22872, #30750 ) ;
#7997 = CARTESIAN_POINT ( 'NONE',  ( -48.30223647638627682, -189.7472609257535510, -0.9842305779475897243 ) ) ;
#7998 = ORIENTED_EDGE ( 'NONE', *, *, #3766, .F. ) ;
#7999 = AXIS2_PLACEMENT_3D ( 'NONE', #23504, #49876, #3524 ) ;
#8000 = VECTOR ( 'NONE', #32498, 1000.000000000000000 ) ;
#8001 = DIRECTION ( 'NONE',  ( -1.000000000000000000, 0.000000000000000000, 0.000000000000000000 ) ) ;
#8002 = PLANE ( 'NONE',  #19661 ) ;
#8003 = CARTESIAN_POINT ( 'NONE',  ( -48.47912675150885065, -189.7472609257535510, 6.938893903907228378E-15 ) ) ;
#8004 = DIRECTION ( 'NONE',  ( 0.000000000000000000, 1.000000000000000000, 0.000000000000000000 ) ) ;
#8005 = EDGE_CURVE ( 'NONE', #36071, #20840, #42468, .T. ) ;
#8006 = AXIS2_PLACEMENT_3D ( 'NONE', #48813, #51989, #48286 ) ;
#8007 = ORIENTED_EDGE ( 'NONE', *, *, #1732, .T. ) ;
#8008 = CARTESIAN_POINT ( 'NONE',  ( 0.000000000000000000, -43.50000000000000000, 30.00000000000000355 ) ) ;
#8009 = ORIENTED_EDGE ( 'NONE', *, *, #20558, .T. ) ;
#8010 = ORIENTED_EDGE ( 'NONE', *, *, #3104, .F. ) ;
#8011 = AXIS2_PLACEMENT_3D ( 'NONE', #51183, #34854, #3067 ) ;
#8012 = FACE_OUTER_BOUND ( 'NONE', #36713, .T. ) ;
#8014 = ORIENTED_EDGE ( 'NONE', *, *, #8574, .F. ) ;
#8013 = CARTESIAN_POINT ( 'NONE',  ( 37.77106160267053525, -193.5000000000000000, 89.08931047202635511 ) ) ;
#8015 = VECTOR ( 'NONE', #4480, 1000.000000000000114 ) ;
#8016 = ORIENTED_EDGE ( 'NONE', *, *, #15519, .T. ) ;
#8017 = DIRECTION ( 'NONE',  ( 1.000000000000000000, 0.000000000000000000, -0.000000000000000000 ) ) ;
#8018 = CIRCLE ( 'NONE', #37387, 125.0000000000000000 ) ;
#8019 = CIRCLE ( 'NONE', #37391, 125.0000000000000000 ) ;
#8020 = DIRECTION ( 'NONE',  ( -0.9266896074318291543, 0.000000000000000000, -0.3758275821142488260 ) ) ;
#8021 = ORIENTED_EDGE ( 'NONE', *, *, #18289, .T. ) ;
#8022 = DIRECTION ( 'NONE',  ( -0.000000000000000000, -0.9350162426854121689, 0.3546048870425426158 ) ) ;
#8023 = DIRECTION ( 'NONE',  ( 0.000000000000000000, 0.000000000000000000, -1.000000000000000000 ) ) ;
#8024 = ORIENTED_EDGE ( 'NONE', *, *, #20853, .F. ) ;
#8025 = CARTESIAN_POINT ( 'NONE',  ( 66.03142248012326831, -183.6283474603465606, 50.12318939044041599 ) ) ;
#8026 = DIRECTION ( 'NONE',  ( -0.4566292373937140270, 0.000000000000000000, 0.8896570909947467687 ) ) ;
#8027 = EDGE_CURVE ( 'NONE', #10828, #25168, #51165, .T. ) ;
#8028 = ADVANCED_FACE ( 'NONE', ( #6493 ), #46426, .T. ) ;
#8029 = DIRECTION ( 'NONE',  ( 0.000000000000000000, 0.000000000000000000, -1.000000000000000000 ) ) ;
#8030 = DIRECTION ( 'NONE',  ( 0.000000000000000000, 0.000000000000000000, 1.000000000000000000 ) ) ;
#8031 = ORIENTED_EDGE ( 'NONE', *, *, #26186, .T. ) ;
#8032 = ORIENTED_EDGE ( 'NONE', *, *, #20852, .F. ) ;
#8033 = EDGE_CURVE ( 'NONE', #45363, #24508, #50122, .T. ) ;
#8034 = ORIENTED_EDGE ( 'NONE', *, *, #32087, .F. ) ;
#8035 = EDGE_CURVE ( 'NONE', #2659, #10865, #28787, .T. ) ;
#8036 = LINE ( 'NONE', #36147, #20731 ) ;
#8037 = DIRECTION ( 'NONE',  ( -0.000000000000000000, -3.491481338843133355E-15, -1.000000000000000000 ) ) ;
#8038 = CIRCLE ( 'NONE', #30684, 125.0000000000000000 ) ;
#8039 = CARTESIAN_POINT ( 'NONE',  ( 54.46899307705341187, -193.5000000000000000, -70.89911581792813422 ) ) ;
#8040 = CIRCLE ( 'NONE', #50819, 125.0000000000000000 ) ;
#8041 = FACE_BOUND ( 'NONE', #11695, .T. ) ;
#8042 = LINE ( 'NONE', #31951, #38956 ) ;
#8043 = ORIENTED_EDGE ( 'NONE', *, *, #4735, .F. ) ;
#8044 = AXIS2_PLACEMENT_3D ( 'NONE', #44466, #40502, #28934 ) ;
#8045 = LINE ( 'NONE', #3328, #37530 ) ;
#8046 = ORIENTED_EDGE ( 'NONE', *, *, #35315, .T. ) ;
#8048 = VERTEX_POINT ( 'NONE', #34576 ) ;
#8047 = CARTESIAN_POINT ( 'NONE',  ( -17.07133635870349408, -177.1207230881787780, -119.9572859573364809 ) ) ;
#8049 = ORIENTED_EDGE ( 'NONE', *, *, #42031, .F. ) ;
#8050 = EDGE_CURVE ( 'NONE', #29948, #19322, #18317, .T. ) ;
#8051 = FACE_OUTER_BOUND ( 'NONE', #18446, .T. ) ;
#8052 = CIRCLE ( 'NONE', #499, 60.00000000000000000 ) ;
#8053 = LINE ( 'NONE', #23323, #5672 ) ;
#8054 = CIRCLE ( 'NONE', #3858, 125.0000000000000000 ) ;
#8055 = CARTESIAN_POINT ( 'NONE',  ( -330.4913330509368166, -123.5000000000000284, 0.000000000000000000 ) ) ;
#8056 = CARTESIAN_POINT ( 'NONE',  ( -37.14819544345410662, -177.1207230881787780, 123.4817304940907263 ) ) ;
#8057 = ORIENTED_EDGE ( 'NONE', *, *, #41299, .T. ) ;
#8058 = LINE ( 'NONE', #36417, #31744 ) ;
#8059 = VECTOR ( 'NONE', #8624, 1000.000000000000000 ) ;
#8060 = VERTEX_POINT ( 'NONE', #50375 ) ;
#8061 = EDGE_CURVE ( 'NONE', #51893, #21483, #26434, .T. ) ;
#8062 = CIRCLE ( 'NONE', #38284, 60.00000000000000000 ) ;
#8063 = EDGE_LOOP ( 'NONE', ( #11475, #25173, #11343, #44366 ) ) ;
#8064 = DIRECTION ( 'NONE',  ( 0.000000000000000000, 0.000000000000000000, -1.000000000000000000 ) ) ;
#8065 = CYLINDRICAL_SURFACE ( 'NONE', #42930, 125.0000000000000000 ) ;
#8066 = DIRECTION ( 'NONE',  ( 0.000000000000000000, 1.000000000000000000, 0.000000000000000000 ) ) ;
#8067 = DIRECTION ( 'NONE',  ( 0.000000000000000000, 5.504855830433067636E-14, -1.000000000000000000 ) ) ;
#8068 = DIRECTION ( 'NONE',  ( -0.3758275821142488260, 0.000000000000000000, 0.9266896074318291543 ) ) ;
#8069 = FACE_OUTER_BOUND ( 'NONE', #26209, .T. ) ;
#8070 = ORIENTED_EDGE ( 'NONE', *, *, #13172, .F. ) ;
#8071 = CARTESIAN_POINT ( 'NONE',  ( -105.7090724259148118, -193.5000000000000000, 111.1293539894142839 ) ) ;
#8072 = CARTESIAN_POINT ( 'NONE',  ( -91.22542124915045747, -193.5000000000000000, 117.4638425504669783 ) ) ;
#8073 = FACE_BOUND ( 'NONE', #16567, .T. ) ;
#8074 = ORIENTED_EDGE ( 'NONE', *, *, #44106, .T. ) ;
#8075 = AXIS2_PLACEMENT_3D ( 'NONE', #46998, #7046, #2336 ) ;
#8076 = AXIS2_PLACEMENT_3D ( 'NONE', #28537, #8066, #44843 ) ;
#8077 = CARTESIAN_POINT ( 'NONE',  ( -165.7578939544008847, -193.5000000000000000, -43.25148278810626579 ) ) ;
#8078 = VECTOR ( 'NONE', #29195, 1000.000000000000114 ) ;
#8079 = AXIS2_PLACEMENT_3D ( 'NONE', #18989, #26610, #35013 ) ;
#8080 = DIRECTION ( 'NONE',  ( 0.000000000000000000, 0.000000000000000000, 1.000000000000000000 ) ) ;
#8081 = ORIENTED_EDGE ( 'NONE', *, *, #44416, .T. ) ;
#8082 = PLANE ( 'NONE',  #32147 ) ;
#8083 = EDGE_CURVE ( 'NONE', #28733, #15796, #30631, .T. ) ;
#8084 = ORIENTED_EDGE ( 'NONE', *, *, #46852, .F. ) ;
#8085 = PLANE ( 'NONE',  #15922 ) ;
#8086 = VECTOR ( 'NONE', #51622, 1000.000000000000000 ) ;
#8087 = FACE_BOUND ( 'NONE', #16262, .T. ) ;
#8088 = MECHANICAL_DESIGN_GEOMETRIC_PRESENTATION_REPRESENTATION (  '', ( #1372 ), #529 ) ;
#8089 = CARTESIAN_POINT ( 'NONE',  ( -154.5708152632604993, -177.1207230881787780, 64.19309449102807719 ) ) ;
#8090 = CIRCLE ( 'NONE', #7268, 125.0000000000000000 ) ;
#8091 = CIRCLE ( 'NONE', #40827, 125.0000000000000000 ) ;
#8092 = EDGE_CURVE ( 'NONE', #41126, #35764, #14897, .T. ) ;
#8093 = AXIS2_PLACEMENT_3D ( 'NONE', #41268, #16605, #48663 ) ;
#8094 = DIRECTION ( 'NONE',  ( 0.000000000000000000, -0.000000000000000000, -1.000000000000000000 ) ) ;
#8095 = ORIENTED_EDGE ( 'NONE', *, *, #6396, .T. ) ;
#8096 = ORIENTED_EDGE ( 'NONE', *, *, #28607, .T. ) ;
#8097 = VECTOR ( 'NONE', #1393, 1000.000000000000000 ) ;
#8098 = FACE_OUTER_BOUND ( 'NONE', #8374, .T. ) ;
#8099 = ORIENTED_EDGE ( 'NONE', *, *, #4844, .F. ) ;
#8100 = CARTESIAN_POINT ( 'NONE',  ( -49.17567778057185990, -177.1207230881787780, 0.7175072570443320474 ) ) ;
#8101 = PLANE ( 'NONE',  #28868 ) ;
#8102 = LINE ( 'NONE', #39372, #725 ) ;
#8103 = CARTESIAN_POINT ( 'NONE',  ( -85.48706473349324142, -189.7472609257535510, -118.3487137068146637 ) ) ;
#8104 = ORIENTED_EDGE ( 'NONE', *, *, #7847, .F. ) ;
#8106 = VERTEX_POINT ( 'NONE', #34830 ) ;
#8105 = CARTESIAN_POINT ( 'NONE',  ( -48.47912675150885065, -188.5000000000000284, 6.938893903907228378E-15 ) ) ;
#8107 = CIRCLE ( 'NONE', #13188, 9.000000000000001776 ) ;
#8108 = ORIENTED_EDGE ( 'NONE', *, *, #26620, .F. ) ;
#8109 = VECTOR ( 'NONE', #29526, 1000.000000000000000 ) ;
#8110 = EDGE_CURVE ( 'NONE', #40799, #3837, #8662, .T. ) ;
#8111 = DIRECTION ( 'NONE',  ( 0.6528221181905119463, 0.000000000000000000, 0.7575112421616284619 ) ) ;
#8112 = ORIENTED_EDGE ( 'NONE', *, *, #37938, .T. ) ;
#8113 = DIRECTION ( 'NONE',  ( 0.000000000000000000, -1.000000000000000000, 0.000000000000000000 ) ) ;
#8114 = VERTEX_POINT ( 'NONE', #10933 ) ;
#8115 = VECTOR ( 'NONE', #45503, 1000.000000000000000 ) ;
#8116 = DIRECTION ( 'NONE',  ( -0.000000000000000000, -1.000000000000000000, 0.000000000000000000 ) ) ;
#8117 = ORIENTED_EDGE ( 'NONE', *, *, #28561, .T. ) ;
#8119 = PLANE ( 'NONE',  #19926 ) ;
#8118 = DIRECTION ( 'NONE',  ( -0.000000000000000000, 1.000000000000000000, -0.000000000000000000 ) ) ;
#8120 = ORIENTED_EDGE ( 'NONE', *, *, #41424, .F. ) ;
#8121 = EDGE_CURVE ( 'NONE', #39858, #22860, #22519, .T. ) ;
#8122 = ORIENTED_EDGE ( 'NONE', *, *, #48160, .F. ) ;
#8123 = DIRECTION ( 'NONE',  ( 0.9720229140804123036, 0.000000000000000000, -0.2348860457809775759 ) ) ;
#8124 = VECTOR ( 'NONE', #11085, 1000.000000000000000 ) ;
#8125 = LINE ( 'NONE', #35198, #27348 ) ;
#8126 = VECTOR ( 'NONE', #5832, 1000.000000000000000 ) ;
#8127 = DIRECTION ( 'NONE',  ( 1.000000000000000000, -0.000000000000000000, -0.000000000000000000 ) ) ;
#8128 = CARTESIAN_POINT ( 'NONE',  ( -40.30502441601360886, -175.3837268820161057, 123.7303097900624920 ) ) ;
#8129 = CARTESIAN_POINT ( 'NONE',  ( 76.04209377433251404, -175.3837268820161057, -10.93003379476866854 ) ) ;
#8130 = VECTOR ( 'NONE', #49750, 1000.000000000000000 ) ;
#8131 = VECTOR ( 'NONE', #34496, 1000.000000000000000 ) ;
#8132 = DIRECTION ( 'NONE',  ( 0.000000000000000000, 0.000000000000000000, 1.000000000000000000 ) ) ;
#8133 = ORIENTED_EDGE ( 'NONE', *, *, #49350, .T. ) ;
#8134 = ADVANCED_FACE ( 'NONE', ( #2782 ), #50892, .F. ) ;
#8135 = VECTOR ( 'NONE', #43709, 1000.000000000000000 ) ;
#8136 = PLANE ( 'NONE',  #21291 ) ;
#8137 = FACE_OUTER_BOUND ( 'NONE', #6124, .T. ) ;
#8138 = VECTOR ( 'NONE', #50215, 999.9999999999998863 ) ;
#8139 = DIRECTION ( 'NONE',  ( -0.6300878435817203194, 0.000000000000000000, 0.7765238627180349740 ) ) ;
#8140 = VERTEX_POINT ( 'NONE', #43243 ) ;
#8141 = DIRECTION ( 'NONE',  ( 0.000000000000000000, -1.000000000000000000, 0.000000000000000000 ) ) ;
#8142 = DIRECTION ( 'NONE',  ( -0.000000000000000000, 0.6631226582408039638, 0.7485107481710934207 ) ) ;
#8143 = CARTESIAN_POINT ( 'NONE',  ( -180.0000000000000568, -155.0173647354142759, -14.76740078976489201 ) ) ;
#8144 = ORIENTED_EDGE ( 'NONE', *, *, #13664, .F. ) ;
#8145 = ORIENTED_EDGE ( 'NONE', *, *, #28112, .T. ) ;
#8146 = ORIENTED_EDGE ( 'NONE', *, *, #22460, .F. ) ;
#8147 = EDGE_CURVE ( 'NONE', #20203, #11822, #7253, .T. ) ;
#8148 = CIRCLE ( 'NONE', #6515, 125.0000000000000000 ) ;
#8149 = CARTESIAN_POINT ( 'NONE',  ( 27.50603775690333563, -175.3837268820161057, -99.25348746834811209 ) ) ;
#8150 = VECTOR ( 'NONE', #19445, 1000.000000000000000 ) ;
#8151 = LINE ( 'NONE', #24189, #9377 ) ;
#8152 = DIRECTION ( 'NONE',  ( 0.5085311186492273983, 0.000000000000000000, -0.8610436117673514467 ) ) ;
#8153 = DIRECTION ( 'NONE',  ( 0.000000000000000000, -1.000000000000000000, -0.000000000000000000 ) ) ;
#8154 = VERTEX_POINT ( 'NONE', #3560 ) ;
#8155 = ADVANCED_FACE ( 'NONE', ( #131 ), #27729, .T. ) ;
#8156 = LINE ( 'NONE', #4738, #25186 ) ;
#8157 = VERTEX_POINT ( 'NONE', #23535 ) ;
#8158 = ORIENTED_EDGE ( 'NONE', *, *, #45971, .T. ) ;
#8159 = VECTOR ( 'NONE', #4546, 1000.000000000000114 ) ;
#8160 = EDGE_CURVE ( 'NONE', #27933, #44506, #34572, .T. ) ;
#8161 = AXIS2_PLACEMENT_3D ( 'NONE', #50269, #5867, #17938 ) ;
#8162 = EDGE_LOOP ( 'NONE', ( #22713, #15772, #42847, #13116 ) ) ;
#8163 = LINE ( 'NONE', #43394, #2390 ) ;
#8164 = AXIS2_PLACEMENT_3D ( 'NONE', #51965, #28011, #15953 ) ;
#8165 = AXIS2_PLACEMENT_3D ( 'NONE', #36332, #13214, #29237 ) ;
#8166 = ORIENTED_EDGE ( 'NONE', *, *, #28881, .T. ) ;
#8167 = CIRCLE ( 'NONE', #40039, 125.0000000000000000 ) ;
#8168 = DIRECTION ( 'NONE',  ( 0.000000000000000000, -0.000000000000000000, -1.000000000000000000 ) ) ;
#8169 = CARTESIAN_POINT ( 'NONE',  ( -332.3517673607765914, -110.7312321683605916, -58.62557946887767457 ) ) ;
#8172 = ORIENTED_EDGE ( 'NONE', *, *, #23994, .F. ) ;
#8171 = FACE_OUTER_BOUND ( 'NONE', #8887, .T. ) ;
#8170 = CARTESIAN_POINT ( 'NONE',  ( -136.1415351158078408, -175.3837268820161057, -89.10837311819175000 ) ) ;
#8173 = EDGE_CURVE ( 'NONE', #2222, #32491, #3521, .T. ) ;
#8174 = DIRECTION ( 'NONE',  ( 0.000000000000000000, 0.5680647467311540355, -0.8229838658936575735 ) ) ;
#8175 = ORIENTED_EDGE ( 'NONE', *, *, #27236, .F. ) ;
#8176 = DIRECTION ( 'NONE',  ( -0.000000000000000000, 1.000000000000000000, -0.000000000000000000 ) ) ;
#8177 = ORIENTED_EDGE ( 'NONE', *, *, #42160, .F. ) ;
#8178 = DIRECTION ( 'NONE',  ( 0.000000000000000000, -0.3546048870425235200, 0.9350162426854194964 ) ) ;
#8179 = FACE_OUTER_BOUND ( 'NONE', #32810, .T. ) ;
#8181 = CARTESIAN_POINT ( 'NONE',  ( 1.755575411425465360, -175.3837268820161057, 114.4616734920527392 ) ) ;
#8180 = CARTESIAN_POINT ( 'NONE',  ( 73.87536152799695799, -193.5000000000000000, -25.58083653558413317 ) ) ;
#8182 = ORIENTED_EDGE ( 'NONE', *, *, #3175, .F. ) ;
#8183 = APPLICATION_CONTEXT ( 'automotive_design' ) ;
#8184 = DIRECTION ( 'NONE',  ( -0.000000000000000000, 1.000000000000000000, -0.000000000000000000 ) ) ;
#8185 = AXIS2_PLACEMENT_3D ( 'NONE', #38739, #18785, #51132 ) ;
#8186 = LINE ( 'NONE', #24221, #21135 ) ;
#8187 = AXIS2_PLACEMENT_3D ( 'NONE', #40950, #28070, #4972 ) ;
#8188 = DIRECTION ( 'NONE',  ( 1.000000000000000000, 0.000000000000000000, -8.718379230999705894E-17 ) ) ;
#8189 = EDGE_LOOP ( 'NONE', ( #48816, #4340, #50370, #51923 ) ) ;
#8190 = CARTESIAN_POINT ( 'NONE',  ( -91.84482189527193441, -193.5000000000000000, -117.2365833888816695 ) ) ;
#8191 = FACE_OUTER_BOUND ( 'NONE', #7223, .T. ) ;
#8192 = AXIS2_PLACEMENT_3D ( 'NONE', #31683, #8795, #28250 ) ;
#8193 = CARTESIAN_POINT ( 'NONE',  ( 57.31108707223381060, -189.7472609257535510, -66.58401203837752291 ) ) ;
#8194 = EDGE_LOOP ( 'NONE', ( #11014, #12159, #4864, #50373 ) ) ;
#8195 = DIRECTION ( 'NONE',  ( -1.000000000000000000, 0.000000000000000000, 0.000000000000000000 ) ) ;
#8196 = PLANE ( 'NONE',  #4662 ) ;
#8197 = ORIENTED_EDGE ( 'NONE', *, *, #552, .F. ) ;
#8198 = DIRECTION ( 'NONE',  ( -0.8124868780056863082, 0.000000000000000000, 0.5829794791144649047 ) ) ;
#8199 = VERTEX_POINT ( 'NONE', #39550 ) ;
#8200 = VECTOR ( 'NONE', #46123, 1000.000000000000000 ) ;
#8201 = CARTESIAN_POINT ( 'NONE',  ( -145.6517069852672535, -193.5000000000000000, 78.62880929222943394 ) ) ;
#8202 = CYLINDRICAL_SURFACE ( 'NONE', #13529, 124.9999999999999858 ) ;
#8203 = VECTOR ( 'NONE', #1402, 1000.000000000000114 ) ;
#8204 = DIRECTION ( 'NONE',  ( 0.000000000000000000, 3.631354476378115974E-14, -1.000000000000000000 ) ) ;
#8205 = ADVANCED_FACE ( 'NONE', ( #36133 ), #35613, .T. ) ;
#8206 = CARTESIAN_POINT ( 'NONE',  ( -49.40581635894068313, -193.5000000000000000, -0.3758275821142418316 ) ) ;
#8207 = FACE_OUTER_BOUND ( 'NONE', #9170, .T. ) ;
#8208 = EDGE_CURVE ( 'NONE', #20769, #11778, #20109, .T. ) ;
#8209 = CARTESIAN_POINT ( 'NONE',  ( -58.17235712592530916, -177.1207230881787780, 123.6213615703899649 ) ) ;
#8210 = LINE ( 'NONE', #32116, #16954 ) ;
#8211 = LINE ( 'NONE', #24246, #23898 ) ;
#8213 = EDGE_LOOP ( 'NONE', ( #12974, #17160, #67, #17538 ) ) ;
#8212 = CARTESIAN_POINT ( 'NONE',  ( -48.47912675150885065, -193.5000000000000000, 6.938893903907228378E-15 ) ) ;
#8214 = EDGE_LOOP ( 'NONE', ( #49589, #25196, #2364, #21493 ) ) ;
#8215 = CARTESIAN_POINT ( 'NONE',  ( -60.00000000000000000, -63.50000000000000000, 60.00000000000000711 ) ) ;
#8216 = EDGE_CURVE ( 'NONE', #37898, #47019, #17829, .T. ) ;
#8217 = EDGE_CURVE ( 'NONE', #15211, #12738, #35405, .T. ) ;
#8218 = LINE ( 'NONE', #36589, #3617 ) ;
#8219 = ORIENTED_EDGE ( 'NONE', *, *, #1810, .F. ) ;
#8220 = CIRCLE ( 'NONE', #51051, 125.0000000000000000 ) ;
#8221 = VERTEX_POINT ( 'NONE', #49211 ) ;
#8222 = ADVANCED_FACE ( 'NONE', ( #40320 ), #47974, .F. ) ;
#8223 = VERTEX_POINT ( 'NONE', #47726 ) ;
#8224 = CARTESIAN_POINT ( 'NONE',  ( -141.2664123866436512, -193.5000000000000000, -83.75869879877495805 ) ) ;
#8225 = AXIS2_PLACEMENT_3D ( 'NONE', #49492, #21084, #9011 ) ;
#8226 = CARTESIAN_POINT ( 'NONE',  ( -12.13476221271688260, -189.7472609257535510, 119.5996955107804780 ) ) ;
#8227 = DIRECTION ( 'NONE',  ( -1.000000000000000000, -0.000000000000000000, -0.000000000000000000 ) ) ;
#8228 = ORIENTED_EDGE ( 'NONE', *, *, #4343, .F. ) ;
#8229 = ORIENTED_EDGE ( 'NONE', *, *, #32211, .F. ) ;
#8230 = EDGE_LOOP ( 'NONE', ( #19883, #10481, #10224, #23120 ) ) ;
#8231 = DIRECTION ( 'NONE',  ( -0.000000000000000000, 1.000000000000000000, -0.000000000000000000 ) ) ;
#8232 = LINE ( 'NONE', #31108, #17677 ) ;
#8233 = DIRECTION ( 'NONE',  ( -1.000000000000000000, 3.701062773504947387E-15, 9.758900497077123602E-15 ) ) ;
#8234 = FACE_OUTER_BOUND ( 'NONE', #3299, .T. ) ;
#8235 = CARTESIAN_POINT ( 'NONE',  ( -123.5870580700902366, -175.3837268820161057, -98.66508442481458019 ) ) ;
#8236 = ORIENTED_EDGE ( 'NONE', *, *, #182, .T. ) ;
#8237 = DIRECTION ( 'NONE',  ( 0.000000000000000000, 0.000000000000000000, 1.000000000000000000 ) ) ;
#8238 = DIRECTION ( 'NONE',  ( 0.000000000000000000, -1.000000000000000000, 0.000000000000000000 ) ) ;
#8239 = DIRECTION ( 'NONE',  ( 1.000000000000000000, 0.000000000000000000, -0.000000000000000000 ) ) ;
#8240 = CARTESIAN_POINT ( 'NONE',  ( -48.47912675150885065, -183.6283474603465606, 6.938893903907228378E-15 ) ) ;
#8241 = ORIENTED_EDGE ( 'NONE', *, *, #31605, .T. ) ;
#8242 = ORIENTED_EDGE ( 'NONE', *, *, #33940, .F. ) ;
#8243 = VERTEX_POINT ( 'NONE', #37105 ) ;
#8244 = DIRECTION ( 'NONE',  ( 0.000000000000000000, 1.000000000000000000, -0.000000000000000000 ) ) ;
#8245 = DIRECTION ( 'NONE',  ( 0.000000000000000000, 0.3546048870425331789, -0.9350162426854158326 ) ) ;
#8246 = VERTEX_POINT ( 'NONE', #7766 ) ;
#8247 = CARTESIAN_POINT ( 'NONE',  ( -339.1964088526558498, -68.51134412508150717, 21.38919645685156112 ) ) ;
#8248 = LINE ( 'NONE', #877, #50575 ) ;
#8249 = EDGE_LOOP ( 'NONE', ( #3458, #50058, #49167, #30850 ) ) ;
#8250 = CARTESIAN_POINT ( 'NONE',  ( -339.1964088526558498, -102.1108035431470427, 54.98865587491797413 ) ) ;
#8251 = EDGE_LOOP ( 'NONE', ( #24730, #42056, #19032, #9996 ) ) ;
#8252 = CARTESIAN_POINT ( 'NONE',  ( -161.4184887245413904, -193.5000000000000000, 51.19472891551360050 ) ) ;
#8253 = VERTEX_POINT ( 'NONE', #7517 ) ;
#8254 = CARTESIAN_POINT ( 'NONE',  ( 59.00260725618640123, -193.5000000000000000, -63.81752780152988436 ) ) ;
#8255 = FACE_BOUND ( 'NONE', #39558, .T. ) ;
#8256 =( GEOMETRIC_REPRESENTATION_CONTEXT ( 3 ) GLOBAL_UNCERTAINTY_ASSIGNED_CONTEXT ( ( #38494 ) ) GLOBAL_UNIT_ASSIGNED_CONTEXT ( ( #51007, #48078, #7864 ) ) REPRESENTATION_CONTEXT ( 'NONE', 'WORKASPACE' ) );
#8257 = VECTOR ( 'NONE', #25075, 1000.000000000000000 ) ;
#8258 = VECTOR ( 'NONE', #48312, 999.9999999999998863 ) ;
#8259 = CARTESIAN_POINT ( 'NONE',  ( 75.47134233844786877, -175.3837268820161057, -3.504489105734901244 ) ) ;
#8260 = VERTEX_POINT ( 'NONE', #17150 ) ;
#8261 = AXIS2_PLACEMENT_3D ( 'NONE', #11586, #20243, #35484 ) ;
#8262 = EDGE_CURVE ( 'NONE', #13126, #46591, #29557, .T. ) ;
#8263 = PLANE ( 'NONE',  #33223 ) ;
#8264 = EDGE_CURVE ( 'NONE', #24091, #21356, #11704, .T. ) ;
#8265 = CARTESIAN_POINT ( 'NONE',  ( -339.1964088526558498, -74.65991953890826949, 33.10432812419072945 ) ) ;
#8266 = FACE_OUTER_BOUND ( 'NONE', #35311, .T. ) ;
#8267 = ADVANCED_FACE ( 'NONE', ( #43515 ), #33162, .T. ) ;
#8268 = DIRECTION ( 'NONE',  ( 0.08879589532293853671, 0.000000000000000000, -0.9960498426152166740 ) ) ;
#8269 = ADVANCED_FACE ( 'NONE', ( #27475 ), #51935, .F. ) ;
#8270 = ORIENTED_EDGE ( 'NONE', *, *, #9616, .T. ) ;
#8271 = LINE ( 'NONE', #39787, #34521 ) ;
#8272 = VERTEX_POINT ( 'NONE', #24062 ) ;
#8273 = ORIENTED_EDGE ( 'NONE', *, *, #21739, .F. ) ;
#8274 = CIRCLE ( 'NONE', #4948, 60.00000000000000000 ) ;
#8275 = EDGE_CURVE ( 'NONE', #41080, #47094, #47458, .T. ) ;
#8276 = CARTESIAN_POINT ( 'NONE',  ( 0.000000000000000000, -64.93017642821470758, 7.111664135063263892 ) ) ;
#8278 = VERTEX_POINT ( 'NONE', #41302 ) ;
#8277 = DIRECTION ( 'NONE',  ( 0.000000000000000000, 0.000000000000000000, -1.000000000000000000 ) ) ;
#8279 = ADVANCED_FACE ( 'NONE', ( #15407 ), #35356, .T. ) ;
#8280 = ORIENTED_EDGE ( 'NONE', *, *, #1812, .T. ) ;
#8281 = CARTESIAN_POINT ( 'NONE',  ( -172.6359455740846158, -183.6283474603465606, -14.49428645563797069 ) ) ;
#8282 = EDGE_CURVE ( 'NONE', #41229, #33330, #49986, .T. ) ;
#8283 = EDGE_CURVE ( 'NONE', #36522, #43333, #33689, .T. ) ;
#8284 = AXIS2_PLACEMENT_3D ( 'NONE', #30164, #30408, #1533 ) ;
#8285 = EDGE_CURVE ( 'NONE', #40286, #2431, #21162, .T. ) ;
#8286 = CARTESIAN_POINT ( 'NONE',  ( -48.47912675150885065, -120.5000000000000284, 6.938893903907228378E-15 ) ) ;
#8287 = ORIENTED_EDGE ( 'NONE', *, *, #48841, .T. ) ;
#8288 = EDGE_CURVE ( 'NONE', #33417, #9630, #25540, .T. ) ;
#8289 = CARTESIAN_POINT ( 'NONE',  ( -48.18706998087187543, -177.1207230881787780, -0.9564009842765152092 ) ) ;
#8290 = DIRECTION ( 'NONE',  ( -0.000000000000000000, 1.000000000000000000, 0.000000000000000000 ) ) ;
#8291 = EDGE_LOOP ( 'NONE', ( #34473, #50256, #32578, #44678 ) ) ;
#8292 = DIRECTION ( 'NONE',  ( 0.000000000000000000, -1.000000000000000000, 0.000000000000000000 ) ) ;
#8293 = DIRECTION ( 'NONE',  ( 0.5586467658036415873, 0.000000000000000000, 0.8294056854502090959 ) ) ;
#8294 = EDGE_CURVE ( 'NONE', #28453, #26725, #29735, .T. ) ;
#8295 = LINE ( 'NONE', #12220, #46241 ) ;
#8296 = CYLINDRICAL_SURFACE ( 'NONE', #25734, 125.0000000000000000 ) ;
#8297 = ORIENTED_EDGE ( 'NONE', *, *, #45031, .T. ) ;
#8298 = ORIENTED_EDGE ( 'NONE', *, *, #47801, .F. ) ;
#8299 = ORIENTED_EDGE ( 'NONE', *, *, #48263, .F. ) ;
#8300 = CARTESIAN_POINT ( 'NONE',  ( -161.8276685539205744, -183.6283474603465606, 50.28156562190587664 ) ) ;
#8301 = ORIENTED_EDGE ( 'NONE', *, *, #24208, .F. ) ;
#8302 = CARTESIAN_POINT ( 'NONE',  ( 52.16997862029128186, -189.7472609257535510, 72.42760398749086903 ) ) ;
#8303 = AXIS2_PLACEMENT_3D ( 'NONE', #14161, #10196, #21779 ) ;
#8304 =( GEOMETRIC_REPRESENTATION_CONTEXT ( 3 ) GLOBAL_UNCERTAINTY_ASSIGNED_CONTEXT ( ( #27427 ) ) GLOBAL_UNIT_ASSIGNED_CONTEXT ( ( #5171, #25393, #17526 ) ) REPRESENTATION_CONTEXT ( 'NONE', 'WORKASPACE' ) );
#8305 = DIRECTION ( 'NONE',  ( -0.000000000000000000, 1.000000000000000000, -0.000000000000000000 ) ) ;
#8306 = FACE_BOUND ( 'NONE', #41972, .T. ) ;
#8307 = DIRECTION ( 'NONE',  ( 0.000000000000000000, 0.000000000000000000, 1.000000000000000000 ) ) ;
#8308 = EDGE_LOOP ( 'NONE', ( #49001, #38988, #46261, #6941 ) ) ;
#8309 = CIRCLE ( 'NONE', #41881, 60.00000000000000000 ) ;
#8310 = EDGE_CURVE ( 'NONE', #35696, #28453, #2135, .T. ) ;
#8311 = VERTEX_POINT ( 'NONE', #46056 ) ;
#8313 = EDGE_LOOP ( 'NONE', ( #25244, #17307, #3130, #45504 ) ) ;
#8312 = PLANE ( 'NONE',  #29840 ) ;
#8314 = VECTOR ( 'NONE', #40640, 1000.000000000000000 ) ;
#8315 = ORIENTED_EDGE ( 'NONE', *, *, #17602, .F. ) ;
#8316 = CARTESIAN_POINT ( 'NONE',  ( -151.4272465800706016, -183.6283474603465606, 70.89911581792887318 ) ) ;
#8317 = CARTESIAN_POINT ( 'NONE',  ( 73.09196206113300320, -177.1207230881787780, 29.07697310430963356 ) ) ;
#8318 = DIRECTION ( 'NONE',  ( 0.000000000000000000, -1.000000000000000000, -0.000000000000000000 ) ) ;
#8319 = CARTESIAN_POINT ( 'NONE',  ( -339.1964088526558498, -64.99044476834235695, 7.608018572112245970 ) ) ;
#8320 = ORIENTED_EDGE ( 'NONE', *, *, #23576, .T. ) ;
#8321 = CARTESIAN_POINT ( 'NONE',  ( -339.1964088526558498, -178.8432607619609485, -20.45418021416653076 ) ) ;
#8322 = ORIENTED_EDGE ( 'NONE', *, *, #37175, .F. ) ;
#8323 = CIRCLE ( 'NONE', #36869, 125.0000000000000000 ) ;
#8324 = ADVANCED_FACE ( 'NONE', ( #17680 ), #25808, .T. ) ;
#8325 = ORIENTED_EDGE ( 'NONE', *, *, #43908, .T. ) ;
#8326 = CARTESIAN_POINT ( 'NONE',  ( -158.3442440847887269, -193.5000000000000000, -59.62093586438114556 ) ) ;
#8327 = DIRECTION ( 'NONE',  ( 0.1182731709213730997, 0.000000000000000000, -0.9929810960135161402 ) ) ;
#8328 = CARTESIAN_POINT ( 'NONE',  ( -160.0000000000000284, -123.5000000000000284, 41.63467731922665394 ) ) ;
#8329 = LINE ( 'NONE', #40359, #29790 ) ;
#8330 = ADVANCED_FACE ( 'NONE', ( #13465 ), #38133, .F. ) ;
#8331 = EDGE_CURVE ( 'NONE', #16064, #9382, #1368, .T. ) ;
#8332 = CYLINDRICAL_SURFACE ( 'NONE', #28030, 4.999999999999997335 ) ;
#8333 = DIRECTION ( 'NONE',  ( 0.000000000000000000, 1.000000000000000000, -0.000000000000000000 ) ) ;
#8334 = EDGE_CURVE ( 'NONE', #27228, #29227, #37093, .T. ) ;
#8335 = ORIENTED_EDGE ( 'NONE', *, *, #40361, .T. ) ;
#8336 = DIRECTION ( 'NONE',  ( -0.000000000000000000, 1.000000000000000000, -0.000000000000000000 ) ) ;
#8337 = CARTESIAN_POINT ( 'NONE',  ( -82.43766229206461560, -183.6283474603465606, -119.2602935412679983 ) ) ;
#8338 = ADVANCED_FACE ( 'NONE', ( #42087 ), #45783, .F. ) ;
#8339 = DIRECTION ( 'NONE',  ( 0.000000000000000000, 0.000000000000000000, -1.000000000000000000 ) ) ;
#8340 = FACE_BOUND ( 'NONE', #41562, .T. ) ;
#8341 = ORIENTED_EDGE ( 'NONE', *, *, #13203, .T. ) ;
#8342 = AXIS2_PLACEMENT_3D ( 'NONE', #33031, #17022, #40378 ) ;
#8343 = CARTESIAN_POINT ( 'NONE',  ( -339.1964088526558498, -84.00150778970767362, -43.83057281297470098 ) ) ;
#8344 = CIRCLE ( 'NONE', #12538, 125.0000000000000000 ) ;
#8345 = DIRECTION ( 'NONE',  ( -0.6068001458185834363, 0.000000000000000000, -0.7948544414133608127 ) ) ;
#8346 = ORIENTED_EDGE ( 'NONE', *, *, #8602, .T. ) ;
#8347 = CARTESIAN_POINT ( 'NONE',  ( 68.59638248015004081, -193.5000000000000000, -43.79868877201405297 ) ) ;
#8348 = EDGE_CURVE ( 'NONE', #29932, #38087, #37637, .T. ) ;
#8349 = ORIENTED_EDGE ( 'NONE', *, *, #21076, .T. ) ;
#8350 = CARTESIAN_POINT ( 'NONE',  ( -336.3521761649654422, -98.41210887299327226, -53.46519113769058151 ) ) ;
#8351 = EDGE_CURVE ( 'NONE', #8740, #9394, #13981, .T. ) ;
#8352 = DIRECTION ( 'NONE',  ( 1.000000000000000000, -0.000000000000000000, 0.000000000000000000 ) ) ;
#8353 = LINE ( 'NONE', #32781, #43881 ) ;
#8354 = EDGE_CURVE ( 'NONE', #33846, #8674, #8544, .T. ) ;
#8355 = CARTESIAN_POINT ( 'NONE',  ( -56.65322908700500193, -175.3837268820161057, -123.7303097900624351 ) ) ;
#8356 = ORIENTED_EDGE ( 'NONE', *, *, #19828, .T. ) ;
#8357 = EDGE_CURVE ( 'NONE', #7888, #36418, #48862, .T. ) ;
#8358 = VECTOR ( 'NONE', #29304, 1000.000000000000114 ) ;
#8359 = VERTEX_POINT ( 'NONE', #33446 ) ;
#8360 = PLANE ( 'NONE',  #17525 ) ;
#8361 = EDGE_LOOP ( 'NONE', ( #41452, #33683, #3468, #12954 ) ) ;
#8362 = PLANE ( 'NONE',  #35157 ) ;
#8363 = DIRECTION ( 'NONE',  ( 0.9646355819083556327, 0.000000000000000000, 0.2635871660690782825 ) ) ;
#8364 = FACE_OUTER_BOUND ( 'NONE', #7199, .T. ) ;
#8365 = ADVANCED_FACE ( 'NONE', ( #21002 ), #36489, .F. ) ;
#8366 = PLANE ( 'NONE',  #21705 ) ;
#8367 = CARTESIAN_POINT ( 'NONE',  ( -74.51199343215203896, -193.5000000000000000, -122.2591094863194598 ) ) ;
#8368 = ORIENTED_EDGE ( 'NONE', *, *, #12540, .T. ) ;
#8371 = ORIENTED_EDGE ( 'NONE', *, *, #7214, .T. ) ;
#8370 = CARTESIAN_POINT ( 'NONE',  ( 5.542374969221969039, -177.1207230881787780, 112.7238987608088365 ) ) ;
#8369 = FACE_OUTER_BOUND ( 'NONE', #1971, .T. ) ;
#8372 = VERTEX_POINT ( 'NONE', #40432 ) ;
#8373 = LINE ( 'NONE', #13089, #13078 ) ;
#8374 = EDGE_LOOP ( 'NONE', ( #20452, #20229, #20508, #30138 ) ) ;
#8375 = DIRECTION ( 'NONE',  ( 0.000000000000000000, 0.000000000000000000, -1.000000000000000000 ) ) ;
#8376 = VERTEX_POINT ( 'NONE', #37022 ) ;
#8377 = DIRECTION ( 'NONE',  ( 0.000000000000000000, -1.000000000000000000, -1.387778780781445182E-16 ) ) ;
#8378 = DIRECTION ( 'NONE',  ( 0.000000000000000000, 1.000000000000000000, 0.000000000000000000 ) ) ;
#8379 = ORIENTED_EDGE ( 'NONE', *, *, #14673, .F. ) ;
#8381 = CARTESIAN_POINT ( 'NONE',  ( -170.0000000000000284, -123.5000000000000284, -41.63467731922663972 ) ) ;
#8380 = LINE ( 'NONE', #12041, #43444 ) ;
#8382 = ORIENTED_EDGE ( 'NONE', *, *, #48522, .F. ) ;
#8383 = ORIENTED_EDGE ( 'NONE', *, *, #30168, .T. ) ;
#8384 = CARTESIAN_POINT ( 'NONE',  ( -330.4913330509368166, -68.51134412508180560, -21.38919645685231075 ) ) ;
#8385 = LINE ( 'NONE', #48863, #29785 ) ;
#8386 = DIRECTION ( 'NONE',  ( -0.5085311186492154079, 0.000000000000000000, -0.8610436117673585521 ) ) ;
#8387 = CARTESIAN_POINT ( 'NONE',  ( -157.4685091425930921, -193.5000000000000000, -59.13814366165038905 ) ) ;
#8388 = DIRECTION ( 'NONE',  ( -0.000000000000000000, 1.000000000000000000, 0.000000000000000000 ) ) ;
#8389 = DIRECTION ( 'NONE',  ( 0.000000000000000000, -0.000000000000000000, 1.000000000000000000 ) ) ;
#8390 = EDGE_LOOP ( 'NONE', ( #30265, #3329, #30716, #50538 ) ) ;
#8391 = EDGE_CURVE ( 'NONE', #20806, #26640, #37928, .T. ) ;
#8392 = APPLICATION_PROTOCOL_DEFINITION ( 'draft international standard', 'automotive_design', 1998, #5204 ) ;
#8393 = CARTESIAN_POINT ( 'NONE',  ( -60.00000000000000000, 20.00000000000000000, 60.00000000000000711 ) ) ;
#8394 = DIRECTION ( 'NONE',  ( -0.000000000000000000, -0.9927088740980548609, -0.1205366802553164696 ) ) ;
#8395 = CARTESIAN_POINT ( 'NONE',  ( -330.4913330509368166, -163.6602333390101762, -44.57752413667967772 ) ) ;
#8396 = VECTOR ( 'NONE', #29876, 1000.000000000000000 ) ;
#8397 = VECTOR ( 'NONE', #2467, 1000.000000000000000 ) ;
#8398 = DIRECTION ( 'NONE',  ( -0.5085311186492094127, 0.000000000000000000, -0.8610436117673619938 ) ) ;
#8399 = ORIENTED_EDGE ( 'NONE', *, *, #26340, .F. ) ;
#8400 = CARTESIAN_POINT ( 'NONE',  ( 35.67816836544800907, -193.5000000000000000, -92.42591454022745268 ) ) ;
#8401 = CARTESIAN_POINT ( 'NONE',  ( -140.1460956102404509, -189.7472609257535510, 84.98333260264821831 ) ) ;
#8402 = CARTESIAN_POINT ( 'NONE',  ( -339.1964088526558498, -79.66942718702553350, -39.49849221029258928 ) ) ;
#8403 = EDGE_LOOP ( 'NONE', ( #32253, #28819, #30796, #20978 ) ) ;
#8404 = ORIENTED_EDGE ( 'NONE', *, *, #5508, .T. ) ;
#8405 = ORIENTED_EDGE ( 'NONE', *, *, #48204, .T. ) ;
#8406 = FACE_OUTER_BOUND ( 'NONE', #47307, .T. ) ;
#8407 = VECTOR ( 'NONE', #2412, 1000.000000000000000 ) ;
#8408 = CARTESIAN_POINT ( 'NONE',  ( -119.6907301311197216, -193.5000000000000000, 101.5140743725400370 ) ) ;
#8409 = EDGE_CURVE ( 'NONE', #11143, #8243, #21263, .T. ) ;
#8410 = PLANE ( 'NONE',  #24550 ) ;
#8411 = CARTESIAN_POINT ( 'NONE',  ( -19.51863976943889512, -193.5000000000000000, 120.5706864261537419 ) ) ;
#8412 = EDGE_LOOP ( 'NONE', ( #41893, #848 ) ) ;
#8413 = DIRECTION ( 'NONE',  ( 0.000000000000000000, -1.000000000000000000, 0.000000000000000000 ) ) ;
#8414 = DIRECTION ( 'NONE',  ( 0.000000000000000000, -0.9927088740980556381, -0.1205366802553095307 ) ) ;
#8415 = EDGE_CURVE ( 'NONE', #19199, #25045, #4986, .T. ) ;
#8416 = ORIENTED_EDGE ( 'NONE', *, *, #52012, .T. ) ;
#8417 = ORIENTED_EDGE ( 'NONE', *, *, #40235, .T. ) ;
#8418 = CARTESIAN_POINT ( 'NONE',  ( -114.1105527140175155, -193.5000000000000000, 106.3838142112217611 ) ) ;
#8419 = VECTOR ( 'NONE', #46643, 1000.000000000000000 ) ;
#8420 = AXIS2_PLACEMENT_3D ( 'NONE', #17412, #25274, #21331 ) ;
#8421 = CARTESIAN_POINT ( 'NONE',  ( 75.27070168362158142, -175.3837268820161057, 17.63462396184792169 ) ) ;
#8422 = CARTESIAN_POINT ( 'NONE',  ( -143.3583119192899460, -183.6283474603465606, -81.38144888055207105 ) ) ;
#8425 = ORIENTED_EDGE ( 'NONE', *, *, #21696, .F. ) ;
#8424 = CARTESIAN_POINT ( 'NONE',  ( -305.0000000000000568, -109.6270296344155923, 58.37414404713457117 ) ) ;
#8423 = CARTESIAN_POINT ( 'NONE',  ( -330.0000000000000568, -123.5000000000000142, 60.00000000000000000 ) ) ;
#8426 = CARTESIAN_POINT ( 'NONE',  ( -143.3583119192899744, -193.5000000000000000, -81.38144888055202841 ) ) ;
#8427 = VERTEX_POINT ( 'NONE', #41217 ) ;
#8428 = DIRECTION ( 'NONE',  ( 0.000000000000000000, -0.000000000000000000, 1.000000000000000000 ) ) ;
#8429 = DIRECTION ( 'NONE',  ( 0.6068001458185890984, 0.000000000000000000, 0.7948544414133565938 ) ) ;
#8430 = EDGE_LOOP ( 'NONE', ( #23671, #13574, #38798, #38663 ) ) ;
#8431 = DIRECTION ( 'NONE',  ( 0.000000000000000000, 0.000000000000000000, -1.000000000000000000 ) ) ;
#8432 = DIRECTION ( 'NONE',  ( 0.000000000000000000, -0.000000000000000000, -1.000000000000000000 ) ) ;
#8434 = DIRECTION ( 'NONE',  ( 0.000000000000000000, 0.000000000000000000, -1.000000000000000000 ) ) ;
#8433 = CARTESIAN_POINT ( 'NONE',  ( -330.4913330509368166, -74.65991953890832633, 33.10432812419081472 ) ) ;
#8435 = EDGE_LOOP ( 'NONE', ( #24960, #49116, #51788, #41986 ) ) ;
#8436 = CARTESIAN_POINT ( 'NONE',  ( -332.3517673607765914, -127.9985676343858501, 58.88711093124869222 ) ) ;
#8437 = DIRECTION ( 'NONE',  ( -0.000000000000000000, 0.000000000000000000, 1.000000000000000000 ) ) ;
#8439 = VECTOR ( 'NONE', #28820, 1000.000000000000114 ) ;
#8438 = DIRECTION ( 'NONE',  ( 1.000000000000000000, 0.000000000000000000, 0.000000000000000000 ) ) ;
#8440 = ORIENTED_EDGE ( 'NONE', *, *, #14388, .F. ) ;
#8441 = CARTESIAN_POINT ( 'NONE',  ( -305.0000000000000568, -121.8677111499054320, 59.97779283292990016 ) ) ;
#8442 = CARTESIAN_POINT ( 'NONE',  ( -336.3521761649654422, -140.1754235130667610, -56.65561927338005432 ) ) ;
#8443 = DIRECTION ( 'NONE',  ( -0.000000000000000000, -1.000000000000000000, -0.000000000000000000 ) ) ;
#8444 = ORIENTED_EDGE ( 'NONE', *, *, #33334, .T. ) ;
#8445 = ADVANCED_FACE ( 'NONE', ( #16814 ), #45197, .F. ) ;
#8446 = DIRECTION ( 'NONE',  ( 0.000000000000000000, 0.000000000000000000, -1.000000000000000000 ) ) ;
#8447 = LINE ( 'NONE', #3466, #49989 ) ;
#8448 = ORIENTED_EDGE ( 'NONE', *, *, #16890, .T. ) ;
#8449 = CARTESIAN_POINT ( 'NONE',  ( -330.4913330509368166, -175.9742670995615015, -26.97593913775547136 ) ) ;
#8450 = ORIENTED_EDGE ( 'NONE', *, *, #38060, .F. ) ;
#8451 = CARTESIAN_POINT ( 'NONE',  ( -330.4913330509368166, -123.5000000000000284, 0.000000000000000000 ) ) ;
#8452 = LINE ( 'NONE', #48413, #6814 ) ;
#8453 = AXIS2_PLACEMENT_3D ( 'NONE', #30553, #13505, #46604 ) ;
#8454 = FACE_OUTER_BOUND ( 'NONE', #38370, .T. ) ;
#8455 = FACE_OUTER_BOUND ( 'NONE', #1291, .T. ) ;
#8456 = CARTESIAN_POINT ( 'NONE',  ( -336.3521761649654422, -70.03480886230919111, 25.08789112700620194 ) ) ;
#8457 = VECTOR ( 'NONE', #21602, 1000.000000000000114 ) ;
#8458 = DIRECTION ( 'NONE',  ( 0.000000000000000000, -1.000000000000000000, 0.000000000000000000 ) ) ;
#8459 = LINE ( 'NONE', #24489, #42110 ) ;
#8460 = EDGE_CURVE ( 'NONE', #31552, #7207, #32887, .T. ) ;
#8461 = CARTESIAN_POINT ( 'NONE',  ( -149.7090673587772756, -193.5000000000000000, -71.61357856150526402 ) ) ;
#8463 = ORIENTED_EDGE ( 'NONE', *, *, #12016, .F. ) ;
#8462 = DIRECTION ( 'NONE',  ( -1.000000000000000000, 0.000000000000000000, 0.000000000000000000 ) ) ;
#8464 = EDGE_LOOP ( 'NONE', ( #42144, #44483, #15442, #32817 ) ) ;
#8465 = CARTESIAN_POINT ( 'NONE',  ( -131.9398708394020332, -183.6283474603465606, 91.70840728318374602 ) ) ;
#8466 = CARTESIAN_POINT ( 'NONE',  ( -48.47912675150885065, -175.3837268820161057, 6.938893903907228378E-15 ) ) ;
#8467 = ORIENTED_EDGE ( 'NONE', *, *, #10579, .F. ) ;
#8468 = EDGE_LOOP ( 'NONE', ( #45154, #28487, #18067, #35387 ) ) ;
#8469 = AXIS2_PLACEMENT_3D ( 'NONE', #11960, #44027, #24068 ) ;
#8470 = ORIENTED_EDGE ( 'NONE', *, *, #46481, .F. ) ;
#8471 = DIRECTION ( 'NONE',  ( 0.6749830015182142207, 0.000000000000000000, -0.7378332790417239107 ) ) ;
#8472 = DIRECTION ( 'NONE',  ( 0.000000000000000000, -1.000000000000000000, 0.000000000000000000 ) ) ;
#8473 = LINE ( 'NONE', #24503, #6497 ) ;
#8474 = VERTEX_POINT ( 'NONE', #21523 ) ;
#8475 = EDGE_LOOP ( 'NONE', ( #35977, #50474, #43778, #34501 ) ) ;
#8476 = ORIENTED_EDGE ( 'NONE', *, *, #4205, .T. ) ;
#8477 = CARTESIAN_POINT ( 'NONE',  ( -332.3517673607765914, -180.1590281025188460, -19.74220186498920881 ) ) ;
#8478 = CARTESIAN_POINT ( 'NONE',  ( -112.7586829773731267, -175.3837268820161057, -107.2060569716373521 ) ) ;
#8480 = ORIENTED_EDGE ( 'NONE', *, *, #799, .F. ) ;
#8479 = DIRECTION ( 'NONE',  ( -0.8757349421956345248, 0.000000000000000000, -0.4827922027307490205 ) ) ;
#8481 = CARTESIAN_POINT ( 'NONE',  ( -336.3521761649654422, -176.5004679656469477, -25.97334715265976612 ) ) ;
#8482 = CARTESIAN_POINT ( 'NONE',  ( -336.3521761649654422, -174.9833430614318388, 28.86398714850502856 ) ) ;
#8483 = ORIENTED_EDGE ( 'NONE', *, *, #47021, .T. ) ;
#8484 = CARTESIAN_POINT ( 'NONE',  ( -108.5723883981724640, -183.6283474603465606, 109.6074810615846076 ) ) ;
#8485 = AXIS2_PLACEMENT_3D ( 'NONE', #2961, #27903, #19268 ) ;
#8486 = ADVANCED_FACE ( 'NONE', ( #8906 ), #16553, .F. ) ;
#8487 = CARTESIAN_POINT ( 'NONE',  ( -336.3521761649654422, -181.1761995186066088, -12.53476669029101842 ) ) ;
#8488 = DIRECTION ( 'NONE',  ( 0.000000000000000000, -0.000000000000000000, -1.000000000000000000 ) ) ;
#8489 = DIRECTION ( 'NONE',  ( -0.000000000000000000, 1.000000000000000000, -0.000000000000000000 ) ) ;
#8490 = AXIS2_PLACEMENT_3D ( 'NONE', #51721, #31737, #47777 ) ;
#8491 = ADVANCED_FACE ( 'NONE', ( #41477 ), #33079, .T. ) ;
#8492 = ORIENTED_EDGE ( 'NONE', *, *, #11730, .F. ) ;
#8493 = VERTEX_POINT ( 'NONE', #48614 ) ;
#8494 = FACE_OUTER_BOUND ( 'NONE', #33566, .T. ) ;
#8496 = VECTOR ( 'NONE', #47961, 1000.000000000000114 ) ;
#8495 = DIRECTION ( 'NONE',  ( 0.000000000000000000, 0.000000000000000000, -1.000000000000000000 ) ) ;
#8497 = ORIENTED_EDGE ( 'NONE', *, *, #40903, .F. ) ;
#8498 = CARTESIAN_POINT ( 'NONE',  ( -49.44376233341721161, -183.6283474603465606, 0.2635871660690650709 ) ) ;
#8499 = LINE ( 'NONE', #44260, #18688 ) ;
#8500 = ORIENTED_EDGE ( 'NONE', *, *, #38496, .T. ) ;
#8501 = ADVANCED_FACE ( 'NONE', ( #32819 ), #48871, .T. ) ;
#8502 = DIRECTION ( 'NONE',  ( -0.7175072570443299380, 0.000000000000000000, -0.6965510290629983725 ) ) ;
#8503 = EDGE_CURVE ( 'NONE', #23398, #6329, #4451, .T. ) ;
#8504 = DIRECTION ( 'NONE',  ( -0.3482016354343995812, 0.000000000000000000, 0.9374196611341205632 ) ) ;
#8505 = VERTEX_POINT ( 'NONE', #51566 ) ;
#8506 = DIRECTION ( 'NONE',  ( -0.000000000000000000, 0.1205366802553337752, 0.9927088740980526405 ) ) ;
#8507 = ORIENTED_EDGE ( 'NONE', *, *, #2663, .F. ) ;
#8508 = ADVANCED_FACE ( 'NONE', ( #47636 ), #8647, .T. ) ;
#8509 = VECTOR ( 'NONE', #13213, 1000.000000000000114 ) ;
#8510 = LINE ( 'NONE', #48485, #9406 ) ;
#8511 = EDGE_LOOP ( 'NONE', ( #22811, #16900, #8084, #23193 ) ) ;
#8512 = DIRECTION ( 'NONE',  ( -0.3202698538628350744, 0.000000000000000000, -0.9473263538541923934 ) ) ;
#8513 = CARTESIAN_POINT ( 'NONE',  ( -26.53529504715431031, -193.5000000000000000, 123.0587999703026725 ) ) ;
#8514 = DIRECTION ( 'NONE',  ( -0.000000000000000000, 0.8854560256532157947, 0.4647231720437573488 ) ) ;
#8515 = CARTESIAN_POINT ( 'NONE',  ( -49.47517659412407198, -175.3837268820161057, 0.08879589532293177823 ) ) ;
#8516 = ORIENTED_EDGE ( 'NONE', *, *, #48741, .F. ) ;
#8517 = LINE ( 'NONE', #40836, #6073 ) ;
#8518 = ORIENTED_EDGE ( 'NONE', *, *, #17626, .T. ) ;
#8519 = ORIENTED_EDGE ( 'NONE', *, *, #35123, .T. ) ;
#8520 = EDGE_CURVE ( 'NONE', #6745, #8999, #17335, .T. ) ;
#8521 = CARTESIAN_POINT ( 'NONE',  ( -135.4258661347518853, -193.5000000000000000, -89.80681772907007598 ) ) ;
#8523 = VERTEX_POINT ( 'NONE', #37285 ) ;
#8522 = DIRECTION ( 'NONE',  ( 0.000000000000000000, 1.000000000000000000, -0.000000000000000000 ) ) ;
#8524 = AXIS2_PLACEMENT_3D ( 'NONE', #30614, #22750, #49842 ) ;
#8525 = EDGE_LOOP ( 'NONE', ( #40994, #10149, #26892, #49175 ) ) ;
#8526 = DIRECTION ( 'NONE',  ( -0.9151456172430181280, 0.000000000000000000, -0.4031234292879730674 ) ) ;
#8527 = VECTOR ( 'NONE', #14875, 1000.000000000000000 ) ;
#8528 = AXIS2_PLACEMENT_3D ( 'NONE', #40248, #20287, #36315 ) ;
#8529 = CARTESIAN_POINT ( 'NONE',  ( 23.33927677392130917, -193.5000000000000000, -102.3089288139528747 ) ) ;
#8530 = CARTESIAN_POINT ( 'NONE',  ( -48.02249751411513756, -189.7472609257535510, -0.8896570909947397743 ) ) ;
#8531 = ORIENTED_EDGE ( 'NONE', *, *, #23912, .F. ) ;
#8532 = DIRECTION ( 'NONE',  ( -0.000000000000000000, -1.000000000000000000, 0.000000000000000000 ) ) ;
#8533 = ORIENTED_EDGE ( 'NONE', *, *, #14962, .T. ) ;
#8534 = CARTESIAN_POINT ( 'NONE',  ( 4.109287492203100634, -183.6283474603465606, -113.3995532942336979 ) ) ;
#8535 = CARTESIAN_POINT ( 'NONE',  ( -49.03777351731249468, -193.5000000000000000, -0.8294056854502022125 ) ) ;
#8536 = DIRECTION ( 'NONE',  ( -1.000000000000000000, 0.000000000000000000, 0.000000000000000000 ) ) ;
#8537 = CARTESIAN_POINT ( 'NONE',  ( 39.56636334395317789, -183.6283474603465606, -87.31661597576083977 ) ) ;
#8538 = ORIENTED_EDGE ( 'NONE', *, *, #28433, .F. ) ;
#8539 = AXIS2_PLACEMENT_3D ( 'NONE', #8212, #36849, #4268 ) ;
#8540 = VERTEX_POINT ( 'NONE', #24420 ) ;
#8541 = EDGE_LOOP ( 'NONE', ( #43932, #25950, #38914, #7840 ) ) ;
#8542 = PLANE ( 'NONE',  #13156 ) ;
#8543 = PLANE ( 'NONE',  #12589 ) ;
#8544 = CIRCLE ( 'NONE', #43810, 31.65769145387501027 ) ;
#8545 = CIRCLE ( 'NONE', #973, 125.0000000000000000 ) ;
#8546 = DIRECTION ( 'NONE',  ( 0.000000000000000000, 0.000000000000000000, -1.000000000000000000 ) ) ;
#8547 = FACE_BOUND ( 'NONE', #29222, .T. ) ;
#8548 = DIRECTION ( 'NONE',  ( 0.000000000000000000, 1.000000000000000000, 0.000000000000000000 ) ) ;
#8549 = ORIENTED_EDGE ( 'NONE', *, *, #31719, .F. ) ;
#8550 = ADVANCED_FACE ( 'NONE', ( #33352 ), #4712, .T. ) ;
#8551 = EDGE_CURVE ( 'NONE', #23514, #28503, #43677, .T. ) ;
#8552 = ORIENTED_EDGE ( 'NONE', *, *, #20947, .T. ) ;
#8554 = EDGE_LOOP ( 'NONE', ( #30551, #31808, #22845, #20110 ) ) ;
#8553 = DIRECTION ( 'NONE',  ( 0.000000000000000000, 1.000000000000000000, 0.000000000000000000 ) ) ;
#8555 = ORIENTED_EDGE ( 'NONE', *, *, #48828, .T. ) ;
#8556 = CARTESIAN_POINT ( 'NONE',  ( -336.3521761649654422, -153.2494431741581025, -51.01861988938816950 ) ) ;
#8557 = CARTESIAN_POINT ( 'NONE',  ( -155.4465502054561057, -183.6283474603465606, 64.67588669375881238 ) ) ;
#8558 = AXIS2_PLACEMENT_3D ( 'NONE', #13428, #42053, #21842 ) ;
#8559 = PLANE ( 'NONE',  #13733 ) ;
#8560 = DIRECTION ( 'NONE',  ( 0.000000000000000000, 7.100801428331730794E-14, -1.000000000000000000 ) ) ;
#8561 = VERTEX_POINT ( 'NONE', #13895 ) ;
#8562 = ADVANCED_FACE ( 'NONE', ( #6006 ), #20320, .T. ) ;
#8563 = DIRECTION ( 'NONE',  ( 0.000000000000000000, 0.000000000000000000, -1.000000000000000000 ) ) ;
#8564 = VECTOR ( 'NONE', #1413, 1000.000000000000000 ) ;
#8565 = VERTEX_POINT ( 'NONE', #1547 ) ;
#8566 = EDGE_CURVE ( 'NONE', #45141, #22586, #50172, .T. ) ;
#8567 = AXIS2_PLACEMENT_3D ( 'NONE', #48358, #509, #40450 ) ;
#8568 = VERTEX_POINT ( 'NONE', #14166 ) ;
#8569 = FACE_OUTER_BOUND ( 'NONE', #18680, .T. ) ;
#8570 = EDGE_CURVE ( 'NONE', #5941, #2933, #22031, .T. ) ;
#8571 = LINE ( 'NONE', #41155, #5180 ) ;
#8572 = CARTESIAN_POINT ( 'NONE',  ( -48.71401279728984690, -177.1207230881787780, 0.9720229140804159673 ) ) ;
#8573 = CARTESIAN_POINT ( 'NONE',  ( -336.3521761649654422, -171.1288023355047585, 34.85916744524404720 ) ) ;
#8574 = EDGE_CURVE ( 'NONE', #2935, #23376, #10200, .T. ) ;
#8575 = CYLINDRICAL_SURFACE ( 'NONE', #46505, 125.0000000000000000 ) ;
#8576 = DIRECTION ( 'NONE',  ( -0.000000000000000000, -0.8854560256532062468, 0.4647231720437755564 ) ) ;
#8577 = EDGE_LOOP ( 'NONE', ( #6735, #37385, #18295, #43378 ) ) ;
#8578 = DIRECTION ( 'NONE',  ( 1.000000000000000000, 0.000000000000000000, 0.000000000000000000 ) ) ;
#8579 = CARTESIAN_POINT ( 'NONE',  ( -47.87232660569025455, -175.3837268820161057, -0.7948544414133454916 ) ) ;
#8580 = CIRCLE ( 'NONE', #27892, 125.0000000000000000 ) ;
#8581 = AXIS2_PLACEMENT_3D ( 'NONE', #19314, #46927, #15895 ) ;
#8582 = DIRECTION ( 'NONE',  ( 0.000000000000000000, -0.3546048870425426158, -0.9350162426854121689 ) ) ;
#8583 = FACE_BOUND ( 'NONE', #10195, .T. ) ;
#8584 = ORIENTED_EDGE ( 'NONE', *, *, #43952, .F. ) ;
#8585 = AXIS2_PLACEMENT_3D ( 'NONE', #5588, #34212, #1643 ) ;
#8586 = AXIS2_PLACEMENT_3D ( 'NONE', #24847, #15939, #31950 ) ;
#8587 = PLANE ( 'NONE',  #35682 ) ;
#8588 = ORIENTED_EDGE ( 'NONE', *, *, #32596, .F. ) ;
#8589 = DIRECTION ( 'NONE',  ( -1.000000000000000000, 0.000000000000000000, -0.000000000000000000 ) ) ;
#8590 = CARTESIAN_POINT ( 'NONE',  ( -47.66663987350317910, -189.7472609257535510, 0.5829794791144832233 ) ) ;
#8591 = EDGE_LOOP ( 'NONE', ( #28945, #35265, #25319, #6281 ) ) ;
#8592 = ADVANCED_FACE ( 'NONE', ( #38578 ), #33602, .F. ) ;
#8593 = LINE ( 'NONE', #8854, #4176 ) ;
#8594 = DIRECTION ( 'NONE',  ( -0.000000000000000000, 0.5680647467311457088, -0.8229838658936633466 ) ) ;
#8596 = VERTEX_POINT ( 'NONE', #30183 ) ;
#8595 = DIRECTION ( 'NONE',  ( 0.8294056854501971054, 0.000000000000000000, 0.5586467658036594619 ) ) ;
#8597 = VECTOR ( 'NONE', #14722, 1000.000000000000227 ) ;
#8598 = DIRECTION ( 'NONE',  ( -0.000000000000000000, 1.000000000000000000, -0.000000000000000000 ) ) ;
#8599 = ORIENTED_EDGE ( 'NONE', *, *, #4550, .T. ) ;
#8600 = AXIS2_PLACEMENT_3D ( 'NONE', #18872, #30698, #12479 ) ;
#8601 = ORIENTED_EDGE ( 'NONE', *, *, #20326, .T. ) ;
#8602 = EDGE_CURVE ( 'NONE', #23236, #9916, #30425, .T. ) ;
#8603 = CARTESIAN_POINT ( 'NONE',  ( 26.89923761108473954, -175.3837268820161057, -98.45863302693476271 ) ) ;
#8604 = ORIENTED_EDGE ( 'NONE', *, *, #15065, .T. ) ;
#8605 = CARTESIAN_POINT ( 'NONE',  ( -26.53529504715431031, -189.7472609257535510, 123.0587999703026725 ) ) ;
#8606 = CARTESIAN_POINT ( 'NONE',  ( -332.3517673607765914, -165.2193480479701293, -43.12187378178659714 ) ) ;
#8607 = CARTESIAN_POINT ( 'NONE',  ( -170.0000000000000284, -173.5000000000000284, 60.00000000000000000 ) ) ;
#8608 = ADVANCED_FACE ( 'NONE', ( #29914 ), #41752, .T. ) ;
#8609 = EDGE_CURVE ( 'NONE', #2088, #36416, #37552, .T. ) ;
#8610 = EDGE_CURVE ( 'NONE', #19842, #28928, #50672, .T. ) ;
#8611 = EDGE_CURVE ( 'NONE', #16275, #32338, #6538, .T. ) ;
#8612 = CIRCLE ( 'NONE', #21233, 125.0000000000000000 ) ;
#8613 = EDGE_CURVE ( 'NONE', #49730, #41086, #34382, .T. ) ;
#8614 = CYLINDRICAL_SURFACE ( 'NONE', #30957, 125.0000000000000000 ) ;
#8615 = CARTESIAN_POINT ( 'NONE',  ( -169.7849785064912282, -175.3837268820161057, -25.70779184431770048 ) ) ;
#8616 = VERTEX_POINT ( 'NONE', #10723 ) ;
#8619 = ORIENTED_EDGE ( 'NONE', *, *, #7891, .F. ) ;
#8618 = FACE_OUTER_BOUND ( 'NONE', #44368, .T. ) ;
#8617 = LINE ( 'NONE', #37259, #18983 ) ;
#8620 = AXIS2_PLACEMENT_3D ( 'NONE', #6208, #17775, #41416 ) ;
#8621 = AXIS2_PLACEMENT_3D ( 'NONE', #39165, #22885, #10799 ) ;
#8622 = ORIENTED_EDGE ( 'NONE', *, *, #8262, .F. ) ;
#8623 = EDGE_CURVE ( 'NONE', #2171, #32119, #6788, .T. ) ;
#8624 = DIRECTION ( 'NONE',  ( 1.000000000000000000, -6.525800561034911606E-17, 5.781354811211940401E-17 ) ) ;
#8625 = VERTEX_POINT ( 'NONE', #26480 ) ;
#8626 = DIRECTION ( 'NONE',  ( 0.000000000000000000, -0.000000000000000000, -1.000000000000000000 ) ) ;
#8627 = EDGE_LOOP ( 'NONE', ( #27453, #7714, #27817, #49298 ) ) ;
#8628 = CARTESIAN_POINT ( 'NONE',  ( -79.88691714431334390, -183.6283474603465606, 119.9572859573367367 ) ) ;
#8629 = VECTOR ( 'NONE', #1290, 1000.000000000000227 ) ;
#8630 = DIRECTION ( 'NONE',  ( 0.000000000000000000, 0.000000000000000000, 1.000000000000000000 ) ) ;
#8631 = ORIENTED_EDGE ( 'NONE', *, *, #8110, .T. ) ;
#8632 = EDGE_CURVE ( 'NONE', #50991, #15872, #30678, .T. ) ;
#8634 = CARTESIAN_POINT ( 'NONE',  ( 17.44316424268006926, -183.6283474603465606, -105.0256126866231625 ) ) ;
#8633 = CARTESIAN_POINT ( 'NONE',  ( -332.3517673607765914, -64.50000000000000000, -1.632288850093980725 ) ) ;
#8635 = EDGE_LOOP ( 'NONE', ( #32225, #9024, #42874, #37415 ) ) ;
#8636 = EDGE_CURVE ( 'NONE', #10170, #27297, #42251, .T. ) ;
#8637 = VERTEX_POINT ( 'NONE', #49641 ) ;
#8638 = DIRECTION ( 'NONE',  ( 0.000000000000000000, 0.000000000000000000, -1.000000000000000000 ) ) ;
#8639 = FACE_OUTER_BOUND ( 'NONE', #19296, .T. ) ;
#8640 = EDGE_CURVE ( 'NONE', #34090, #37367, #6266, .T. ) ;
#8641 = DIRECTION ( 'NONE',  ( -0.000000000000000000, 1.000000000000000000, 0.000000000000000000 ) ) ;
#8642 = CARTESIAN_POINT ( 'NONE',  ( -339.1964088526558498, -74.65991953890876687, -33.10432812419148263 ) ) ;
#8643 = DIRECTION ( 'NONE',  ( 0.000000000000000000, 0.000000000000000000, 1.000000000000000000 ) ) ;
#8644 = CIRCLE ( 'NONE', #1935, 125.0000000000000000 ) ;
#8645 = CARTESIAN_POINT ( 'NONE',  ( 39.56636334395317789, -177.1207230881787780, -87.31661597576083977 ) ) ;
#8646 = EDGE_CURVE ( 'NONE', #10667, #42459, #50423, .T. ) ;
#8647 = PLANE ( 'NONE',  #16972 ) ;
#8648 = DIRECTION ( 'NONE',  ( -0.000000000000000000, 1.000000000000000000, -0.000000000000000000 ) ) ;
#8649 = CARTESIAN_POINT ( 'NONE',  ( -173.0003472773501301, -175.3837268820161057, 10.93003379476953363 ) ) ;
#8650 = EDGE_CURVE ( 'NONE', #7741, #32981, #9690, .T. ) ;
#8651 = VECTOR ( 'NONE', #46119, 1000.000000000000000 ) ;
#8652 = CARTESIAN_POINT ( 'NONE',  ( -48.41988612361514299, -183.6283474603465606, -0.9982437317643144681 ) ) ;
#8653 = ORIENTED_EDGE ( 'NONE', *, *, #44578, .F. ) ;
#8654 = ORIENTED_EDGE ( 'NONE', *, *, #19872, .T. ) ;
#8655 = DIRECTION ( 'NONE',  ( 0.000000000000000000, 0.9927088740980544168, 0.1205366802553199251 ) ) ;
#8656 = FACE_OUTER_BOUND ( 'NONE', #46417, .T. ) ;
#8657 = FACE_OUTER_BOUND ( 'NONE', #40917, .T. ) ;
#8658 = ORIENTED_EDGE ( 'NONE', *, *, #24658, .T. ) ;
#8659 = EDGE_LOOP ( 'NONE', ( #17682, #40453, #44384, #6809 ) ) ;
#8660 = VECTOR ( 'NONE', #25786, 999.9999999999998863 ) ;
#8661 = ORIENTED_EDGE ( 'NONE', *, *, #35871, .T. ) ;
#8662 = CIRCLE ( 'NONE', #19575, 125.0000000000000000 ) ;
#8663 = EDGE_CURVE ( 'NONE', #10734, #1781, #18856, .T. ) ;
#8664 = EDGE_CURVE ( 'NONE', #49035, #3976, #43802, .T. ) ;
#8665 = CARTESIAN_POINT ( 'NONE',  ( 1.734723475976807094E-15, 20.00000000000000000, 41.00000000000000711 ) ) ;
#8666 = VECTOR ( 'NONE', #24241, 1000.000000000000000 ) ;
#8667 = DIRECTION ( 'NONE',  ( -0.9151456172430181280, 0.000000000000000000, -0.4031234292879730674 ) ) ;
#8668 = CARTESIAN_POINT ( 'NONE',  ( -48.47912675150885065, -117.5479369270332057, 6.938893903907228378E-15 ) ) ;
#8669 = ORIENTED_EDGE ( 'NONE', *, *, #4236, .T. ) ;
#8670 = AXIS2_PLACEMENT_3D ( 'NONE', #11175, #26427, #43236 ) ;
#8671 = CARTESIAN_POINT ( 'NONE',  ( 26.89923761108473599, -193.5000000000000000, -98.45863302693476271 ) ) ;
#8672 = ORIENTED_EDGE ( 'NONE', *, *, #48690, .T. ) ;
#8673 = LINE ( 'NONE', #792, #2985 ) ;
#8674 = VERTEX_POINT ( 'NONE', #27252 ) ;
#8675 = ORIENTED_EDGE ( 'NONE', *, *, #3608, .F. ) ;
#8676 = CARTESIAN_POINT ( 'NONE',  ( 66.73972540229263473, -193.5000000000000000, 45.83253885719642540 ) ) ;
#8677 = VECTOR ( 'NONE', #36774, 1000.000000000000000 ) ;
#8678 = EDGE_CURVE ( 'NONE', #31178, #27045, #11226, .T. ) ;
#8679 = EDGE_CURVE ( 'NONE', #33832, #44506, #51708, .T. ) ;
#8680 = TOROIDAL_SURFACE ( 'NONE', #43943, 9.000000000000000000, 2.000000000000000000 ) ;
#8681 = EDGE_CURVE ( 'NONE', #17017, #13772, #51453, .T. ) ;
#8682 = EDGE_CURVE ( 'NONE', #23051, #43457, #15352, .T. ) ;
#8683 = DIRECTION ( 'NONE',  ( 0.000000000000000000, 0.000000000000000000, 1.000000000000000000 ) ) ;
#8684 = FACE_OUTER_BOUND ( 'NONE', #32046, .T. ) ;
#8687 = EDGE_LOOP ( 'NONE', ( #21149, #11882, #22361, #41646 ) ) ;
#8686 = CARTESIAN_POINT ( 'NONE',  ( -48.47912675150885065, -175.3837268820161057, 6.938893903907228378E-15 ) ) ;
#8685 = LINE ( 'NONE', #28641, #35895 ) ;
#8688 = DIRECTION ( 'NONE',  ( 0.000000000000000000, 0.4647231720437724478, 0.8854560256532078011 ) ) ;
#8689 = ORIENTED_EDGE ( 'NONE', *, *, #51713, .F. ) ;
#8690 = DIRECTION ( 'NONE',  ( -0.9027978299657477557, 0.000000000000000000, 0.4300652022765115712 ) ) ;
#8691 = CARTESIAN_POINT ( 'NONE',  ( -166.9790462269951661, -193.5000000000000000, 36.52255268223138529 ) ) ;
#8692 = VERTEX_POINT ( 'NONE', #23835 ) ;
#8693 = FACE_OUTER_BOUND ( 'NONE', #35553, .T. ) ;
#8694 = DIRECTION ( 'NONE',  ( 0.000000000000000000, 0.000000000000000000, 1.000000000000000000 ) ) ;
#8696 = DIRECTION ( 'NONE',  ( 0.000000000000000000, -0.000000000000000000, 1.000000000000000000 ) ) ;
#8695 = DIRECTION ( 'NONE',  ( 0.000000000000000000, 0.000000000000000000, 1.000000000000000000 ) ) ;
#8697 = CIRCLE ( 'NONE', #39728, 125.0000000000000000 ) ;
#8698 = ORIENTED_EDGE ( 'NONE', *, *, #33560, .T. ) ;
#8699 = DIRECTION ( 'NONE',  ( -0.2059786187410953262, 0.000000000000000000, -0.9785564922995046988 ) ) ;
#8700 = VECTOR ( 'NONE', #29317, 1000.000000000000000 ) ;
#8701 = CARTESIAN_POINT ( 'NONE',  ( -170.2790847791494855, -193.5000000000000000, -28.10285082451569494 ) ) ;
#8702 = CARTESIAN_POINT ( 'NONE',  ( -330.4913330509368166, -180.6659093959934523, -14.60509510167853442 ) ) ;
#8703 = EDGE_LOOP ( 'NONE', ( #46703, #49008, #40519, #17814 ) ) ;
#8704 = CARTESIAN_POINT ( 'NONE',  ( -330.4913330509368166, -63.99980407363864288, -7.728304129924675969 ) ) ;
#8705 = CARTESIAN_POINT ( 'NONE',  ( -336.3521761649654422, -91.32752733096738496, -49.48329383994654052 ) ) ;
#8706 = DIRECTION ( 'NONE',  ( 0.7765238627180393038, 0.000000000000000000, 0.6300878435817147682 ) ) ;
#8707 = ORIENTED_EDGE ( 'NONE', *, *, #46418, .T. ) ;
#8708 = DIRECTION ( 'NONE',  ( -0.4639789333096864810, 0.000000000000000000, 0.8858462335218260097 ) ) ;
#8709 = ADVANCED_FACE ( 'NONE', ( #28026 ), #23337, .F. ) ;
#8710 = ORIENTED_EDGE ( 'NONE', *, *, #3625, .F. ) ;
#8711 = CARTESIAN_POINT ( 'NONE',  ( -305.0000000000000568, -63.50208336950359467, -0.4999999999996888600 ) ) ;
#8712 = VERTEX_POINT ( 'NONE', #30949 ) ;
#8713 = DIRECTION ( 'NONE',  ( -1.000000000000000000, 0.000000000000000000, -0.000000000000000000 ) ) ;
#8714 = VECTOR ( 'NONE', #8336, 1000.000000000000000 ) ;
#8715 = DIRECTION ( 'NONE',  ( -0.3758275821142357809, 0.000000000000000000, -0.9266896074318343723 ) ) ;
#8716 = FACE_BOUND ( 'NONE', #1185, .T. ) ;
#8717 = CARTESIAN_POINT ( 'NONE',  ( -332.3517673607765914, -127.9985676343858501, 58.88711093124869222 ) ) ;
#8718 = AXIS2_PLACEMENT_3D ( 'NONE', #7300, #51707, #24356 ) ;
#8719 = DIRECTION ( 'NONE',  ( -1.000000000000000000, -2.497772389992548343E-15, -1.013386094502323194E-14 ) ) ;
#8720 = LINE ( 'NONE', #29467, #44622 ) ;
#8721 = DIRECTION ( 'NONE',  ( 0.000000000000000000, 0.000000000000000000, -1.000000000000000000 ) ) ;
#8723 = ORIENTED_EDGE ( 'NONE', *, *, #37465, .T. ) ;
#8722 = LINE ( 'NONE', #47903, #46342 ) ;
#8724 = ORIENTED_EDGE ( 'NONE', *, *, #25830, .T. ) ;
#8725 = CARTESIAN_POINT ( 'NONE',  ( -74.51199343215201054, -183.6283474603465606, -122.2591094863194883 ) ) ;
#8726 = CIRCLE ( 'NONE', #26365, 4.000000000000003553 ) ;
#8727 = DIRECTION ( 'NONE',  ( 0.000000000000000000, 0.2393156642875582940, 0.9709418174260519008 ) ) ;
#8728 = ORIENTED_EDGE ( 'NONE', *, *, #37827, .F. ) ;
#8729 = ORIENTED_EDGE ( 'NONE', *, *, #40693, .F. ) ;
#8730 = ORIENTED_EDGE ( 'NONE', *, *, #36352, .T. ) ;
#8731 = CARTESIAN_POINT ( 'NONE',  ( -12.76653800058364574, -189.7472609257535510, -119.7898618611244927 ) ) ;
#8732 = EDGE_CURVE ( 'NONE', #5675, #16257, #24564, .T. ) ;
#8733 = DIRECTION ( 'NONE',  ( 0.000000000000000000, 0.000000000000000000, 1.000000000000000000 ) ) ;
#8734 = DIRECTION ( 'NONE',  ( -0.000000000000000000, 0.000000000000000000, -1.000000000000000000 ) ) ;
#8735 = ORIENTED_EDGE ( 'NONE', *, *, #36276, .T. ) ;
#8736 = ORIENTED_EDGE ( 'NONE', *, *, #51700, .F. ) ;
#8737 = CARTESIAN_POINT ( 'NONE',  ( -55.71438232577009586, -193.5000000000000000, -124.7904286264580804 ) ) ;
#8738 = PLANE ( 'NONE',  #13462 ) ;
#8740 = VERTEX_POINT ( 'NONE', #35397 ) ;
#8739 = PLANE ( 'NONE',  #36715 ) ;
#8741 = PLANE ( 'NONE',  #22847 ) ;
#8742 = CARTESIAN_POINT ( 'NONE',  ( -47.48307690889363641, -193.5000000000000000, 0.08879589532294547560 ) ) ;
#8743 = CIRCLE ( 'NONE', #38119, 125.0000000000000000 ) ;
#8744 = ORIENTED_EDGE ( 'NONE', *, *, #22642, .F. ) ;
#8745 = DIRECTION ( 'NONE',  ( 0.000000000000000000, 0.000000000000000000, -1.000000000000000000 ) ) ;
#8746 = EDGE_LOOP ( 'NONE', ( #13809, #15390, #45727, #4872 ) ) ;
#8747 = AXIS2_PLACEMENT_3D ( 'NONE', #2824, #26740, #30670 ) ;
#8748 = CARTESIAN_POINT ( 'NONE',  ( -339.1964088526558498, -66.09477493971917283, -13.63415328425296202 ) ) ;
#8749 = CYLINDRICAL_SURFACE ( 'NONE', #49830, 16.00000000000000711 ) ;
#8750 = LINE ( 'NONE', #24274, #46706 ) ;
#8751 = CIRCLE ( 'NONE', #381, 125.0000000000000000 ) ;
#8752 = PRODUCT_DEFINITION ( 'UNKNOWN', '', #25890, #46912 ) ;
#8753 = ORIENTED_EDGE ( 'NONE', *, *, #22934, .T. ) ;
#8754 = VERTEX_POINT ( 'NONE', #3872 ) ;
#8755 = FACE_OUTER_BOUND ( 'NONE', #36638, .T. ) ;
#8756 = DIRECTION ( 'NONE',  ( 0.000000000000000000, -1.000000000000000000, 0.000000000000000000 ) ) ;
#8757 = ORIENTED_EDGE ( 'NONE', *, *, #40781, .F. ) ;
#8758 = EDGE_CURVE ( 'NONE', #49289, #28894, #15967, .T. ) ;
#8759 = LINE ( 'NONE', #37135, #46696 ) ;
#8760 = CARTESIAN_POINT ( 'NONE',  ( -332.3517673607765914, -152.3639871485048900, -51.48334306143194539 ) ) ;
#8761 = VERTEX_POINT ( 'NONE', #3603 ) ;
#8762 = DIRECTION ( 'NONE',  ( 0.000000000000000000, -0.3546048870425267951, 0.9350162426854181641 ) ) ;
#8763 = AXIS2_PLACEMENT_3D ( 'NONE', #50332, #10369, #26395 ) ;
#8764 = DIRECTION ( 'NONE',  ( -0.000000000000000000, 1.000000000000000000, -0.000000000000000000 ) ) ;
#8765 = ORIENTED_EDGE ( 'NONE', *, *, #10900, .T. ) ;
#8766 = LINE ( 'NONE', #9306, #23221 ) ;
#8767 = ORIENTED_EDGE ( 'NONE', *, *, #42322, .F. ) ;
#8768 = DIRECTION ( 'NONE',  ( -0.000000000000000000, -0.2393156642875615969, -0.9709418174260511236 ) ) ;
#8769 = CARTESIAN_POINT ( 'NONE',  ( -63.43218022845230308, -189.7472609257535510, 124.1024020384604540 ) ) ;
#8770 = ORIENTED_EDGE ( 'NONE', *, *, #27023, .T. ) ;
#8771 = CARTESIAN_POINT ( 'NONE',  ( 63.31225588004632243, -193.5000000000000000, 55.92572546981597981 ) ) ;
#8772 = DIRECTION ( 'NONE',  ( -0.000000000000000000, -0.4647231720437604574, 0.8854560256532141294 ) ) ;
#8773 = LINE ( 'NONE', #20093, #40847 ) ;
#8774 = EDGE_CURVE ( 'NONE', #10230, #1251, #44686, .T. ) ;
#8775 = DIRECTION ( 'NONE',  ( 0.000000000000000000, 1.000000000000000000, -0.000000000000000000 ) ) ;
#8776 = ORIENTED_EDGE ( 'NONE', *, *, #44358, .F. ) ;
#8777 = PLANE ( 'NONE',  #19404 ) ;
#8778 = ORIENTED_EDGE ( 'NONE', *, *, #6812, .F. ) ;
#8779 = ORIENTED_EDGE ( 'NONE', *, *, #19478, .T. ) ;
#8780 = ADVANCED_FACE ( 'NONE', ( #34876 ), #39589, .T. ) ;
#8781 = LINE ( 'NONE', #37421, #40371 ) ;
#8783 = EDGE_LOOP ( 'NONE', ( #17579, #25725, #2681, #7280 ) ) ;
#8782 = DIRECTION ( 'NONE',  ( 0.8757349421956345248, 0.000000000000000000, 0.4827922027307490205 ) ) ;
#8784 = CIRCLE ( 'NONE', #28925, 125.0000000000000000 ) ;
#8785 = CIRCLE ( 'NONE', #51597, 60.00000000000000000 ) ;
#8786 = VERTEX_POINT ( 'NONE', #11743 ) ;
#8787 = CARTESIAN_POINT ( 'NONE',  ( 65.12862465015750502, -193.5000000000000000, 49.69312418816386412 ) ) ;
#8788 = AXIS2_PLACEMENT_3D ( 'NONE', #39228, #35526, #4009 ) ;
#8789 = EDGE_CURVE ( 'NONE', #47477, #11775, #50941, .T. ) ;
#8790 = DIRECTION ( 'NONE',  ( 0.000000000000000000, 0.000000000000000000, -1.000000000000000000 ) ) ;
#8791 = ORIENTED_EDGE ( 'NONE', *, *, #44089, .F. ) ;
#8792 = CARTESIAN_POINT ( 'NONE',  ( -332.3517673607765914, -119.0014323656137947, -58.88711093124865670 ) ) ;
#8793 = ORIENTED_EDGE ( 'NONE', *, *, #18546, .F. ) ;
#8794 = DIRECTION ( 'NONE',  ( -0.000000000000000000, 1.000000000000000000, -0.000000000000000000 ) ) ;
#8795 = DIRECTION ( 'NONE',  ( 0.000000000000000000, 1.000000000000000000, -1.156482317317871232E-16 ) ) ;
#8796 = ADVANCED_FACE ( 'NONE', ( #46995 ), #19896, .T. ) ;
#8798 = AXIS2_PLACEMENT_3D ( 'NONE', #19727, #15286, #43656 ) ;
#8797 = LINE ( 'NONE', #20909, #19365 ) ;
#8799 = PLANE ( 'NONE',  #4761 ) ;
#8800 = VERTEX_POINT ( 'NONE', #10975 ) ;
#8801 = ORIENTED_EDGE ( 'NONE', *, *, #1912, .F. ) ;
#8802 = EDGE_CURVE ( 'NONE', #26457, #10145, #47504, .T. ) ;
#8803 = ORIENTED_EDGE ( 'NONE', *, *, #6919, .T. ) ;
#8804 = DIRECTION ( 'NONE',  ( -8.718379230999708359E-17, -0.8229838658936495799, 0.5680647467311656929 ) ) ;
#8805 = CARTESIAN_POINT ( 'NONE',  ( 52.59568867645218404, -175.3837268820161057, -73.54509967498589162 ) ) ;
#8806 = EDGE_CURVE ( 'NONE', #7086, #21227, #43839, .T. ) ;
#8807 = DIRECTION ( 'NONE',  ( 0.9785564922995017012, 0.000000000000000000, 0.2059786187411094538 ) ) ;
#8808 = DIRECTION ( 'NONE',  ( 0.000000000000000000, 0.000000000000000000, -1.000000000000000000 ) ) ;
#8809 = DIRECTION ( 'NONE',  ( 0.000000000000000000, 0.9350162426854121689, -0.3546048870425426158 ) ) ;
#8810 = ORIENTED_EDGE ( 'NONE', *, *, #48536, .F. ) ;
#8811 = ORIENTED_EDGE ( 'NONE', *, *, #18487, .F. ) ;
#8813 = VERTEX_POINT ( 'NONE', #35146 ) ;
#8812 = CARTESIAN_POINT ( 'NONE',  ( 8.294189685504184339, -175.3837268820161057, -110.2396968984190977 ) ) ;
#8814 = DIRECTION ( 'NONE',  ( 0.000000000000000000, -1.000000000000000000, 0.000000000000000000 ) ) ;
#8815 = ORIENTED_EDGE ( 'NONE', *, *, #46036, .T. ) ;
#8816 = VECTOR ( 'NONE', #14020, 1000.000000000000000 ) ;
#8817 = CARTESIAN_POINT ( 'NONE',  ( -49.08592689732743963, -189.7472609257535510, -0.7948544414133539293 ) ) ;
#8818 = EDGE_CURVE ( 'NONE', #10133, #38089, #15190, .T. ) ;
#8819 = DIRECTION ( 'NONE',  ( 0.000000000000000000, -0.000000000000000000, 1.000000000000000000 ) ) ;
#8820 = AXIS2_PLACEMENT_3D ( 'NONE', #45178, #37528, #8626 ) ;
#8821 = AXIS2_PLACEMENT_3D ( 'NONE', #4137, #20150, #36172 ) ;
#8822 = CARTESIAN_POINT ( 'NONE',  ( -164.0008810331606526, -189.7472609257535510, 47.74645837849825369 ) ) ;
#8823 = CARTESIAN_POINT ( 'NONE',  ( -152.0588566364587848, -177.1207230881787780, -68.17212999877148150 ) ) ;
#8824 = ORIENTED_EDGE ( 'NONE', *, *, #28783, .T. ) ;
#8825 = FACE_OUTER_BOUND ( 'NONE', #32151, .T. ) ;
#8827 = ADVANCED_FACE ( 'NONE', ( #7301 ), #28293, .T. ) ;
#8826 = EDGE_LOOP ( 'NONE', ( #5293, #45850, #48432, #46718 ) ) ;
#8828 = AXIS2_PLACEMENT_3D ( 'NONE', #24885, #36717, #28034 ) ;
#8829 = VERTEX_POINT ( 'NONE', #33010 ) ;
#8830 = FACE_OUTER_BOUND ( 'NONE', #37164, .T. ) ;
#8831 = CYLINDRICAL_SURFACE ( 'NONE', #11041, 125.0000000000000000 ) ;
#8832 = CARTESIAN_POINT ( 'NONE',  ( -339.1964088526558498, -64.99044476834235695, 7.608018572112245970 ) ) ;
#8833 = AXIS2_PLACEMENT_3D ( 'NONE', #46627, #6684, #22705 ) ;
#8834 = CARTESIAN_POINT ( 'NONE',  ( -55.99477380783403646, -193.5000000000000000, 123.7720294769269600 ) ) ;
#8835 = FACE_OUTER_BOUND ( 'NONE', #27952, .T. ) ;
#8836 = DIRECTION ( 'NONE',  ( 0.000000000000000000, -0.000000000000000000, -1.000000000000000000 ) ) ;
#8837 = DIRECTION ( 'NONE',  ( 0.000000000000000000, 0.000000000000000000, 1.000000000000000000 ) ) ;
#8838 = VERTEX_POINT ( 'NONE', #24113 ) ;
#8839 = VECTOR ( 'NONE', #3975, 1000.000000000000000 ) ;
#8840 = CARTESIAN_POINT ( 'NONE',  ( -330.4913330509368166, -122.9999999999994600, 59.00000000000002132 ) ) ;
#8841 = DIRECTION ( 'NONE',  ( -0.000000000000000000, -0.7485107481710977506, 0.6631226582407989678 ) ) ;
#8843 = AXIS2_PLACEMENT_3D ( 'NONE', #12360, #44435, #48903 ) ;
#8842 = DIRECTION ( 'NONE',  ( 0.000000000000000000, 0.000000000000000000, -1.000000000000000000 ) ) ;
#8844 = FACE_BOUND ( 'NONE', #5459, .T. ) ;
#8845 = ORIENTED_EDGE ( 'NONE', *, *, #35940, .F. ) ;
#8846 = CARTESIAN_POINT ( 'NONE',  ( -20.16057156355606139, -193.5000000000000000, -120.7230919990158782 ) ) ;
#8847 = ORIENTED_EDGE ( 'NONE', *, *, #37281, .T. ) ;
#8848 = CARTESIAN_POINT ( 'NONE',  ( -23.99795575808071035, -193.5000000000000000, -122.5792489240757703 ) ) ;
#8849 = EDGE_CURVE ( 'NONE', #32529, #9666, #48553, .T. ) ;
#8850 = ORIENTED_EDGE ( 'NONE', *, *, #49403, .F. ) ;
#8851 = EDGE_CURVE ( 'NONE', #28628, #51319, #20669, .T. ) ;
#8852 = LINE ( 'NONE', #37489, #26300 ) ;
#8853 = ORIENTED_EDGE ( 'NONE', *, *, #46117, .T. ) ;
#8854 = CARTESIAN_POINT ( 'NONE',  ( 66.03142248012325410, -177.1207230881787780, 50.12318939044039467 ) ) ;
#8855 = DIRECTION ( 'NONE',  ( 1.000000000000000000, 0.000000000000000000, 0.000000000000000000 ) ) ;
#8857 = ORIENTED_EDGE ( 'NONE', *, *, #23774, .F. ) ;
#8856 = DIRECTION ( 'NONE',  ( 0.9266896074318343723, 0.000000000000000000, -0.3758275821142357809 ) ) ;
#8858 = CIRCLE ( 'NONE', #2141, 125.0000000000000000 ) ;
#8859 = CIRCLE ( 'NONE', #38232, 60.00000000000000000 ) ;
#8860 = EDGE_CURVE ( 'NONE', #17733, #20353, #36963, .T. ) ;
#8861 = CARTESIAN_POINT ( 'NONE',  ( -332.3517673607765914, -86.34605966037949543, -45.90766452162698386 ) ) ;
#8862 = ORIENTED_EDGE ( 'NONE', *, *, #7852, .F. ) ;
#8863 = ORIENTED_EDGE ( 'NONE', *, *, #10537, .T. ) ;
#8864 = EDGE_CURVE ( 'NONE', #48760, #10162, #32760, .T. ) ;
#8865 = VERTEX_POINT ( 'NONE', #4918 ) ;
#8866 = APPLICATION_CONTEXT ( 'automotive_design' ) ;
#8867 = CARTESIAN_POINT ( 'NONE',  ( -336.3521761649654422, -174.9833430614318388, 28.86398714850502856 ) ) ;
#8868 = CARTESIAN_POINT ( 'NONE',  ( -130.2106798473772642, -175.3837268820161057, 94.57776286494217288 ) ) ;
#8869 = EDGE_CURVE ( 'NONE', #27646, #39413, #5177, .T. ) ;
#8870 = VERTEX_POINT ( 'NONE', #13312 ) ;
#8871 = VECTOR ( 'NONE', #45107, 1000.000000000000227 ) ;
#8872 = DIRECTION ( 'NONE',  ( -0.000000000000000000, 1.000000000000000000, -0.000000000000000000 ) ) ;
#8873 = VECTOR ( 'NONE', #4916, 1000.000000000000000 ) ;
#8874 = CARTESIAN_POINT ( 'NONE',  ( 56.28386853063362594, -175.3837268820161057, 66.33788548805519270 ) ) ;
#8875 = DIRECTION ( 'NONE',  ( -0.000000000000000000, 1.000000000000000000, -0.000000000000000000 ) ) ;
#8876 = ADVANCED_FACE ( 'NONE', ( #8069 ), #9115, .T. ) ;
#8877 = VECTOR ( 'NONE', #12820, 1000.000000000000114 ) ;
#8878 = CIRCLE ( 'NONE', #2169, 125.0000000000000000 ) ;
#8879 = PLANE ( 'NONE',  #22572 ) ;
#8880 = FACE_OUTER_BOUND ( 'NONE', #25041, .T. ) ;
#8881 = VERTEX_POINT ( 'NONE', #40121 ) ;
#8884 = EDGE_LOOP ( 'NONE', ( #8229, #6447, #10253, #9230 ) ) ;
#8883 = DIRECTION ( 'NONE',  ( 0.000000000000000000, -0.000000000000000000, -1.000000000000000000 ) ) ;
#8882 = DIRECTION ( 'NONE',  ( 0.000000000000000000, -0.4647231720437755564, -0.8854560256532062468 ) ) ;
#8885 = VERTEX_POINT ( 'NONE', #49323 ) ;
#8886 = DIRECTION ( 'NONE',  ( 0.000000000000000000, 0.000000000000000000, -1.000000000000000000 ) ) ;
#8887 = EDGE_LOOP ( 'NONE', ( #42493, #10261, #3304, #5615 ) ) ;
#8888 = ORIENTED_EDGE ( 'NONE', *, *, #22461, .T. ) ;
#8889 = DIRECTION ( 'NONE',  ( -0.000000000000000000, 1.000000000000000000, -0.000000000000000000 ) ) ;
#8890 = PLANE ( 'NONE',  #21688 ) ;
#8891 = ORIENTED_EDGE ( 'NONE', *, *, #15136, .T. ) ;
#8892 = CARTESIAN_POINT ( 'NONE',  ( -339.1964088526558498, -168.0775241366801254, -40.16023333900967884 ) ) ;
#8893 = ORIENTED_EDGE ( 'NONE', *, *, #19267, .T. ) ;
#8894 = VERTEX_POINT ( 'NONE', #20153 ) ;
#8895 = DIRECTION ( 'NONE',  ( 0.000000000000000000, 0.8660254037844375974, 0.5000000000000018874 ) ) ;
#8896 = AXIS2_PLACEMENT_3D ( 'NONE', #34123, #38830, #50175 ) ;
#8897 = CARTESIAN_POINT ( 'NONE',  ( -134.9506378406916838, -175.3837268820161057, 90.26448786734087548 ) ) ;
#8898 = AXIS2_PLACEMENT_3D ( 'NONE', #49637, #26216, #5499 ) ;
#8899 = DIRECTION ( 'NONE',  ( 0.000000000000000000, -0.000000000000000000, -1.000000000000000000 ) ) ;
#8900 = DIRECTION ( 'NONE',  ( 0.000000000000000000, -0.6631226582407863113, 0.7485107481711089639 ) ) ;
#8901 = ORIENTED_EDGE ( 'NONE', *, *, #22111, .T. ) ;
#8902 = AXIS2_PLACEMENT_3D ( 'NONE', #27577, #39643, #3656 ) ;
#8903 = CARTESIAN_POINT ( 'NONE',  ( -48.93575598890257794, -177.1207230881787780, 0.8896570909947506545 ) ) ;
#8904 = CIRCLE ( 'NONE', #8079, 125.0000000000000000 ) ;
#8905 = APPLICATION_PROTOCOL_DEFINITION ( 'draft international standard', 'automotive_design', 1998, #44796 ) ;
#8906 = FACE_OUTER_BOUND ( 'NONE', #22726, .T. ) ;
#8907 = DIRECTION ( 'NONE',  ( 0.000000000000000000, -0.2393156642875615969, -0.9709418174260511236 ) ) ;
#8908 = FACE_OUTER_BOUND ( 'NONE', #37803, .T. ) ;
#8909 = DIRECTION ( 'NONE',  ( -0.000000000000000000, 1.000000000000000000, -0.000000000000000000 ) ) ;
#8910 = ORIENTED_EDGE ( 'NONE', *, *, #6453, .T. ) ;
#8911 = ORIENTED_EDGE ( 'NONE', *, *, #1996, .T. ) ;
#8912 = CARTESIAN_POINT ( 'NONE',  ( -28.86423599357335590, -177.1207230881787780, 122.4396006697296144 ) ) ;
#8913 = AXIS2_PLACEMENT_3D ( 'NONE', #23950, #16082, #16613 ) ;
#8914 = EDGE_CURVE ( 'NONE', #44523, #14995, #36175, .T. ) ;
#8915 = CIRCLE ( 'NONE', #38277, 125.0000000000000000 ) ;
#8916 = VECTOR ( 'NONE', #12049, 1000.000000000000000 ) ;
#8917 = ADVANCED_FACE ( 'NONE', ( #49056 ), #20943, .T. ) ;
#8918 = FACE_OUTER_BOUND ( 'NONE', #19122, .T. ) ;
#8919 = DIRECTION ( 'NONE',  ( 0.000000000000000000, -1.000000000000000000, 0.000000000000000000 ) ) ;
#8920 = EDGE_CURVE ( 'NONE', #246, #16275, #48898, .T. ) ;
#8921 = VERTEX_POINT ( 'NONE', #40894 ) ;
#8922 = EDGE_CURVE ( 'NONE', #22978, #49147, #40363, .T. ) ;
#8923 = ORIENTED_EDGE ( 'NONE', *, *, #1027, .F. ) ;
#8924 = AXIS2_PLACEMENT_3D ( 'NONE', #51249, #39134, #23622 ) ;
#8925 = ORIENTED_EDGE ( 'NONE', *, *, #34601, .T. ) ;
#8926 = ADVANCED_FACE ( 'NONE', ( #29062 ), #12258, .T. ) ;
#8927 = VECTOR ( 'NONE', #46666, 1000.000000000000000 ) ;
#8928 = CARTESIAN_POINT ( 'NONE',  ( -305.0000000000000568, -123.5000000000000142, 60.00000000000000000 ) ) ;
#8929 = EDGE_CURVE ( 'NONE', #49151, #14954, #20406, .T. ) ;
#8930 = PLANE ( 'NONE',  #42142 ) ;
#8931 = CARTESIAN_POINT ( 'NONE',  ( -305.0000000000000568, -95.17484985463171654, -52.89315522109019696 ) ) ;
#8932 = DIRECTION ( 'NONE',  ( 0.000000000000000000, -1.000000000000000000, 0.000000000000000000 ) ) ;
#8933 = ORIENTED_EDGE ( 'NONE', *, *, #15183, .T. ) ;
#8934 = LINE ( 'NONE', #24974, #21634 ) ;
#8935 = EDGE_CURVE ( 'NONE', #43736, #10566, #25144, .T. ) ;
#8936 = DIRECTION ( 'NONE',  ( -0.000000000000000000, 1.000000000000000000, -0.000000000000000000 ) ) ;
#8937 = ORIENTED_EDGE ( 'NONE', *, *, #48831, .T. ) ;
#8938 = EDGE_CURVE ( 'NONE', #48723, #17876, #37217, .T. ) ;
#8939 = FACE_OUTER_BOUND ( 'NONE', #9823, .T. ) ;
#8940 = ORIENTED_EDGE ( 'NONE', *, *, #20215, .T. ) ;
#8941 = CARTESIAN_POINT ( 'NONE',  ( 59.80284513346456521, -183.6283474603465606, 62.45009659481583242 ) ) ;
#8942 = AXIS2_PLACEMENT_3D ( 'NONE', #15970, #19384, #19135 ) ;
#8943 = AXIS2_PLACEMENT_3D ( 'NONE', #12195, #44274, #47954 ) ;
#8944 = EDGE_CURVE ( 'NONE', #16500, #23459, #24608, .T. ) ;
#8945 = ORIENTED_EDGE ( 'NONE', *, *, #8986, .T. ) ;
#8946 = DIRECTION ( 'NONE',  ( 0.000000000000000000, 0.000000000000000000, -1.000000000000000000 ) ) ;
#8947 = AXIS2_PLACEMENT_3D ( 'NONE', #18066, #14642, #5982 ) ;
#8948 = ADVANCED_FACE ( 'NONE', ( #17261 ), #41937, .F. ) ;
#8949 = EDGE_CURVE ( 'NONE', #19112, #24906, #43025, .T. ) ;
#8950 = CARTESIAN_POINT ( 'NONE',  ( -130.7087404384255080, -189.7472609257535510, -94.14505102712755047 ) ) ;
#8953 = ORIENTED_EDGE ( 'NONE', *, *, #47659, .T. ) ;
#8952 = CARTESIAN_POINT ( 'NONE',  ( -280.0000000000000000, -123.5000000000000284, 20.00000000000002487 ) ) ;
#8951 = CARTESIAN_POINT ( 'NONE',  ( -30.00000000000000000, -43.50000000000000000, 30.00000000000000355 ) ) ;
#8954 = CIRCLE ( 'NONE', #5632, 125.0000000000000000 ) ;
#8955 = VECTOR ( 'NONE', #51504, 1000.000000000000114 ) ;
#8956 = VECTOR ( 'NONE', #24787, 1000.000000000000000 ) ;
#8957 = FACE_OUTER_BOUND ( 'NONE', #49271, .T. ) ;
#8959 = EDGE_LOOP ( 'NONE', ( #30667, #5756, #15138, #1029 ) ) ;
#8958 = AXIS2_PLACEMENT_3D ( 'NONE', #15900, #50418, #38307 ) ;
#8960 = CARTESIAN_POINT ( 'NONE',  ( -48.47912675150885065, -183.6283474603465606, 6.938893903907228378E-15 ) ) ;
#8961 = DIRECTION ( 'NONE',  ( 1.000000000000000000, -0.000000000000000000, -0.000000000000000000 ) ) ;
#8962 = ORIENTED_EDGE ( 'NONE', *, *, #24967, .F. ) ;
#8963 = DIRECTION ( 'NONE',  ( -0.000000000000000000, 0.3546048870425426158, 0.9350162426854120579 ) ) ;
#8965 = CARTESIAN_POINT ( 'NONE',  ( -332.3517673607765914, -123.5000000000000284, 0.000000000000000000 ) ) ;
#8964 = DIRECTION ( 'NONE',  ( -0.000000000000000000, -0.8854560256532126861, -0.4647231720437631775 ) ) ;
#8966 = ADVANCED_FACE ( 'NONE', ( #45382 ), #13564, .F. ) ;
#8967 = VERTEX_POINT ( 'NONE', #18299 ) ;
#8968 = VECTOR ( 'NONE', #12687, 999.9999999999998863 ) ;
#8969 = DIRECTION ( 'NONE',  ( -1.000000000000000000, 0.000000000000000000, 0.000000000000000000 ) ) ;
#8970 = CARTESIAN_POINT ( 'NONE',  ( 73.66680038934278230, -189.7472609257535510, -26.55884942729568365 ) ) ;
#8971 = FACE_OUTER_BOUND ( 'NONE', #39132, .T. ) ;
#8972 = ORIENTED_EDGE ( 'NONE', *, *, #49555, .F. ) ;
#8973 = CARTESIAN_POINT ( 'NONE',  ( -150.5215542367829471, -175.3837268820161057, -72.19655804061974891 ) ) ;
#8974 = CARTESIAN_POINT ( 'NONE',  ( 5.139251539934009294, -183.6283474603465606, 111.8087531435657951 ) ) ;
#8975 = DIRECTION ( 'NONE',  ( 0.9564009842765244240, 0.000000000000000000, -0.2920567706369695538 ) ) ;
#8976 = ORIENTED_EDGE ( 'NONE', *, *, #42064, .T. ) ;
#8977 = DIRECTION ( 'NONE',  ( -0.000000000000000000, 1.000000000000000000, -0.000000000000000000 ) ) ;
#8978 = ADVANCED_FACE ( 'NONE', ( #9892 ), #2264, .T. ) ;
#8979 = DIRECTION ( 'NONE',  ( -0.000000000000000000, 1.000000000000000000, -0.000000000000000000 ) ) ;
#8980 = ORIENTED_EDGE ( 'NONE', *, *, #21333, .F. ) ;
#8981 = VECTOR ( 'NONE', #29780, 1000.000000000000000 ) ;
#8982 = AXIS2_PLACEMENT_3D ( 'NONE', #2965, #7685, #50553 ) ;
#8983 = CARTESIAN_POINT ( 'NONE',  ( -27.36201831380532923, -175.3837268820161057, -122.1886788576022411 ) ) ;
#8984 = CARTESIAN_POINT ( 'NONE',  ( -48.47912675150885065, -175.3837268820161057, 6.938893903907228378E-15 ) ) ;
#8985 = AXIS2_PLACEMENT_3D ( 'NONE', #30316, #46623, #7182 ) ;
#8986 = EDGE_CURVE ( 'NONE', #28248, #19289, #34617, .T. ) ;
#8987 = CARTESIAN_POINT ( 'NONE',  ( -339.1964088526558498, -150.4759391377560576, -52.47426709956116042 ) ) ;
#8988 = PLANE ( 'NONE',  #17210 ) ;
#8989 = DIRECTION ( 'NONE',  ( -0.000000000000000000, 0.5680647467311540355, -0.8229838658936575735 ) ) ;
#8990 = EDGE_CURVE ( 'NONE', #44410, #1407, #41330, .T. ) ;
#8991 = EDGE_CURVE ( 'NONE', #28728, #41453, #22504, .T. ) ;
#8992 = EDGE_CURVE ( 'NONE', #1774, #14215, #40500, .T. ) ;
#8993 = FACE_OUTER_BOUND ( 'NONE', #1890, .T. ) ;
#8994 = AXIS2_PLACEMENT_3D ( 'NONE', #51311, #31063, #15061 ) ;
#8995 = AXIS2_PLACEMENT_3D ( 'NONE', #21884, #38420, #46071 ) ;
#8996 = DIRECTION ( 'NONE',  ( 0.000000000000000000, 1.000000000000000000, 0.000000000000000000 ) ) ;
#8997 = CARTESIAN_POINT ( 'NONE',  ( -49.45768324380835423, -193.5000000000000000, 0.2059786187410958813 ) ) ;
#8999 = VERTEX_POINT ( 'NONE', #37738 ) ;
#8998 = CARTESIAN_POINT ( 'NONE',  ( 0.000000000000000000, -53.50000000000000000, 0.000000000000000000 ) ) ;
#9000 = AXIS2_PLACEMENT_3D ( 'NONE', #2677, #43412, #18462 ) ;
#9001 = VECTOR ( 'NONE', #3229, 1000.000000000000114 ) ;
#9002 = VERTEX_POINT ( 'NONE', #41677 ) ;
#9003 = DIRECTION ( 'NONE',  ( 1.000000000000000000, -0.000000000000000000, -0.000000000000000000 ) ) ;
#9004 = AXIS2_PLACEMENT_3D ( 'NONE', #27152, #51352, #20051 ) ;
#9005 = VECTOR ( 'NONE', #5030, 1000.000000000000114 ) ;
#9006 = CARTESIAN_POINT ( 'NONE',  ( -332.3517673607765914, -84.94915232962709695, -45.97643030831888922 ) ) ;
#9007 = VERTEX_POINT ( 'NONE', #46161 ) ;
#9008 = VERTEX_POINT ( 'NONE', #45899 ) ;
#9009 = ADVANCED_FACE ( 'NONE', ( #5704 ), #45641, .F. ) ;
#9010 = EDGE_LOOP ( 'NONE', ( #29529, #41628, #34097, #18581 ) ) ;
#9011 = DIRECTION ( 'NONE',  ( 0.000000000000000000, 0.000000000000000000, -1.000000000000000000 ) ) ;
#9012 = EDGE_CURVE ( 'NONE', #31844, #17957, #31275, .T. ) ;
#9013 = CARTESIAN_POINT ( 'NONE',  ( -330.4913330509368166, -137.1341532842531876, -57.40522506028080585 ) ) ;
#9014 = CYLINDRICAL_SURFACE ( 'NONE', #50986, 125.0000000000000000 ) ;
#9015 = ORIENTED_EDGE ( 'NONE', *, *, #48758, .T. ) ;
#9016 = ORIENTED_EDGE ( 'NONE', *, *, #19984, .T. ) ;
#9017 = EDGE_CURVE ( 'NONE', #22760, #4153, #37995, .T. ) ;
#9018 = CARTESIAN_POINT ( 'NONE',  ( -169.0136227435421006, -175.3837268820161057, -33.11246405730811659 ) ) ;
#9019 = AXIS2_PLACEMENT_3D ( 'NONE', #30402, #43540, #46452 ) ;
#9021 = ORIENTED_EDGE ( 'NONE', *, *, #22438, .F. ) ;
#9020 = PLANE ( 'NONE',  #33344 ) ;
#9022 = AXIS2_PLACEMENT_3D ( 'NONE', #32042, #40441, #3672 ) ;
#9023 = CARTESIAN_POINT ( 'NONE',  ( 26.52087324849106054, -198.5000000000000000, -70.00000000000002842 ) ) ;
#9024 = ORIENTED_EDGE ( 'NONE', *, *, #2553, .F. ) ;
#9025 = CARTESIAN_POINT ( 'NONE',  ( 46.40005841627163363, -183.6283474603465606, 81.38144888055276738 ) ) ;
#9026 = AXIS2_PLACEMENT_3D ( 'NONE', #9204, #17094, #40987 ) ;
#9027 = ORIENTED_EDGE ( 'NONE', *, *, #34491, .T. ) ;
#9028 = FACE_OUTER_BOUND ( 'NONE', #35033, .T. ) ;
#9029 = CARTESIAN_POINT ( 'NONE',  ( -332.3517673607765914, -140.4009141470556870, -57.57047073799078873 ) ) ;
#9030 = LINE ( 'NONE', #13484, #42532 ) ;
#9031 = ORIENTED_EDGE ( 'NONE', *, *, #18683, .T. ) ;
#9032 = AXIS2_PLACEMENT_3D ( 'NONE', #32661, #46428, #50627 ) ;
#9033 = EDGE_LOOP ( 'NONE', ( #34418, #30140, #44134, #8555 ) ) ;
#9034 = CARTESIAN_POINT ( 'NONE',  ( 55.03325008324586776, -193.5000000000000000, -70.07273251429357686 ) ) ;
#9035 = FACE_OUTER_BOUND ( 'NONE', #46857, .T. ) ;
#9036 = VECTOR ( 'NONE', #49163, 1000.000000000000000 ) ;
#9037 = ORIENTED_EDGE ( 'NONE', *, *, #2923, .F. ) ;
#9038 = CARTESIAN_POINT ( 'NONE',  ( -48.47912675150885065, -189.7472609257535510, 6.938893903907228378E-15 ) ) ;
#9039 = VECTOR ( 'NONE', #12513, 1000.000000000000000 ) ;
#9040 = CARTESIAN_POINT ( 'NONE',  ( -19.28375372365792728, -175.3837268820161057, 121.5427093402341541 ) ) ;
#9041 = EDGE_LOOP ( 'NONE', ( #31740, #27869, #4933, #6970 ) ) ;
#9042 = LINE ( 'NONE', #21649, #40138 ) ;
#9043 = AXIS2_PLACEMENT_3D ( 'NONE', #49457, #9492, #25512 ) ;
#9044 = DIRECTION ( 'NONE',  ( 1.000000000000000000, -0.000000000000000000, -0.000000000000000000 ) ) ;
#9045 = CIRCLE ( 'NONE', #26634, 125.0000000000000000 ) ;
#9046 = ORIENTED_EDGE ( 'NONE', *, *, #22833, .F. ) ;
#9047 = CARTESIAN_POINT ( 'NONE',  ( 8.750818922897904528, -193.5000000000000000, -111.1293539894138434 ) ) ;
#9048 = ORIENTED_EDGE ( 'NONE', *, *, #42671, .F. ) ;
#9049 = DIRECTION ( 'NONE',  ( -0.000000000000000000, 1.000000000000000000, -0.000000000000000000 ) ) ;
#9050 = CARTESIAN_POINT ( 'NONE',  ( -141.2664123866436796, -175.3837268820161057, -83.75869879877495805 ) ) ;
#9051 = ORIENTED_EDGE ( 'NONE', *, *, #47814, .F. ) ;
#9052 = DIRECTION ( 'NONE',  ( 0.000000000000000000, -1.000000000000000000, -0.000000000000000000 ) ) ;
#9053 = CARTESIAN_POINT ( 'NONE',  ( -118.9967449635792320, -189.7472609257535510, -103.2098131075562009 ) ) ;
#9054 = CARTESIAN_POINT ( 'NONE',  ( -336.3521761649654422, -142.8954717479169574, 55.74477592174805096 ) ) ;
#9055 = ADVANCED_FACE ( 'NONE', ( #21454 ), #22224, .T. ) ;
#9056 = ADVANCED_FACE ( 'NONE', ( #5436 ), #38517, .T. ) ;
#9057 = CARTESIAN_POINT ( 'NONE',  ( -85.14888725715766782, -189.7472609257535510, 119.5003291395398719 ) ) ;
#9058 = EDGE_LOOP ( 'NONE', ( #8021, #51340, #7415, #29351 ) ) ;
#9059 = CARTESIAN_POINT ( 'NONE',  ( -144.0067397530739584, -183.6283474603465606, -80.61932246194587037 ) ) ;
#9060 = ORIENTED_EDGE ( 'NONE', *, *, #16647, .F. ) ;
#9061 = ORIENTED_EDGE ( 'NONE', *, *, #16681, .F. ) ;
#9062 = VECTOR ( 'NONE', #14079, 1000.000000000000114 ) ;
#9063 = AXIS2_PLACEMENT_3D ( 'NONE', #48857, #52030, #3924 ) ;
#9064 = DIRECTION ( 'NONE',  ( -0.05924062789370006937, 0.000000000000000000, -0.9982437317643222396 ) ) ;
#9066 = ORIENTED_EDGE ( 'NONE', *, *, #23675, .F. ) ;
#9065 = DIRECTION ( 'NONE',  ( 0.000000000000000000, -0.1205366802553303196, -0.9927088740980530845 ) ) ;
#9067 = CIRCLE ( 'NONE', #25010, 125.0000000000000000 ) ;
#9068 = ORIENTED_EDGE ( 'NONE', *, *, #31996, .T. ) ;
#9069 = CARTESIAN_POINT ( 'NONE',  ( -332.3517673607765914, -66.84438072661991725, -16.67542351306652648 ) ) ;
#9070 = CARTESIAN_POINT ( 'NONE',  ( -305.0000000000000568, -183.4777928329299357, 1.632288850093980725 ) ) ;
#9071 = DIRECTION ( 'NONE',  ( 0.000000000000000000, -0.2393156642875448881, 0.9709418174260553425 ) ) ;
#9072 = AXIS2_PLACEMENT_3D ( 'NONE', #47976, #11958, #44025 ) ;
#9073 = EDGE_LOOP ( 'NONE', ( #14394, #48890, #9761, #23314 ) ) ;
#9074 = PLANE ( 'NONE',  #28102 ) ;
#9075 = EDGE_CURVE ( 'NONE', #46251, #51992, #14349, .T. ) ;
#9076 = EDGE_LOOP ( 'NONE', ( #23271, #45182, #36020, #9292 ) ) ;
#9077 = DIRECTION ( 'NONE',  ( 0.000000000000000000, 0.000000000000000000, 1.000000000000000000 ) ) ;
#9078 = PLANE ( 'NONE',  #44286 ) ;
#9079 = CARTESIAN_POINT ( 'NONE',  ( -48.47912675150885065, -188.5000000000000284, 13.99999999999999645 ) ) ;
#9080 = CARTESIAN_POINT ( 'NONE',  ( 33.75048693540708911, -175.3837268820161057, 94.14505102712816154 ) ) ;
#9081 = ORIENTED_EDGE ( 'NONE', *, *, #38469, .F. ) ;
#9082 = EDGE_LOOP ( 'NONE', ( #42264, #16111, #21183, #1903 ) ) ;
#9083 = ADVANCED_FACE ( 'NONE', ( #6476 ), #37479, .T. ) ;
#9084 = VERTEX_POINT ( 'NONE', #17531 ) ;
#9085 = VECTOR ( 'NONE', #22332, 999.9999999999998863 ) ;
#9086 = DIRECTION ( 'NONE',  ( 0.6528221181905174975, 0.000000000000000000, 0.7575112421616236880 ) ) ;
#9087 = DIRECTION ( 'NONE',  ( 0.4031234292879792847, 0.000000000000000000, -0.9151456172430153524 ) ) ;
#9088 = DIRECTION ( 'NONE',  ( 0.000000000000000000, -0.000000000000000000, -1.000000000000000000 ) ) ;
#9089 = FACE_BOUND ( 'NONE', #14504, .T. ) ;
#9090 = CARTESIAN_POINT ( 'NONE',  ( -330.4913330509368166, -78.92247586331968989, 40.16023333900940173 ) ) ;
#9091 = ORIENTED_EDGE ( 'NONE', *, *, #49922, .T. ) ;
#9092 = VERTEX_POINT ( 'NONE', #47185 ) ;
#9094 = ORIENTED_EDGE ( 'NONE', *, *, #17974, .T. ) ;
#9093 = DIRECTION ( 'NONE',  ( -0.9473263538541946138, 0.000000000000000000, 0.3202698538628279690 ) ) ;
#9095 = DIRECTION ( 'NONE',  ( -0.000000000000000000, 1.000000000000000000, -0.000000000000000000 ) ) ;
#9096 = ORIENTED_EDGE ( 'NONE', *, *, #37233, .F. ) ;
#9097 = CIRCLE ( 'NONE', #25042, 125.0000000000000000 ) ;
#9099 = AXIS2_PLACEMENT_3D ( 'NONE', #40467, #20504, #12616 ) ;
#9098 = DIRECTION ( 'NONE',  ( -0.000000000000000000, 1.000000000000000000, -0.000000000000000000 ) ) ;
#9100 = CARTESIAN_POINT ( 'NONE',  ( -336.3521761649654422, -123.5000000000000284, 0.000000000000000000 ) ) ;
#9101 = VECTOR ( 'NONE', #16897, 1000.000000000000000 ) ;
#9102 = LINE ( 'NONE', #41145, #43027 ) ;
#9103 = DIRECTION ( 'NONE',  ( 0.000000000000000000, 0.000000000000000000, 1.000000000000000000 ) ) ;
#9104 = CARTESIAN_POINT ( 'NONE',  ( -165.5546359831674295, -193.5000000000000000, 43.79868877201493405 ) ) ;
#9105 = ORIENTED_EDGE ( 'NONE', *, *, #27779, .T. ) ;
#9106 = CARTESIAN_POINT ( 'NONE',  ( 40.26790151320557953, -183.6283474603465606, -86.60307583628355133 ) ) ;
#9107 = ORIENTED_EDGE ( 'NONE', *, *, #25133, .T. ) ;
#9108 = EDGE_CURVE ( 'NONE', #15949, #33758, #35771, .T. ) ;
#9109 = ORIENTED_EDGE ( 'NONE', *, *, #9328, .T. ) ;
#9110 = PLANE ( 'NONE',  #27086 ) ;
#9111 = AXIS2_PLACEMENT_3D ( 'NONE', #17363, #33383, #2357 ) ;
#9112 = DIRECTION ( 'NONE',  ( 0.000000000000000000, -0.8854560256532093554, 0.4647231720437695057 ) ) ;
#9113 = DIRECTION ( 'NONE',  ( 0.000000000000000000, 1.000000000000000000, -6.938893903907229364E-16 ) ) ;
#9114 = PLANE ( 'NONE',  #23839 ) ;
#9115 = CYLINDRICAL_SURFACE ( 'NONE', #35435, 125.0000000000000000 ) ;
#9116 = EDGE_CURVE ( 'NONE', #32483, #31844, #35861, .T. ) ;
#9117 = EDGE_LOOP ( 'NONE', ( #43077, #31071, #6107, #28256 ) ) ;
#9118 = DIRECTION ( 'NONE',  ( 0.000000000000000000, 0.000000000000000000, 1.000000000000000000 ) ) ;
#9119 = CARTESIAN_POINT ( 'NONE',  ( 29.27398957514435196, -183.6283474603465606, -97.87467957287998388 ) ) ;
#9120 = AXIS2_PLACEMENT_3D ( 'NONE', #28850, #44903, #24931 ) ;
#9121 = CARTESIAN_POINT ( 'NONE',  ( -336.3521761649654422, -182.5000000000000568, 1.632288850093980725 ) ) ;
#9122 = FACE_BOUND ( 'NONE', #38135, .T. ) ;
#9123 = ORIENTED_EDGE ( 'NONE', *, *, #18876, .T. ) ;
#9124 = EDGE_CURVE ( 'NONE', #35572, #24400, #23996, .T. ) ;
#9125 = CYLINDRICAL_SURFACE ( 'NONE', #38199, 125.0000000000000000 ) ;
#9126 = ORIENTED_EDGE ( 'NONE', *, *, #41799, .T. ) ;
#9127 = FACE_OUTER_BOUND ( 'NONE', #51157, .T. ) ;
#9128 = ORIENTED_EDGE ( 'NONE', *, *, #14380, .T. ) ;
#9129 = CARTESIAN_POINT ( 'NONE',  ( 0.000000000000000000, -175.7419055135395922, -27.41866715058203852 ) ) ;
#9130 = ORIENTED_EDGE ( 'NONE', *, *, #6366, .T. ) ;
#9131 = DIRECTION ( 'NONE',  ( -0.000000000000000000, 1.000000000000000000, 0.000000000000000000 ) ) ;
#9132 = CARTESIAN_POINT ( 'NONE',  ( -332.3517673607765914, -125.1322888500942270, -59.97779283292990016 ) ) ;
#9133 = VECTOR ( 'NONE', #7990, 1000.000000000000000 ) ;
#9134 = AXIS2_PLACEMENT_3D ( 'NONE', #47023, #14451, #14197 ) ;
#9135 = CARTESIAN_POINT ( 'NONE',  ( -339.1964088526558498, -123.5000000000000284, 0.000000000000000000 ) ) ;
#9137 = EDGE_LOOP ( 'NONE', ( #25847, #16592, #36005, #15858 ) ) ;
#9136 = PLANE ( 'NONE',  #24560 ) ;
#9138 = EDGE_CURVE ( 'NONE', #49593, #24719, #30892, .T. ) ;
#9139 = CIRCLE ( 'NONE', #22574, 125.0000000000000000 ) ;
#9140 = PLANE ( 'NONE',  #39 ) ;
#9141 = ORIENTED_EDGE ( 'NONE', *, *, #2243, .F. ) ;
#9142 = ORIENTED_EDGE ( 'NONE', *, *, #9960, .F. ) ;
#9143 = EDGE_LOOP ( 'NONE', ( #19156, #42009, #40980, #2493 ) ) ;
#9144 = CARTESIAN_POINT ( 'NONE',  ( 64.86941505090324256, -193.5000000000000000, -50.28156562190505241 ) ) ;
#9145 = AXIS2_PLACEMENT_3D ( 'NONE', #49862, #13067, #45665 ) ;
#9146 = CARTESIAN_POINT ( 'NONE',  ( -88.78924379339714790, -193.5000000000000000, -118.3219948448692520 ) ) ;
#9147 = ORIENTED_EDGE ( 'NONE', *, *, #38153, .F. ) ;
#9148 = DIRECTION ( 'NONE',  ( -0.000000000000000000, 1.000000000000000000, -0.000000000000000000 ) ) ;
#9149 = DIRECTION ( 'NONE',  ( 1.000000000000000000, 0.000000000000000000, -0.000000000000000000 ) ) ;
#9150 = LINE ( 'NONE', #29882, #30521 ) ;
#9151 = ORIENTED_EDGE ( 'NONE', *, *, #5451, .T. ) ;
#9152 = AXIS2_PLACEMENT_3D ( 'NONE', #40108, #45114, #16742 ) ;
#9153 = LINE ( 'NONE', #21235, #35116 ) ;
#9154 = DIRECTION ( 'NONE',  ( -0.000000000000000000, 1.000000000000000000, -0.000000000000000000 ) ) ;
#9155 = ORIENTED_EDGE ( 'NONE', *, *, #8990, .T. ) ;
#9158 = ORIENTED_EDGE ( 'NONE', *, *, #12826, .T. ) ;
#9157 = CARTESIAN_POINT ( 'NONE',  ( -73.94077438226447896, -193.5000000000000000, 122.3793467049372481 ) ) ;
#9156 = DIRECTION ( 'NONE',  ( 0.000000000000000000, 0.000000000000000000, -1.000000000000000000 ) ) ;
#9159 = ORIENTED_EDGE ( 'NONE', *, *, #32175, .T. ) ;
#9160 = CARTESIAN_POINT ( 'NONE',  ( 60.58466639580034041, -189.7472609257535510, -61.07445476073405644 ) ) ;
#9161 = VERTEX_POINT ( 'NONE', #23004 ) ;
#9162 = CARTESIAN_POINT ( 'NONE',  ( -46.00000000000000711, 20.00000000000000000, -46.00000000000000000 ) ) ;
#9163 = ADVANCED_FACE ( 'NONE', ( #27711 ), #27186, .T. ) ;
#9164 = EDGE_LOOP ( 'NONE', ( #48066, #26868, #5553, #40969 ) ) ;
#9165 = EDGE_CURVE ( 'NONE', #33115, #49764, #19068, .T. ) ;
#9166 = DIRECTION ( 'NONE',  ( 0.000000000000000000, 0.000000000000000000, -1.000000000000000000 ) ) ;
#9167 = CARTESIAN_POINT ( 'NONE',  ( -170.9669310976187830, -189.7472609257535510, -24.93467037017130394 ) ) ;
#9168 = EDGE_LOOP ( 'NONE', ( #49934, #22485, #7141, #7027 ) ) ;
#9169 = CARTESIAN_POINT ( 'NONE',  ( -48.47912675150885065, -213.5000000000000000, 6.938893903907228378E-15 ) ) ;
#9170 = EDGE_LOOP ( 'NONE', ( #11886, #947, #34394, #15486 ) ) ;
#9171 = EDGE_CURVE ( 'NONE', #9853, #20140, #23520, .T. ) ;
#9172 = EDGE_LOOP ( 'NONE', ( #44787, #25247, #26016, #19974 ) ) ;
#9173 = DIRECTION ( 'NONE',  ( -0.000000000000000000, 1.000000000000000000, -0.000000000000000000 ) ) ;
#9174 = DIRECTION ( 'NONE',  ( 0.000000000000000000, 1.000000000000000000, 0.000000000000000000 ) ) ;
#9175 = AXIS2_PLACEMENT_3D ( 'NONE', #2346, #42266, #34396 ) ;
#9176 = FACE_OUTER_BOUND ( 'NONE', #49360, .T. ) ;
#9177 = FACE_OUTER_BOUND ( 'NONE', #6768, .T. ) ;
#9178 = EDGE_LOOP ( 'NONE', ( #22589, #10495, #21375, #29223 ) ) ;
#9179 = VECTOR ( 'NONE', #4413, 1000.000000000000000 ) ;
#9180 = DIRECTION ( 'NONE',  ( 1.000000000000000000, -0.000000000000000000, -0.000000000000000000 ) ) ;
#9181 = APPLICATION_PROTOCOL_DEFINITION ( 'draft international standard', 'automotive_design', 1998, #21625 ) ;
#9182 = CARTESIAN_POINT ( 'NONE',  ( -47.92047998570520662, -193.5000000000000000, 0.8294056854502119824 ) ) ;
#9183 = DIRECTION ( 'NONE',  ( 0.000000000000000000, -0.3546048870425235200, 0.9350162426854194964 ) ) ;
#9184 = EDGE_CURVE ( 'NONE', #21155, #40815, #49192, .T. ) ;
#9185 = DIRECTION ( 'NONE',  ( 0.000000000000000000, 0.1205366802553199251, -0.9927088740980544168 ) ) ;
#9186 = LINE ( 'NONE', #25209, #44119 ) ;
#9187 = ADVANCED_FACE ( 'NONE', ( #46938 ), #39290, .F. ) ;
#9188 = EDGE_CURVE ( 'NONE', #34792, #18880, #23274, .T. ) ;
#9189 = CARTESIAN_POINT ( 'NONE',  ( -332.3517673607765914, -114.6500883362968892, 59.34373651485599055 ) ) ;
#9190 = ORIENTED_EDGE ( 'NONE', *, *, #9604, .T. ) ;
#9191 = EDGE_CURVE ( 'NONE', #9672, #34082, #8062, .T. ) ;
#9192 = ADVANCED_FACE ( 'NONE', ( #11419 ), #39014, .F. ) ;
#9193 = FACE_OUTER_BOUND ( 'NONE', #5403, .T. ) ;
#9194 = CARTESIAN_POINT ( 'NONE',  ( 28.02885774092382221, -175.3837268820161057, 98.85104101073332572 ) ) ;
#9195 = ORIENTED_EDGE ( 'NONE', *, *, #32175, .F. ) ;
#9196 = CARTESIAN_POINT ( 'NONE',  ( -91.84482189527184914, -189.7472609257535510, -117.2365833888816837 ) ) ;
#9197 = VERTEX_POINT ( 'NONE', #50872 ) ;
#9198 = VECTOR ( 'NONE', #39001, 1000.000000000000000 ) ;
#9199 = PLANE ( 'NONE',  #37677 ) ;
#9200 = DIRECTION ( 'NONE',  ( 0.2348860457809911206, 0.000000000000000000, -0.9720229140804089729 ) ) ;
#9201 = LINE ( 'NONE', #33096, #50601 ) ;
#9202 = DIRECTION ( 'NONE',  ( 0.000000000000000000, 0.000000000000000000, -1.000000000000000000 ) ) ;
#9203 = VERTEX_POINT ( 'NONE', #27456 ) ;
#9204 = CARTESIAN_POINT ( 'NONE',  ( -336.3521761649654422, -123.5000000000000284, 0.000000000000000000 ) ) ;
#9205 = LINE ( 'NONE', #16576, #37776 ) ;
#9206 = CARTESIAN_POINT ( 'NONE',  ( 0.000000000000000000, 55.00653718120851465, -11.89184658936181727 ) ) ;
#9207 = ORIENTED_EDGE ( 'NONE', *, *, #17246, .T. ) ;
#9208 = DIRECTION ( 'NONE',  ( -1.000000000000000000, 0.000000000000000000, 0.000000000000000000 ) ) ;
#9209 = AXIS2_PLACEMENT_3D ( 'NONE', #19341, #15403, #43512 ) ;
#9210 = ORIENTED_EDGE ( 'NONE', *, *, #26761, .T. ) ;
#9211 = CARTESIAN_POINT ( 'NONE',  ( -48.47912675150885065, -189.7472609257535510, 6.938893903907228378E-15 ) ) ;
#9212 = AXIS2_PLACEMENT_3D ( 'NONE', #2426, #30523, #22394 ) ;
#9213 = CARTESIAN_POINT ( 'NONE',  ( 53.56330073376472001, -193.5000000000000000, 72.19655804062048787 ) ) ;
#9214 = CARTESIAN_POINT ( 'NONE',  ( -339.1964088526558498, -103.0458197858333165, -55.34326076196084188 ) ) ;
#9215 = ORIENTED_EDGE ( 'NONE', *, *, #2243, .T. ) ;
#9218 = ORIENTED_EDGE ( 'NONE', *, *, #37420, .T. ) ;
#9217 = CARTESIAN_POINT ( 'NONE',  ( -48.02249751411513756, -177.1207230881787780, -0.8896570909947397743 ) ) ;
#9216 = CARTESIAN_POINT ( 'NONE',  ( 0.000000000000000000, -116.3883358649353141, 58.56982357178514320 ) ) ;
#9219 = DIRECTION ( 'NONE',  ( 0.000000000000000000, 0.000000000000000000, 1.000000000000000000 ) ) ;
#9220 = ORIENTED_EDGE ( 'NONE', *, *, #39204, .F. ) ;
#9221 = DIRECTION ( 'NONE',  ( -0.5586467658036415873, 0.000000000000000000, -0.8294056854502090959 ) ) ;
#9222 = DIRECTION ( 'NONE',  ( -0.000000000000000000, 0.9350162426854181641, 0.3546048870425267951 ) ) ;
#9223 = EDGE_LOOP ( 'NONE', ( #35980, #45338, #40807, #19531 ) ) ;
#9224 = EDGE_CURVE ( 'NONE', #40095, #43678, #43498, .T. ) ;
#9225 = EDGE_CURVE ( 'NONE', #38326, #19688, #41626, .T. ) ;
#9226 = EDGE_CURVE ( 'NONE', #14956, #47094, #37428, .T. ) ;
#9227 = DIRECTION ( 'NONE',  ( 0.000000000000000000, -1.000000000000000000, 0.000000000000000000 ) ) ;
#9230 = ORIENTED_EDGE ( 'NONE', *, *, #2705, .F. ) ;
#9229 = LINE ( 'NONE', #28131, #11373 ) ;
#9228 = DIRECTION ( 'NONE',  ( -0.000000000000000000, 1.000000000000000000, -0.000000000000000000 ) ) ;
#9231 = ORIENTED_EDGE ( 'NONE', *, *, #30769, .F. ) ;
#9232 = AXIS2_PLACEMENT_3D ( 'NONE', #30387, #30918, #46440 ) ;
#9233 = CARTESIAN_POINT ( 'NONE',  ( -119.6907301311197216, -177.1207230881787780, 101.5140743725400370 ) ) ;
#9234 = LINE ( 'NONE', #21585, #19443 ) ;
#9235 = CARTESIAN_POINT ( 'NONE',  ( 60.00000000000001421, -113.5000000000000142, 39.99999999999998579 ) ) ;
#9236 = ORIENTED_EDGE ( 'NONE', *, *, #24401, .T. ) ;
#9237 = LINE ( 'NONE', #49695, #27481 ) ;
#9238 = DIRECTION ( 'NONE',  ( -0.000000000000000000, 1.000000000000000000, -0.000000000000000000 ) ) ;
#9239 = ADVANCED_FACE ( 'NONE', ( #47709 ), #11687, .T. ) ;
#9240 = CYLINDRICAL_SURFACE ( 'NONE', #4164, 125.0000000000000000 ) ;
#9241 = FACE_OUTER_BOUND ( 'NONE', #27295, .T. ) ;
#9242 = VERTEX_POINT ( 'NONE', #39783 ) ;
#9243 = ADVANCED_FACE ( 'NONE', ( #6726 ), #38756, .T. ) ;
#9244 = CARTESIAN_POINT ( 'NONE',  ( -48.47912675150885065, -187.5000000000000284, 6.938893903907228378E-15 ) ) ;
#9245 = CARTESIAN_POINT ( 'NONE',  ( 76.21810084846656252, -193.5000000000000000, -8.694908215727984668 ) ) ;
#9246 = EDGE_CURVE ( 'NONE', #6229, #27746, #12565, .T. ) ;
#9247 = DIRECTION ( 'NONE',  ( 0.000000000000000000, 1.000000000000000000, 0.000000000000000000 ) ) ;
#9248 = VERTEX_POINT ( 'NONE', #21238 ) ;
#9249 = EDGE_CURVE ( 'NONE', #50694, #13737, #5218, .T. ) ;
#9250 = AXIS2_PLACEMENT_3D ( 'NONE', #28105, #12608, #5006 ) ;
#9251 = CARTESIAN_POINT ( 'NONE',  ( -305.0000000000000568, -65.12585595286518014, 13.87297036558326013 ) ) ;
#9252 = FACE_OUTER_BOUND ( 'NONE', #50515, .T. ) ;
#9253 = ADVANCED_FACE ( 'NONE', ( #24648 ), #48588, .F. ) ;
#9254 = FACE_OUTER_BOUND ( 'NONE', #33706, .T. ) ;
#9255 = DIRECTION ( 'NONE',  ( -0.000000000000000000, -0.8229838658936516893, 0.5680647467311626952 ) ) ;
#9256 = LINE ( 'NONE', #836, #22924 ) ;
#9257 = CARTESIAN_POINT ( 'NONE',  ( -49.46816693883101834, -189.7472609257535510, 0.1476465640024780257 ) ) ;
#9258 = PLANE ( 'NONE',  #12801 ) ;
#9260 = ORIENTED_EDGE ( 'NONE', *, *, #10815, .F. ) ;
#9259 = LINE ( 'NONE', #29469, #44681 ) ;
#9261 = ORIENTED_EDGE ( 'NONE', *, *, #40126, .F. ) ;
#9262 = PLANE ( 'NONE',  #49283 ) ;
#9263 = EDGE_CURVE ( 'NONE', #12238, #46358, #20711, .T. ) ;
#9264 = VECTOR ( 'NONE', #42937, 1000.000000000000114 ) ;
#9265 = DIRECTION ( 'NONE',  ( 0.000000000000000000, 0.000000000000000000, -1.000000000000000000 ) ) ;
#9267 = EDGE_LOOP ( 'NONE', ( #47806, #33139, #33785, #7261 ) ) ;
#9266 = DIRECTION ( 'NONE',  ( 0.000000000000000000, -0.000000000000000000, -1.000000000000000000 ) ) ;
#9268 = EDGE_LOOP ( 'NONE', ( #38964, #27022 ) ) ;
#9269 = EDGE_LOOP ( 'NONE', ( #21273, #37369, #37330, #46943 ) ) ;
#9270 = DIRECTION ( 'NONE',  ( 0.000000000000000000, 0.000000000000000000, -1.000000000000000000 ) ) ;
#9271 = DIRECTION ( 'NONE',  ( -0.000000000000000000, 1.000000000000000000, -0.000000000000000000 ) ) ;
#9272 = DIRECTION ( 'NONE',  ( 0.000000000000000000, 0.000000000000000000, 1.000000000000000000 ) ) ;
#9273 = ORIENTED_EDGE ( 'NONE', *, *, #28374, .F. ) ;
#9274 = EDGE_CURVE ( 'NONE', #7810, #44829, #8617, .T. ) ;
#9275 = DIRECTION ( 'NONE',  ( -0.000000000000000000, -0.7485107481710953081, 0.6631226582408016323 ) ) ;
#9277 = VERTEX_POINT ( 'NONE', #12814 ) ;
#9276 = CARTESIAN_POINT ( 'NONE',  ( -47.64924157374594671, -189.7472609257535510, 123.9972451320097377 ) ) ;
#9278 = AXIS2_PLACEMENT_3D ( 'NONE', #46431, #10159, #37500 ) ;
#9279 = LINE ( 'NONE', #8482, #33152 ) ;
#9280 = ORIENTED_EDGE ( 'NONE', *, *, #20182, .T. ) ;
#9281 = FACE_OUTER_BOUND ( 'NONE', #17422, .T. ) ;
#9282 = EDGE_LOOP ( 'NONE', ( #36969, #14937, #10155, #15798 ) ) ;
#9283 = ADVANCED_FACE ( 'NONE', ( #28839 ), #42428, .T. ) ;
#9284 = EDGE_CURVE ( 'NONE', #42609, #17165, #39924, .T. ) ;
#9285 = ADVANCED_FACE ( 'NONE', ( #44891 ), #2237, .T. ) ;
#9286 = ADVANCED_FACE ( 'NONE', ( #33323 ), #36998, .F. ) ;
#9287 = DIRECTION ( 'NONE',  ( 0.000000000000000000, 1.000000000000000000, 0.000000000000000000 ) ) ;
#9288 = CARTESIAN_POINT ( 'NONE',  ( -330.4913330509368166, -66.09477493971897388, 13.63415328425216622 ) ) ;
#9289 = PLANE ( 'NONE',  #5602 ) ;
#9290 = ADVANCED_FACE ( 'NONE', ( #14325 ), #30338, .F. ) ;
#9291 = ORIENTED_EDGE ( 'NONE', *, *, #47852, .T. ) ;
#9292 = ORIENTED_EDGE ( 'NONE', *, *, #41933, .T. ) ;
#9293 = DIRECTION ( 'NONE',  ( 0.8455960035018311727, 0.000000000000000000, -0.5338233779647826305 ) ) ;
#9294 = LINE ( 'NONE', #21644, #41806 ) ;
#9295 = ORIENTED_EDGE ( 'NONE', *, *, #41824, .T. ) ;
#9296 = EDGE_CURVE ( 'NONE', #37279, #39766, #18278, .T. ) ;
#9297 = DIRECTION ( 'NONE',  ( -0.000000000000000000, 1.000000000000000000, -0.000000000000000000 ) ) ;
#9298 = VERTEX_POINT ( 'NONE', #49366 ) ;
#9299 = CARTESIAN_POINT ( 'NONE',  ( -332.3517673607765914, -162.0508476703726330, 45.97643030831915212 ) ) ;
#9300 = EDGE_CURVE ( 'NONE', #29184, #29691, #464, .T. ) ;
#9301 = DIRECTION ( 'NONE',  ( -0.000000000000000000, -0.6631226582407885317, 0.7485107481711069655 ) ) ;
#9302 = AXIS2_PLACEMENT_3D ( 'NONE', #17691, #34470, #46069 ) ;
#9303 = EDGE_CURVE ( 'NONE', #41107, #51365, #46390, .T. ) ;
#9304 = VECTOR ( 'NONE', #23147, 1000.000000000000000 ) ;
#9305 = ORIENTED_EDGE ( 'NONE', *, *, #37685, .T. ) ;
#9306 = CARTESIAN_POINT ( 'NONE',  ( 51.05451324771861721, -183.6283474603465606, 75.61781872352699452 ) ) ;
#9307 = VERTEX_POINT ( 'NONE', #33050 ) ;
#9308 = CARTESIAN_POINT ( 'NONE',  ( 76.04209377433248562, -175.3837268820161057, -10.93003379476866677 ) ) ;
#9309 = EDGE_CURVE ( 'NONE', #19466, #46209, #29366, .T. ) ;
#9310 = DIRECTION ( 'NONE',  ( -0.000000000000000000, -0.9350162426854132791, 0.3546048870425396182 ) ) ;
#9311 = ORIENTED_EDGE ( 'NONE', *, *, #10110, .T. ) ;
#9312 = ADVANCED_FACE ( 'NONE', ( #41192 ), #46139, .T. ) ;
#9313 = DIRECTION ( 'NONE',  ( 0.000000000000000000, -0.9709418174260544543, -0.2393156642875482465 ) ) ;
#9314 = DIRECTION ( 'NONE',  ( -0.02963332782257007553, 0.000000000000000000, 0.9995608365087941261 ) ) ;
#9315 = DIRECTION ( 'NONE',  ( 0.000000000000000000, 1.000000000000000000, -0.000000000000000000 ) ) ;
#9316 = DIRECTION ( 'NONE',  ( 0.000000000000000000, 0.000000000000000000, -1.000000000000000000 ) ) ;
#9317 = EDGE_CURVE ( 'NONE', #43356, #17362, #13080, .T. ) ;
#9318 = ORIENTED_EDGE ( 'NONE', *, *, #39642, .T. ) ;
#9319 = DIRECTION ( 'NONE',  ( -1.000000000000000000, 0.000000000000000000, -0.000000000000000000 ) ) ;
#9320 = ORIENTED_EDGE ( 'NONE', *, *, #2432, .T. ) ;
#9321 = ORIENTED_EDGE ( 'NONE', *, *, #12756, .F. ) ;
#9322 = VECTOR ( 'NONE', #31163, 1000.000000000000000 ) ;
#9323 = LINE ( 'NONE', #13261, #1788 ) ;
#9325 = VERTEX_POINT ( 'NONE', #39267 ) ;
#9324 = CARTESIAN_POINT ( 'NONE',  ( -336.3521761649654422, -153.6873197461136158, -51.85292399224849902 ) ) ;
#9326 = VERTEX_POINT ( 'NONE', #42699 ) ;
#9327 = CARTESIAN_POINT ( 'NONE',  ( -336.3521761649654422, -113.7752393642576720, 58.25253621232167944 ) ) ;
#9328 = EDGE_CURVE ( 'NONE', #25619, #46012, #26669, .T. ) ;
#9329 = CARTESIAN_POINT ( 'NONE',  ( 8.879953965148883910, -175.3837268820161057, 109.9360785596608707 ) ) ;
#9330 = ORIENTED_EDGE ( 'NONE', *, *, #40895, .T. ) ;
#9331 = CARTESIAN_POINT ( 'NONE',  ( -48.47912675150885065, -183.6283474603465606, 6.938893903907228378E-15 ) ) ;
#9332 = EDGE_LOOP ( 'NONE', ( #22287, #14899, #13291, #16461 ) ) ;
#9333 = FACE_OUTER_BOUND ( 'NONE', #49656, .T. ) ;
#9334 = DIRECTION ( 'NONE',  ( -0.000000000000000000, 1.000000000000000000, -0.000000000000000000 ) ) ;
#9335 = FACE_OUTER_BOUND ( 'NONE', #24261, .T. ) ;
#9336 = DIRECTION ( 'NONE',  ( -0.000000000000000000, 1.000000000000000000, 0.000000000000000000 ) ) ;
#9337 = ORIENTED_EDGE ( 'NONE', *, *, #8632, .T. ) ;
#9338 = ORIENTED_EDGE ( 'NONE', *, *, #31926, .T. ) ;
#9340 = ORIENTED_EDGE ( 'NONE', *, *, #21689, .T. ) ;
#9339 = CIRCLE ( 'NONE', #16053, 60.00000000000000000 ) ;
#9341 = CARTESIAN_POINT ( 'NONE',  ( -1.079983486989452192E-15, 45.00000000000000000, 0.000000000000000000 ) ) ;
#9342 = PLANE ( 'NONE',  #15091 ) ;
#9343 = DIRECTION ( 'NONE',  ( 0.000000000000000000, 0.000000000000000000, 1.000000000000000000 ) ) ;
#9344 = DIRECTION ( 'NONE',  ( -0.000000000000000000, 1.000000000000000000, -0.000000000000000000 ) ) ;
#9345 = ORIENTED_EDGE ( 'NONE', *, *, #13552, .F. ) ;
#9346 = EDGE_CURVE ( 'NONE', #27143, #6578, #34536, .T. ) ;
#9347 = EDGE_CURVE ( 'NONE', #19097, #44141, #46915, .T. ) ;
#9348 = EDGE_CURVE ( 'NONE', #20876, #13540, #3274, .T. ) ;
#9349 = ORIENTED_EDGE ( 'NONE', *, *, #13516, .F. ) ;
#9351 = ORIENTED_EDGE ( 'NONE', *, *, #21443, .T. ) ;
#9350 = FACE_OUTER_BOUND ( 'NONE', #13777, .T. ) ;
#9352 = CARTESIAN_POINT ( 'NONE',  ( -48.30223647638627682, -193.5000000000000000, -0.9842305779475897243 ) ) ;
#9353 = VERTEX_POINT ( 'NONE', #51126 ) ;
#9354 = AXIS2_PLACEMENT_3D ( 'NONE', #40007, #27677, #32385 ) ;
#9355 = CARTESIAN_POINT ( 'NONE',  ( -336.3521761649654422, -147.2170408776451609, -55.11353710303946940 ) ) ;
#9356 = DIRECTION ( 'NONE',  ( 0.000000000000000000, 0.000000000000000000, 1.000000000000000000 ) ) ;
#9357 = FACE_OUTER_BOUND ( 'NONE', #5591, .T. ) ;
#9358 = DIRECTION ( 'NONE',  ( 0.000000000000000000, 5.319818659662208160E-15, -1.000000000000000000 ) ) ;
#9359 = DIRECTION ( 'NONE',  ( -0.8757349421956379665, 0.000000000000000000, 0.4827922027307427477 ) ) ;
#9360 = VERTEX_POINT ( 'NONE', #18521 ) ;
#9361 = LINE ( 'NONE', #41927, #24178 ) ;
#9362 = ORIENTED_EDGE ( 'NONE', *, *, #8949, .F. ) ;
#9363 = ORIENTED_EDGE ( 'NONE', *, *, #31220, .T. ) ;
#9364 = DIRECTION ( 'NONE',  ( 0.000000000000000000, 0.8229838658936575735, 0.5680647467311540355 ) ) ;
#9365 = EDGE_CURVE ( 'NONE', #31967, #10943, #14587, .T. ) ;
#9366 = DIRECTION ( 'NONE',  ( -0.000000000000000000, 1.000000000000000000, -0.000000000000000000 ) ) ;
#9367 = VERTEX_POINT ( 'NONE', #43201 ) ;
#9368 = VECTOR ( 'NONE', #50613, 1000.000000000000000 ) ;
#9369 = VECTOR ( 'NONE', #35878, 1000.000000000000000 ) ;
#9370 = CARTESIAN_POINT ( 'NONE',  ( -336.3521761649654422, -91.32752733096738496, -49.48329383994654052 ) ) ;
#9371 = CARTESIAN_POINT ( 'NONE',  ( -332.3517673607765914, -100.1170788342122080, 54.23253582808833073 ) ) ;
#9372 = DIRECTION ( 'NONE',  ( 0.000000000000000000, 0.000000000000000000, 1.000000000000000000 ) ) ;
#9373 = CARTESIAN_POINT ( 'NONE',  ( -48.47912675150885065, -175.3837268820161057, 6.938893903907228378E-15 ) ) ;
#9374 = CIRCLE ( 'NONE', #31191, 125.0000000000000000 ) ;
#9375 = DIRECTION ( 'NONE',  ( -0.000000000000000000, -1.000000000000000000, 0.000000000000000000 ) ) ;
#9376 = ADVANCED_FACE ( 'NONE', ( #6706 ), #35317, .T. ) ;
#9377 = VECTOR ( 'NONE', #31023, 1000.000000000000114 ) ;
#9378 = CARTESIAN_POINT ( 'NONE',  ( -47.70260288879081401, -183.6283474603465606, 0.6300878435817218737 ) ) ;
#9379 = FACE_BOUND ( 'NONE', #51928, .T. ) ;
#9380 = EDGE_LOOP ( 'NONE', ( #8175, #18014, #5541, #43730 ) ) ;
#9381 = CARTESIAN_POINT ( 'NONE',  ( -48.71401279728984690, -193.5000000000000000, 0.9720229140804159673 ) ) ;
#9382 = VERTEX_POINT ( 'NONE', #15113 ) ;
#9383 = CARTESIAN_POINT ( 'NONE',  ( -155.9155026329808607, -193.5000000000000000, -61.91627321685031404 ) ) ;
#9384 = ORIENTED_EDGE ( 'NONE', *, *, #10826, .T. ) ;
#9385 = FACE_OUTER_BOUND ( 'NONE', #28511, .T. ) ;
#9386 = ORIENTED_EDGE ( 'NONE', *, *, #18590, .T. ) ;
#9387 = AXIS2_PLACEMENT_3D ( 'NONE', #40841, #24307, #16945 ) ;
#9388 = FACE_OUTER_BOUND ( 'NONE', #15131, .T. ) ;
#9389 = AXIS2_PLACEMENT_3D ( 'NONE', #26969, #47741, #43003 ) ;
#9390 = CYLINDRICAL_SURFACE ( 'NONE', #10013, 124.9999999999999858 ) ;
#9392 = ORIENTED_EDGE ( 'NONE', *, *, #46155, .F. ) ;
#9391 = LINE ( 'NONE', #40916, #33793 ) ;
#9393 = CARTESIAN_POINT ( 'NONE',  ( -68.21229068036657850, -183.6283474603465606, -123.4325817657429809 ) ) ;
#9394 = VERTEX_POINT ( 'NONE', #51615 ) ;
#9395 = ORIENTED_EDGE ( 'NONE', *, *, #1199, .T. ) ;
#9396 = ORIENTED_EDGE ( 'NONE', *, *, #20337, .F. ) ;
#9397 = CARTESIAN_POINT ( 'NONE',  ( -48.47912675150885065, -177.1207230881787780, 6.938893903907228378E-15 ) ) ;
#9398 = CARTESIAN_POINT ( 'NONE',  ( -330.4913330509368166, -172.5932850007654338, 34.49419324804716069 ) ) ;
#9399 = ORIENTED_EDGE ( 'NONE', *, *, #10221, .T. ) ;
#9400 = DIRECTION ( 'NONE',  ( 0.000000000000000000, 1.000000000000000000, 0.000000000000000000 ) ) ;
#9401 = CARTESIAN_POINT ( 'NONE',  ( -330.4913330509368166, -123.5000000000000284, 0.000000000000000000 ) ) ;
#9402 = CARTESIAN_POINT ( 'NONE',  ( -339.1964088526558498, -123.5000000000000284, 0.000000000000000000 ) ) ;
#9403 = AXIS2_PLACEMENT_3D ( 'NONE', #37852, #20796, #5297 ) ;
#9404 = VERTEX_POINT ( 'NONE', #23500 ) ;
#9405 = EDGE_CURVE ( 'NONE', #42603, #23736, #35737, .T. ) ;
#9406 = VECTOR ( 'NONE', #25085, 1000.000000000000114 ) ;
#9407 = CIRCLE ( 'NONE', #36251, 4.999999999999997335 ) ;
#9408 = CARTESIAN_POINT ( 'NONE',  ( -151.4272465800706300, -177.1207230881787780, 70.89911581792885897 ) ) ;
#9409 = LINE ( 'NONE', #26668, #39878 ) ;
#9410 = VERTEX_POINT ( 'NONE', #51368 ) ;
#9412 = ORIENTED_EDGE ( 'NONE', *, *, #14430, .T. ) ;
#9411 = LINE ( 'NONE', #37520, #28140 ) ;
#9413 = VERTEX_POINT ( 'NONE', #2743 ) ;
#9414 = EDGE_LOOP ( 'NONE', ( #49689, #23648, #33869, #7352 ) ) ;
#9415 = DIRECTION ( 'NONE',  ( -0.9995608365087940150, 0.000000000000000000, -0.02963332782257007206 ) ) ;
#9416 = ORIENTED_EDGE ( 'NONE', *, *, #2516, .T. ) ;
#9417 = CARTESIAN_POINT ( 'NONE',  ( 60.00000000000000000, -63.50000000000000000, -60.00000000000000711 ) ) ;
#9418 = DIRECTION ( 'NONE',  ( 0.000000000000000000, 0.000000000000000000, -1.000000000000000000 ) ) ;
#9419 = ORIENTED_EDGE ( 'NONE', *, *, #10706, .F. ) ;
#9420 = CARTESIAN_POINT ( 'NONE',  ( -339.1964088526558498, -64.99044476834248485, -7.608018572113150135 ) ) ;
#9421 = ORIENTED_EDGE ( 'NONE', *, *, #22807, .F. ) ;
#9422 = VECTOR ( 'NONE', #6351, 1000.000000000000000 ) ;
#9423 = ORIENTED_EDGE ( 'NONE', *, *, #3447, .T. ) ;
#9424 = DIRECTION ( 'NONE',  ( 0.000000000000000000, -0.4647231720437755564, -0.8854560256532062468 ) ) ;
#9425 = AXIS2_PLACEMENT_3D ( 'NONE', #48238, #16178, #8023 ) ;
#9427 = AXIS2_PLACEMENT_3D ( 'NONE', #48452, #28191, #4288 ) ;
#9426 = DIRECTION ( 'NONE',  ( 1.000000000000000000, 0.000000000000000000, -6.978251959525016136E-17 ) ) ;
#9428 = ADVANCED_FACE ( 'NONE', ( #31117 ), #11141, .T. ) ;
#9429 = CARTESIAN_POINT ( 'NONE',  ( 67.64905612629584652, -183.6283474603465606, -43.47841891815124882 ) ) ;
#9430 = CARTESIAN_POINT ( 'NONE',  ( -48.59739992243020623, -177.1207230881787780, -0.9929810960135115883 ) ) ;
#9431 = ORIENTED_EDGE ( 'NONE', *, *, #31727, .T. ) ;
#9432 = CARTESIAN_POINT ( 'NONE',  ( 48.47907891923915713, -193.5000000000000000, 78.89300572996904748 ) ) ;
#9433 = CARTESIAN_POINT ( 'NONE',  ( -108.5723883981723930, -177.1207230881787780, 109.6074810615846360 ) ) ;
#9434 = APPLICATION_PROTOCOL_DEFINITION ( 'draft international standard', 'automotive_design', 1998, #30352 ) ;
#9435 = CARTESIAN_POINT ( 'NONE',  ( -336.3521761649654422, -86.34605966037949543, -45.90766452162698386 ) ) ;
#9436 = DIRECTION ( 'NONE',  ( -0.000000000000000000, 0.000000000000000000, -1.000000000000000000 ) ) ;
#9437 = CARTESIAN_POINT ( 'NONE',  ( -48.98765787015805984, -193.5000000000000000, -0.8610436117673551104 ) ) ;
#9438 = LINE ( 'NONE', #4714, #24842 ) ;
#9439 = CARTESIAN_POINT ( 'NONE',  ( 4.298610786024391605E-15, 20.00000000000000000, -41.00000000000000711 ) ) ;
#9440 = VERTEX_POINT ( 'NONE', #7210 ) ;
#9441 = AXIS2_PLACEMENT_3D ( 'NONE', #21773, #13367, #8638 ) ;
#9442 = DIRECTION ( 'NONE',  ( 0.000000000000000000, 0.000000000000000000, 1.000000000000000000 ) ) ;
#9443 = DIRECTION ( 'NONE',  ( -0.000000000000000000, 0.9927088740980556381, 0.1205366802553095307 ) ) ;
#9444 = EDGE_LOOP ( 'NONE', ( #1456, #3063, #5912, #2097 ) ) ;
#9445 = EDGE_LOOP ( 'NONE', ( #49110, #38253, #26388, #9719 ) ) ;
#9446 = EDGE_CURVE ( 'NONE', #13290, #25971, #3516, .T. ) ;
#9447 = ORIENTED_EDGE ( 'NONE', *, *, #18087, .F. ) ;
#9448 = VECTOR ( 'NONE', #33369, 1000.000000000000000 ) ;
#9449 = DIRECTION ( 'NONE',  ( 0.000000000000000000, 0.000000000000000000, 1.000000000000000000 ) ) ;
#9450 = LINE ( 'NONE', #4469, #34595 ) ;
#9451 = DIRECTION ( 'NONE',  ( 0.000000000000000000, -1.000000000000000000, 0.000000000000000000 ) ) ;
#9452 = DIRECTION ( 'NONE',  ( 0.000000000000000000, -0.8229838658936634577, -0.5680647467311457088 ) ) ;
#9453 = DIRECTION ( 'NONE',  ( -0.4827922027307551267, 0.000000000000000000, 0.8757349421956311941 ) ) ;
#9454 = CIRCLE ( 'NONE', #18687, 16.00000000000000711 ) ;
#9455 = ORIENTED_EDGE ( 'NONE', *, *, #39755, .F. ) ;
#9456 = CIRCLE ( 'NONE', #1040, 125.0000000000000000 ) ;
#9457 = DIRECTION ( 'NONE',  ( 0.000000000000000000, 0.000000000000000000, 1.000000000000000000 ) ) ;
#9458 = ADVANCED_FACE ( 'NONE', ( #31371 ), #47413, .T. ) ;
#9459 = ORIENTED_EDGE ( 'NONE', *, *, #8944, .F. ) ;
#9460 = FACE_OUTER_BOUND ( 'NONE', #20499, .T. ) ;
#9461 = VECTOR ( 'NONE', #26219, 1000.000000000000000 ) ;
#9462 = AXIS2_PLACEMENT_3D ( 'NONE', #47845, #38903, #35738 ) ;
#9463 = ORIENTED_EDGE ( 'NONE', *, *, #2532, .F. ) ;
#9464 = FACE_OUTER_BOUND ( 'NONE', #6484, .T. ) ;
#9465 = EDGE_LOOP ( 'NONE', ( #15946, #32271, #12859, #40664 ) ) ;
#9466 = ADVANCED_FACE ( 'NONE', ( #43475 ), #7478, .F. ) ;
#9467 = AXIS2_PLACEMENT_3D ( 'NONE', #6549, #42790, #2591 ) ;
#9468 = EDGE_CURVE ( 'NONE', #47944, #46596, #38495, .T. ) ;
#9469 = LINE ( 'NONE', #17628, #51912 ) ;
#9470 = DIRECTION ( 'NONE',  ( -1.000000000000000000, 0.000000000000000000, -0.000000000000000000 ) ) ;
#9471 = ORIENTED_EDGE ( 'NONE', *, *, #21164, .F. ) ;
#9474 = ORIENTED_EDGE ( 'NONE', *, *, #33047, .F. ) ;
#9473 = PLANE ( 'NONE',  #45136 ) ;
#9472 = DIRECTION ( 'NONE',  ( 0.000000000000000000, 0.000000000000000000, 1.000000000000000000 ) ) ;
#9475 = EDGE_CURVE ( 'NONE', #30972, #3140, #47932, .T. ) ;
#9476 = CARTESIAN_POINT ( 'NONE',  ( -305.0000000000000568, -177.3662605214052519, -26.42775013958059560 ) ) ;
#9477 = ORIENTED_EDGE ( 'NONE', *, *, #16352, .T. ) ;
#9478 = CARTESIAN_POINT ( 'NONE',  ( -47.64924157374594671, -175.3837268820161057, 124.9972451320097377 ) ) ;
#9479 = AXIS2_PLACEMENT_3D ( 'NONE', #1730, #14874, #38749 ) ;
#9480 = EDGE_LOOP ( 'NONE', ( #6824, #44894, #27882, #9917 ) ) ;
#9481 = DIRECTION ( 'NONE',  ( 0.000000000000000000, 0.000000000000000000, -1.000000000000000000 ) ) ;
#9484 = ORIENTED_EDGE ( 'NONE', *, *, #43337, .F. ) ;
#9483 = DIRECTION ( 'NONE',  ( 0.000000000000000000, 0.000000000000000000, -1.000000000000000000 ) ) ;
#9482 = CARTESIAN_POINT ( 'NONE',  ( -160.2705093830644216, -183.6283474603465606, -55.92572546981521242 ) ) ;
#9485 = VERTEX_POINT ( 'NONE', #36351 ) ;
#9486 = CIRCLE ( 'NONE', #22046, 125.0000000000000000 ) ;
#9487 = LINE ( 'NONE', #41017, #42487 ) ;
#9488 = DIRECTION ( 'NONE',  ( -0.9785564922995060311, 0.000000000000000000, 0.2059786187410889424 ) ) ;
#9489 = CARTESIAN_POINT ( 'NONE',  ( -330.4913330509368166, -89.57268800991444380, 48.27201571435978877 ) ) ;
#9490 = VERTEX_POINT ( 'NONE', #19800 ) ;
#9491 = ADVANCED_FACE ( 'NONE', ( #23753 ), #36881, .T. ) ;
#9492 = DIRECTION ( 'NONE',  ( -0.5829794791144820021, 0.000000000000000000, 0.8124868780056742068 ) ) ;
#9493 = DIRECTION ( 'NONE',  ( -0.000000000000000000, 0.2393156642875547968, -0.9709418174260527890 ) ) ;
#9494 = DIRECTION ( 'NONE',  ( 0.000000000000000000, 0.000000000000000000, -1.000000000000000000 ) ) ;
#9495 = DIRECTION ( 'NONE',  ( 0.000000000000000000, 0.000000000000000000, 1.000000000000000000 ) ) ;
#9496 = AXIS2_PLACEMENT_3D ( 'NONE', #24423, #19965, #23893 ) ;
#9497 = DIRECTION ( 'NONE',  ( 5.399917434947259359E-17, 1.000000000000000000, -0.000000000000000000 ) ) ;
#9498 = VECTOR ( 'NONE', #13055, 1000.000000000000227 ) ;
#9499 = CARTESIAN_POINT ( 'NONE',  ( 73.50869128264334051, -183.6283474603465606, -22.25084316132034701 ) ) ;
#9500 = CARTESIAN_POINT ( 'NONE',  ( -336.3521761649653854, -173.7880015656344312, -32.72792230702632565 ) ) ;
#9501 = ORIENTED_EDGE ( 'NONE', *, *, #34453, .F. ) ;
#9502 = CIRCLE ( 'NONE', #29627, 125.0000000000000000 ) ;
#9503 = CARTESIAN_POINT ( 'NONE',  ( -339.1964088526558498, -162.9984922102920848, 43.83057281297495678 ) ) ;
#9504 = CARTESIAN_POINT ( 'NONE',  ( -49.45768324380835423, -193.5000000000000000, 0.2059786187410958813 ) ) ;
#9505 = CARTESIAN_POINT ( 'NONE',  ( -332.3517673607765914, -133.2247606357419443, -58.25253621232173629 ) ) ;
#9506 = CARTESIAN_POINT ( 'NONE',  ( -151.9915035862630646, -193.5000000000000000, 70.07273251429430161 ) ) ;
#9507 = AXIS2_PLACEMENT_3D ( 'NONE', #25921, #33554, #14109 ) ;
#9508 = PLANE ( 'NONE',  #36342 ) ;
#9509 = LINE ( 'NONE', #578, #6857 ) ;
#9510 = FACE_OUTER_BOUND ( 'NONE', #19591, .T. ) ;
#9512 = ORIENTED_EDGE ( 'NONE', *, *, #35668, .F. ) ;
#9511 = FACE_OUTER_BOUND ( 'NONE', #20436, .T. ) ;
#9513 = VECTOR ( 'NONE', #34440, 1000.000000000000114 ) ;
#9514 = ORIENTED_EDGE ( 'NONE', *, *, #46911, .T. ) ;
#9515 = EDGE_CURVE ( 'NONE', #12661, #34438, #28198, .T. ) ;
#9516 = EDGE_CURVE ( 'NONE', #34486, #46012, #4048, .T. ) ;
#9517 = DIRECTION ( 'NONE',  ( 0.8455960035018272869, 0.000000000000000000, -0.5338233779647886257 ) ) ;
#9518 = AXIS2_PLACEMENT_3D ( 'NONE', #43699, #12137, #4537 ) ;
#9520 = ORIENTED_EDGE ( 'NONE', *, *, #1622, .F. ) ;
#9519 = CARTESIAN_POINT ( 'NONE',  ( 141.7825277784304205, -213.5000000000000000, 10.00000000000000178 ) ) ;
#9521 = ORIENTED_EDGE ( 'NONE', *, *, #28568, .F. ) ;
#9522 = ORIENTED_EDGE ( 'NONE', *, *, #661, .F. ) ;
#9523 = CARTESIAN_POINT ( 'NONE',  ( -339.1964088526558498, -89.57268800991437274, 48.27201571435973904 ) ) ;
#9524 = ADVANCED_FACE ( 'NONE', ( #36615 ), #7975, .F. ) ;
#9525 = CARTESIAN_POINT ( 'NONE',  ( -4.176930889631405464, -175.3837268820161057, 116.8859077982279615 ) ) ;
#9526 = FACE_OUTER_BOUND ( 'NONE', #48847, .T. ) ;
#9528 = ORIENTED_EDGE ( 'NONE', *, *, #29096, .T. ) ;
#9527 = AXIS2_PLACEMENT_3D ( 'NONE', #21638, #37658, #49507 ) ;
#9529 = EDGE_CURVE ( 'NONE', #3419, #20713, #1382, .T. ) ;
#9530 = DIRECTION ( 'NONE',  ( 0.000000000000000000, 1.000000000000000000, 0.000000000000000000 ) ) ;
#9532 = EDGE_LOOP ( 'NONE', ( #4409, #30399, #13443, #40431 ) ) ;
#9531 = DIRECTION ( 'NONE',  ( 0.000000000000000000, -0.000000000000000000, 1.000000000000000000 ) ) ;
#9533 = AXIS2_PLACEMENT_3D ( 'NONE', #45113, #13024, #41146 ) ;
#9534 = EDGE_CURVE ( 'NONE', #18514, #4438, #16912, .T. ) ;
#9535 = PLANE ( 'NONE',  #41507 ) ;
#9536 = ORIENTED_EDGE ( 'NONE', *, *, #44292, .T. ) ;
#9537 = LINE ( 'NONE', #21360, #28886 ) ;
#9538 = EDGE_CURVE ( 'NONE', #32555, #24446, #16394, .T. ) ;
#9539 = ORIENTED_EDGE ( 'NONE', *, *, #17297, .T. ) ;
#9540 = CARTESIAN_POINT ( 'NONE',  ( -48.47912675150885065, -189.7472609257535510, 6.938893903907228378E-15 ) ) ;
#9541 = DIRECTION ( 'NONE',  ( 0.8757349421956379665, 0.000000000000000000, -0.4827922027307427477 ) ) ;
#9542 = DIRECTION ( 'NONE',  ( 0.000000000000000000, 1.000000000000000000, 0.000000000000000000 ) ) ;
#9543 = ORIENTED_EDGE ( 'NONE', *, *, #5162, .F. ) ;
#9544 = ORIENTED_EDGE ( 'NONE', *, *, #36762, .F. ) ;
#9545 = DIRECTION ( 'NONE',  ( 0.000000000000000000, -1.000000000000000000, 0.000000000000000000 ) ) ;
#9546 = CARTESIAN_POINT ( 'NONE',  ( -49.08592689732743963, -183.6283474603465606, -0.7948544414133539293 ) ) ;
#9547 = ORIENTED_EDGE ( 'NONE', *, *, #3578, .F. ) ;
#9548 = DIRECTION ( 'NONE',  ( 0.000000000000000000, 0.000000000000000000, 1.000000000000000000 ) ) ;
#9549 = VECTOR ( 'NONE', #41756, 1000.000000000000114 ) ;
#9550 = EDGE_LOOP ( 'NONE', ( #20044, #2252, #15959, #42394 ) ) ;
#9551 = DIRECTION ( 'NONE',  ( -0.000000000000000000, 1.000000000000000000, -0.000000000000000000 ) ) ;
#9553 = VECTOR ( 'NONE', #2414, 1000.000000000000000 ) ;
#9552 = CARTESIAN_POINT ( 'NONE',  ( -336.3521761649654422, -70.49953203435293858, 25.97334715265942151 ) ) ;
#9554 = ORIENTED_EDGE ( 'NONE', *, *, #4181, .F. ) ;
#9555 = CARTESIAN_POINT ( 'NONE',  ( -305.0000000000000568, -66.51961791625839737, 18.79457521708899392 ) ) ;
#9556 = VERTEX_POINT ( 'NONE', #24008 ) ;
#9557 = FACE_OUTER_BOUND ( 'NONE', #31945, .T. ) ;
#9558 = CARTESIAN_POINT ( 'NONE',  ( -305.0000000000000568, -182.1255794688777314, -12.76876783163924323 ) ) ;
#9559 = ORIENTED_EDGE ( 'NONE', *, *, #36762, .T. ) ;
#9560 = LINE ( 'NONE', #28476, #7231 ) ;
#9561 = DIRECTION ( 'NONE',  ( -0.000000000000000000, 1.000000000000000000, -0.000000000000000000 ) ) ;
#9562 = FACE_OUTER_BOUND ( 'NONE', #9805, .T. ) ;
#9563 = AXIS2_PLACEMENT_3D ( 'NONE', #21488, #37768, #1240 ) ;
#9564 = DIRECTION ( 'NONE',  ( 0.000000000000000000, 0.000000000000000000, -1.000000000000000000 ) ) ;
#9565 = EDGE_LOOP ( 'NONE', ( #32056, #12443, #5007, #18584 ) ) ;
#9566 = CARTESIAN_POINT ( 'NONE',  ( 75.67769207106684348, -177.1207230881787780, 14.49428645563876650 ) ) ;
#9567 = ORIENTED_EDGE ( 'NONE', *, *, #2800, .F. ) ;
#9568 = EDGE_CURVE ( 'NONE', #9092, #12643, #11910, .T. ) ;
#9569 = ORIENTED_EDGE ( 'NONE', *, *, #27978, .F. ) ;
#9570 = CARTESIAN_POINT ( 'NONE',  ( -48.47912675150885065, -175.3837268820161057, 6.938893903907228378E-15 ) ) ;
#9572 = VERTEX_POINT ( 'NONE', #16667 ) ;
#9571 = FACE_OUTER_BOUND ( 'NONE', #46588, .T. ) ;
#9573 = EDGE_CURVE ( 'NONE', #10121, #33538, #44769, .T. ) ;
#9574 = ORIENTED_EDGE ( 'NONE', *, *, #29160, .F. ) ;
#9575 = EDGE_CURVE ( 'NONE', #39066, #13383, #8750, .T. ) ;
#9576 = DIRECTION ( 'NONE',  ( 0.000000000000000000, -2.326842422443557418E-13, 1.000000000000000000 ) ) ;
#9577 = ADVANCED_FACE ( 'NONE', ( #40541 ), #39757, .T. ) ;
#9578 = EDGE_CURVE ( 'NONE', #1828, #22639, #4297, .T. ) ;
#9579 = DIRECTION ( 'NONE',  ( -0.000000000000000000, 1.000000000000000000, -0.000000000000000000 ) ) ;
#9580 = EDGE_LOOP ( 'NONE', ( #29487, #24304, #7581, #22511 ) ) ;
#9581 = LINE ( 'NONE', #13525, #17219 ) ;
#9582 = EDGE_CURVE ( 'NONE', #42659, #33404, #48460, .T. ) ;
#9583 = ORIENTED_EDGE ( 'NONE', *, *, #29374, .F. ) ;
#9584 = DIRECTION ( 'NONE',  ( 0.5085311186492273983, 0.000000000000000000, -0.8610436117673514467 ) ) ;
#9585 = DIRECTION ( 'NONE',  ( -0.000000000000000000, 1.000000000000000000, -0.000000000000000000 ) ) ;
#9586 = AXIS2_PLACEMENT_3D ( 'NONE', #44589, #39348, #3353 ) ;
#9587 = CIRCLE ( 'NONE', #22190, 125.0000000000000000 ) ;
#9588 = EDGE_CURVE ( 'NONE', #30266, #26571, #9791, .T. ) ;
#9589 = CARTESIAN_POINT ( 'NONE',  ( -153.7737137892885073, -193.5000000000000000, -65.49088066501643368 ) ) ;
#9590 = DIRECTION ( 'NONE',  ( -0.4566292373937200777, 0.000000000000000000, 0.8896570909947436601 ) ) ;
#9591 = VERTEX_POINT ( 'NONE', #31893 ) ;
#9592 = ORIENTED_EDGE ( 'NONE', *, *, #13850, .F. ) ;
#9593 = AXIS2_PLACEMENT_3D ( 'NONE', #32759, #27519, #43555 ) ;
#9594 = ADVANCED_FACE ( 'NONE', ( #40804 ), #24790, .T. ) ;
#9595 = ORIENTED_EDGE ( 'NONE', *, *, #33546, .F. ) ;
#9596 = DIRECTION ( 'NONE',  ( -0.000000000000000000, 1.000000000000000000, -0.000000000000000000 ) ) ;
#9597 = DIRECTION ( 'NONE',  ( 0.9151456172430153524, 0.000000000000000000, 0.4031234292879792847 ) ) ;
#9598 = EDGE_CURVE ( 'NONE', #8921, #33930, #43723, .T. ) ;
#9599 = FACE_OUTER_BOUND ( 'NONE', #18883, .T. ) ;
#9600 = CARTESIAN_POINT ( 'NONE',  ( -77.03256798524175508, -189.7472609257535510, 121.6951149130964893 ) ) ;
#9601 = VERTEX_POINT ( 'NONE', #41585 ) ;
#9602 = ADVANCED_FACE ( 'NONE', ( #25311 ), #14008, .F. ) ;
#9603 = CIRCLE ( 'NONE', #9637, 125.0000000000000000 ) ;
#9604 = EDGE_CURVE ( 'NONE', #1758, #36353, #4765, .T. ) ;
#9605 = ORIENTED_EDGE ( 'NONE', *, *, #3695, .F. ) ;
#9607 = ORIENTED_EDGE ( 'NONE', *, *, #42109, .F. ) ;
#9606 = DIRECTION ( 'NONE',  ( 0.000000000000000000, -0.000000000000000000, -1.000000000000000000 ) ) ;
#9608 = ORIENTED_EDGE ( 'NONE', *, *, #16992, .T. ) ;
#9609 = DIRECTION ( 'NONE',  ( -0.000000000000000000, 1.000000000000000000, -0.000000000000000000 ) ) ;
#9610 = DIRECTION ( 'NONE',  ( -0.000000000000000000, 0.9350162426854107256, -0.3546048870425463906 ) ) ;
#9611 = DIRECTION ( 'NONE',  ( 0.000000000000000000, 0.000000000000000000, 1.000000000000000000 ) ) ;
#9612 = CARTESIAN_POINT ( 'NONE',  ( -336.3521761649654422, -164.5945333327934463, -42.41660376256285048 ) ) ;
#9613 = VERTEX_POINT ( 'NONE', #30031 ) ;
#9614 = CARTESIAN_POINT ( 'NONE',  ( -48.47912675150885065, -183.6283474603465606, 6.938893903907228378E-15 ) ) ;
#9615 = ORIENTED_EDGE ( 'NONE', *, *, #27234, .F. ) ;
#9616 = EDGE_CURVE ( 'NONE', #22071, #38204, #46080, .T. ) ;
#9617 = ORIENTED_EDGE ( 'NONE', *, *, #24688, .F. ) ;
#9618 = CARTESIAN_POINT ( 'NONE',  ( -157.1522883217072604, -175.3837268820161057, 59.71720175837172206 ) ) ;
#9619 = DIRECTION ( 'NONE',  ( 0.05924062789371441901, 0.000000000000000000, -0.9982437317643214625 ) ) ;
#9620 = ORIENTED_EDGE ( 'NONE', *, *, #33967, .T. ) ;
#9621 = VECTOR ( 'NONE', #8176, 1000.000000000000000 ) ;
#9622 = CIRCLE ( 'NONE', #45718, 125.0000000000000000 ) ;
#9623 = DIRECTION ( 'NONE',  ( -1.000000000000000000, -0.000000000000000000, 4.884776371667511665E-16 ) ) ;
#9624 = DIRECTION ( 'NONE',  ( -0.000000000000000000, 1.000000000000000000, -0.000000000000000000 ) ) ;
#9625 = DIRECTION ( 'NONE',  ( 0.000000000000000000, -0.8229838658936613482, -0.5680647467311485954 ) ) ;
#9626 = CARTESIAN_POINT ( 'NONE',  ( -332.3517673607765914, -133.2247606357419443, -58.25253621232173629 ) ) ;
#9627 = AXIS2_PLACEMENT_3D ( 'NONE', #30829, #18744, #46876 ) ;
#9628 = DIRECTION ( 'NONE',  ( 0.000000000000000000, 1.156482317317871449E-14, -1.000000000000000000 ) ) ;
#9629 = DIRECTION ( 'NONE',  ( 0.8124868780056783146, 0.000000000000000000, 0.5829794791144762289 ) ) ;
#9630 = VERTEX_POINT ( 'NONE', #13743 ) ;
#9631 = CARTESIAN_POINT ( 'NONE',  ( -339.1964088526558498, -173.1613497474965300, 33.67120938215357739 ) ) ;
#9632 = EDGE_LOOP ( 'NONE', ( #1543, #42137, #37905, #8270 ) ) ;
#9633 = EDGE_CURVE ( 'NONE', #21582, #24818, #33710, .T. ) ;
#9634 = EDGE_LOOP ( 'NONE', ( #7097, #10302 ) ) ;
#9635 = ADVANCED_FACE ( 'NONE', ( #9802 ), #45551, .F. ) ;
#9636 = CARTESIAN_POINT ( 'NONE',  ( -180.0000000000000568, -123.5000000000000284, 0.000000000000000000 ) ) ;
#9637 = AXIS2_PLACEMENT_3D ( 'NONE', #50583, #14583, #10631 ) ;
#9638 = ORIENTED_EDGE ( 'NONE', *, *, #15285, .F. ) ;
#9639 = EDGE_CURVE ( 'NONE', #27923, #895, #45038, .T. ) ;
#9640 = ADVANCED_FACE ( 'NONE', ( #17170 ), #13229, .T. ) ;
#9641 = CARTESIAN_POINT ( 'NONE',  ( 11.52087324849114580, -132.5479369270331915, 60.00000000000002132 ) ) ;
#9642 = DIRECTION ( 'NONE',  ( -0.000000000000000000, -1.000000000000000000, 0.000000000000000000 ) ) ;
#9644 = VERTEX_POINT ( 'NONE', #41860 ) ;
#9643 = CARTESIAN_POINT ( 'NONE',  ( -332.3517673607765914, -132.2320517616439020, -58.37307289257706344 ) ) ;
#9645 = DIRECTION ( 'NONE',  ( -0.8757349421956345248, 0.000000000000000000, -0.4827922027307490205 ) ) ;
#9646 = ORIENTED_EDGE ( 'NONE', *, *, #9346, .T. ) ;
#9647 = ORIENTED_EDGE ( 'NONE', *, *, #13325, .T. ) ;
#9648 = ORIENTED_EDGE ( 'NONE', *, *, #29663, .F. ) ;
#9649 = CARTESIAN_POINT ( 'NONE',  ( -48.41988612361515010, -175.3837268820161057, 0.9982437317643287900 ) ) ;
#9650 = FACE_OUTER_BOUND ( 'NONE', #7883, .T. ) ;
#9651 = VECTOR ( 'NONE', #3596, 1000.000000000000114 ) ;
#9652 = ADVANCED_FACE ( 'NONE', ( #33468 ), #9289, .F. ) ;
#9653 = ORIENTED_EDGE ( 'NONE', *, *, #11124, .T. ) ;
#9654 = PLANE ( 'NONE',  #10856 ) ;
#9655 = VECTOR ( 'NONE', #43480, 1000.000000000000000 ) ;
#9656 = DIRECTION ( 'NONE',  ( -1.000000000000000000, 0.000000000000000000, -0.000000000000000000 ) ) ;
#9657 = CARTESIAN_POINT ( 'NONE',  ( -141.2664123866436512, -189.7472609257535510, -83.75869879877495805 ) ) ;
#9658 = VERTEX_POINT ( 'NONE', #5875 ) ;
#9659 = VECTOR ( 'NONE', #19389, 1000.000000000000000 ) ;
#9660 = EDGE_CURVE ( 'NONE', #16711, #29476, #22147, .T. ) ;
#9661 = FACE_OUTER_BOUND ( 'NONE', #3291, .T. ) ;
#9662 = DIRECTION ( 'NONE',  ( 0.000000000000000000, 0.000000000000000000, -1.000000000000000000 ) ) ;
#9663 = EDGE_LOOP ( 'NONE', ( #23122, #47390, #6057, #14155 ) ) ;
#9665 = VERTEX_POINT ( 'NONE', #49752 ) ;
#9664 = DIRECTION ( 'NONE',  ( 0.1768902751225666370, 0.000000000000000000, 0.9842305779475979399 ) ) ;
#9666 = VERTEX_POINT ( 'NONE', #28972 ) ;
#9667 = VECTOR ( 'NONE', #39117, 1000.000000000000000 ) ;
#9668 = EDGE_LOOP ( 'NONE', ( #6676, #40421, #2160, #4533 ) ) ;
#9669 = CARTESIAN_POINT ( 'NONE',  ( 76.52053249983501360, -183.6283474603465606, -0.2918682030015273265 ) ) ;
#9670 = CARTESIAN_POINT ( 'NONE',  ( -332.3517673607765914, -182.2665742509934148, -5.491276508484069119 ) ) ;
#9671 = AXIS2_PLACEMENT_3D ( 'NONE', #40075, #48759, #36662 ) ;
#9672 = VERTEX_POINT ( 'NONE', #29500 ) ;
#9673 = LINE ( 'NONE', #10437, #17825 ) ;
#9674 = CARTESIAN_POINT ( 'NONE',  ( -332.3517673607765914, -123.5000000000000284, 0.000000000000000000 ) ) ;
#9675 = ORIENTED_EDGE ( 'NONE', *, *, #50392, .F. ) ;
#9676 = CARTESIAN_POINT ( 'NONE',  ( -48.47912675150885065, -177.1207230881787780, 6.938893903907228378E-15 ) ) ;
#9677 = VECTOR ( 'NONE', #51546, 1000.000000000000114 ) ;
#9678 = VERTEX_POINT ( 'NONE', #17448 ) ;
#9679 = AXIS2_PLACEMENT_3D ( 'NONE', #10487, #30215, #33636 ) ;
#9680 = EDGE_LOOP ( 'NONE', ( #37141, #25871, #24226, #46427 ) ) ;
#9681 = CARTESIAN_POINT ( 'NONE',  ( 75.78974234412359579, -193.5000000000000000, 13.49993235881449394 ) ) ;
#9682 = CARTESIAN_POINT ( 'NONE',  ( -155.4121128832437364, -183.6283474603465606, -62.78108192021942813 ) ) ;
#9683 = DIRECTION ( 'NONE',  ( 1.000000000000000000, -0.000000000000000000, -0.000000000000000000 ) ) ;
#9684 = DIRECTION ( 'NONE',  ( 0.000000000000000000, -1.000000000000000000, 0.000000000000000000 ) ) ;
#9685 = VERTEX_POINT ( 'NONE', #37912 ) ;
#9686 = DIRECTION ( 'NONE',  ( -0.000000000000000000, 1.000000000000000000, -0.000000000000000000 ) ) ;
#9687 = CARTESIAN_POINT ( 'NONE',  ( 51.78320179844649118, -175.3837268820161057, -72.96212019587142095 ) ) ;
#9688 = CONTEXT_DEPENDENT_SHAPE_REPRESENTATION ( #25991, #24715 ) ;
#9689 = DIRECTION ( 'NONE',  ( 1.000000000000000000, 0.000000000000000000, -0.000000000000000000 ) ) ;
#9690 = LINE ( 'NONE', #25718, #36306 ) ;
#9691 = ORIENTED_EDGE ( 'NONE', *, *, #27934, .T. ) ;
#9692 = DIRECTION ( 'NONE',  ( 0.000000000000000000, 0.000000000000000000, 1.000000000000000000 ) ) ;
#9693 = CYLINDRICAL_SURFACE ( 'NONE', #32369, 125.0000000000000000 ) ;
#9694 = CARTESIAN_POINT ( 'NONE',  ( -48.47912675150885065, -189.7472609257535510, 6.938893903907228378E-15 ) ) ;
#9695 = EDGE_LOOP ( 'NONE', ( #33515, #5351, #11078, #37850 ) ) ;
#9696 = EDGE_LOOP ( 'NONE', ( #49892, #26792, #6641, #12551 ) ) ;
#9697 = VECTOR ( 'NONE', #11620, 999.9999999999998863 ) ;
#9698 = AXIS2_PLACEMENT_3D ( 'NONE', #9034, #41589, #9293 ) ;
#9699 = CIRCLE ( 'NONE', #12191, 60.00000000000000000 ) ;
#9700 = CARTESIAN_POINT ( 'NONE',  ( 64.29733702426837283, -193.5000000000000000, 53.91167979418564471 ) ) ;
#9701 = CARTESIAN_POINT ( 'NONE',  ( -330.4913330509368166, -150.4759391377560576, -52.47426709956116042 ) ) ;
#9702 = ORIENTED_EDGE ( 'NONE', *, *, #47746, .T. ) ;
#9703 = ADVANCED_FACE ( 'NONE', ( #38158 ), #2167, .F. ) ;
#9704 = EDGE_CURVE ( 'NONE', #885, #32675, #17951, .T. ) ;
#9705 = DIRECTION ( 'NONE',  ( 0.000000000000000000, 0.000000000000000000, 1.000000000000000000 ) ) ;
#9706 = ORIENTED_EDGE ( 'NONE', *, *, #19143, .T. ) ;
#9707 = LINE ( 'NONE', #46242, #16121 ) ;
#9708 = AXIS2_PLACEMENT_3D ( 'NONE', #18833, #43011, #14917 ) ;
#9709 = CARTESIAN_POINT ( 'NONE',  ( -85.48706473349324142, -175.3837268820161057, -118.3487137068146637 ) ) ;
#9710 = AXIS2_PLACEMENT_3D ( 'NONE', #45467, #13140, #9457 ) ;
#9711 = CARTESIAN_POINT ( 'NONE',  ( 76.28370911321319170, -177.1207230881787780, -7.696413904697508634 ) ) ;
#9712 = VECTOR ( 'NONE', #27639, 1000.000000000000000 ) ;
#9713 = CARTESIAN_POINT ( 'NONE',  ( -48.47912675150885065, -183.6283474603465606, 6.938893903907228378E-15 ) ) ;
#9714 = EDGE_LOOP ( 'NONE', ( #44688, #36971, #15457, #40672 ) ) ;
#9715 = CARTESIAN_POINT ( 'NONE',  ( -124.4642912599203726, -193.5000000000000000, 99.25348746834863789 ) ) ;
#9716 = ORIENTED_EDGE ( 'NONE', *, *, #32358, .F. ) ;
#9717 = AXIS2_PLACEMENT_3D ( 'NONE', #1246, #17303, #41450 ) ;
#9718 = CARTESIAN_POINT ( 'NONE',  ( -78.00521078983979351, -175.3837268820161057, 121.4627941443857111 ) ) ;
#9719 = ORIENTED_EDGE ( 'NONE', *, *, #51956, .T. ) ;
#9720 = EDGE_CURVE ( 'NONE', #5531, #1746, #9030, .T. ) ;
#9721 = DIRECTION ( 'NONE',  ( 0.000000000000000000, 0.000000000000000000, -1.000000000000000000 ) ) ;
#9722 = ORIENTED_EDGE ( 'NONE', *, *, #26254, .F. ) ;
#9723 = ADVANCED_FACE ( 'NONE', ( #33960 ), #41073, .T. ) ;
#9724 = DIRECTION ( 'NONE',  ( 0.6068001458185834363, 0.000000000000000000, 0.7948544414133608127 ) ) ;
#9725 = DIRECTION ( 'NONE',  ( -0.9993203489176063492, 0.000000000000000000, -0.03686245026030391531 ) ) ;
#9726 = ORIENTED_EDGE ( 'NONE', *, *, #41365, .T. ) ;
#9729 = ORIENTED_EDGE ( 'NONE', *, *, #13010, .F. ) ;
#9728 = DIRECTION ( 'NONE',  ( 0.000000000000000000, -0.8229838658936516893, 0.5680647467311626952 ) ) ;
#9727 = CARTESIAN_POINT ( 'NONE',  ( -1.446716803940739871, 57.92321382262407070, -16.54047372258810000 ) ) ;
#9730 = AXIS2_PLACEMENT_3D ( 'NONE', #8649, #48873, #36775 ) ;
#9731 = PLANE ( 'NONE',  #16392 ) ;
#9732 = VECTOR ( 'NONE', #2105, 1000.000000000000227 ) ;
#9733 = ORIENTED_EDGE ( 'NONE', *, *, #7167, .F. ) ;
#9734 = LINE ( 'NONE', #29182, #28051 ) ;
#9735 = ORIENTED_EDGE ( 'NONE', *, *, #23840, .T. ) ;
#9736 = AXIS2_PLACEMENT_3D ( 'NONE', #12851, #28875, #4992 ) ;
#9737 = EDGE_CURVE ( 'NONE', #20555, #40265, #34235, .T. ) ;
#9738 = DIRECTION ( 'NONE',  ( -0.000000000000000000, 1.000000000000000000, -0.000000000000000000 ) ) ;
#9741 = ORIENTED_EDGE ( 'NONE', *, *, #9660, .F. ) ;
#9740 = PLANE ( 'NONE',  #37569 ) ;
#9739 = DIRECTION ( 'NONE',  ( 0.000000000000000000, 0.000000000000000000, 1.000000000000000000 ) ) ;
#9742 = ORIENTED_EDGE ( 'NONE', *, *, #15996, .F. ) ;
#9743 = DIRECTION ( 'NONE',  ( -0.2059786187411094538, 0.000000000000000000, 0.9785564922995017012 ) ) ;
#9744 = PLANE ( 'NONE',  #8558 ) ;
#9745 = DIRECTION ( 'NONE',  ( 0.000000000000000000, -6.129356281784718821E-14, -1.000000000000000000 ) ) ;
#9746 = VERTEX_POINT ( 'NONE', #11076 ) ;
#9747 = AXIS2_PLACEMENT_3D ( 'NONE', #48126, #12893, #8696 ) ;
#9748 = CARTESIAN_POINT ( 'NONE',  ( -330.4913330509368166, -123.5000000000000284, 0.000000000000000000 ) ) ;
#9749 = LINE ( 'NONE', #25262, #39987 ) ;
#9750 = CARTESIAN_POINT ( 'NONE',  ( -173.4787860028527007, -177.1207230881787780, 0.2918682030023981300 ) ) ;
#9751 = AXIS2_PLACEMENT_3D ( 'NONE', #43741, #39531, #32172 ) ;
#9752 = FACE_OUTER_BOUND ( 'NONE', #42762, .T. ) ;
#9753 = ORIENTED_EDGE ( 'NONE', *, *, #22486, .T. ) ;
#9754 = SHAPE_REPRESENTATION_RELATIONSHIP ( 'NONE' , 'NONE' ,  #33452, #24902 ) ;
#9755 = CIRCLE ( 'NONE', #39101, 125.0000000000000000 ) ;
#9756 = DIRECTION ( 'NONE',  ( -0.6068001458185834363, 0.000000000000000000, -0.7948544414133608127 ) ) ;
#9757 = DIRECTION ( 'NONE',  ( 0.000000000000000000, -1.000000000000000000, 0.000000000000000000 ) ) ;
#9758 = EDGE_CURVE ( 'NONE', #29300, #45837, #15294, .T. ) ;
#9759 = VECTOR ( 'NONE', #10635, 1000.000000000000114 ) ;
#9760 = CARTESIAN_POINT ( 'NONE',  ( -48.47912675150885065, -189.7472609257535510, 6.938893903907228378E-15 ) ) ;
#9761 = ORIENTED_EDGE ( 'NONE', *, *, #37951, .F. ) ;
#9762 = CARTESIAN_POINT ( 'NONE',  ( -29.73468717939733708, -183.6283474603465606, 123.5865930638411214 ) ) ;
#9763 = CARTESIAN_POINT ( 'NONE',  ( -339.1964088526558498, -167.3305728129748786, -39.49849221029221269 ) ) ;
#9764 = LINE ( 'NONE', #34447, #5062 ) ;
#9765 = ADVANCED_FACE ( 'NONE', ( #47354 ), #6384, .F. ) ;
#9766 = DIRECTION ( 'NONE',  ( 0.000000000000000000, -0.8229838658936634577, -0.5680647467311457088 ) ) ;
#9767 = ADVANCED_FACE ( 'NONE', ( #46850 ), #14526, .T. ) ;
#9768 = CIRCLE ( 'NONE', #34111, 125.0000000000000000 ) ;
#9769 = AXIS2_PLACEMENT_3D ( 'NONE', #27517, #3600, #35143 ) ;
#9770 = CARTESIAN_POINT ( 'NONE',  ( 70.68712318874649725, -183.6283474603465606, -37.74128873232327663 ) ) ;
#9771 = LINE ( 'NONE', #48684, #22834 ) ;
#9773 = EDGE_LOOP ( 'NONE', ( #6767, #30032, #25661, #50425 ) ) ;
#9772 = DIRECTION ( 'NONE',  ( 0.000000000000000000, 0.4647231720437695057, 0.8854560256532093554 ) ) ;
#9774 = VERTEX_POINT ( 'NONE', #18979 ) ;
#9775 = CARTESIAN_POINT ( 'NONE',  ( -154.2693405752510500, -175.3837268820161057, 66.58401203837830451 ) ) ;
#9776 = FACE_OUTER_BOUND ( 'NONE', #12631, .T. ) ;
#9778 = ORIENTED_EDGE ( 'NONE', *, *, #28211, .T. ) ;
#9777 = DIRECTION ( 'NONE',  ( 1.000000000000000000, -0.000000000000000000, -0.000000000000000000 ) ) ;
#9779 = VECTOR ( 'NONE', #27698, 1000.000000000000000 ) ;
#9780 = ORIENTED_EDGE ( 'NONE', *, *, #47286, .F. ) ;
#9781 = AXIS2_PLACEMENT_3D ( 'NONE', #24469, #11856, #32347 ) ;
#9782 = VERTEX_POINT ( 'NONE', #22666 ) ;
#9783 = ADVANCED_FACE ( 'NONE', ( #11329 ), #26851, .F. ) ;
#9784 = LINE ( 'NONE', #29480, #9101 ) ;
#9785 = AXIS2_PLACEMENT_3D ( 'NONE', #25916, #37224, #1214 ) ;
#9786 = AXIS2_PLACEMENT_3D ( 'NONE', #27964, #42242, #35855 ) ;
#9788 = AXIS2_PLACEMENT_3D ( 'NONE', #23800, #19348, #15414 ) ;
#9787 = LINE ( 'NONE', #37374, #19395 ) ;
#9789 = DIRECTION ( 'NONE',  ( 0.000000000000000000, -0.000000000000000000, 1.000000000000000000 ) ) ;
#9790 = ORIENTED_EDGE ( 'NONE', *, *, #8849, .T. ) ;
#9791 = CIRCLE ( 'NONE', #30752, 60.00000000000000000 ) ;
#9792 = DIRECTION ( 'NONE',  ( -0.000000000000000000, 1.000000000000000000, 0.000000000000000000 ) ) ;
#9794 = ORIENTED_EDGE ( 'NONE', *, *, #48323, .F. ) ;
#9793 = DIRECTION ( 'NONE',  ( 0.000000000000000000, 0.8854560256532079121, -0.4647231720437724478 ) ) ;
#9795 = VECTOR ( 'NONE', #17374, 1000.000000000000000 ) ;
#9796 = DIRECTION ( 'NONE',  ( 0.000000000000000000, 0.000000000000000000, 1.000000000000000000 ) ) ;
#9797 = EDGE_LOOP ( 'NONE', ( #22442, #32121, #40796, #32082 ) ) ;
#9798 = LINE ( 'NONE', #49744, #24693 ) ;
#9799 = ORIENTED_EDGE ( 'NONE', *, *, #29800, .F. ) ;
#9800 = CARTESIAN_POINT ( 'NONE',  ( 74.31448861501726810, -183.6283474603465606, -23.38221600314288651 ) ) ;
#9801 = LINE ( 'NONE', #26598, #33868 ) ;
#9802 = FACE_OUTER_BOUND ( 'NONE', #5743, .T. ) ;
#9803 = ORIENTED_EDGE ( 'NONE', *, *, #48887, .F. ) ;
#9804 = VECTOR ( 'NONE', #7500, 1000.000000000000114 ) ;
#9805 = EDGE_LOOP ( 'NONE', ( #25771, #37969, #11173, #14883 ) ) ;
#9806 = DIRECTION ( 'NONE',  ( 0.000000000000000000, 0.8854560256532079121, -0.4647231720437724478 ) ) ;
#9807 = VECTOR ( 'NONE', #8514, 1000.000000000000000 ) ;
#9808 = CARTESIAN_POINT ( 'NONE',  ( -169.3144491972411458, -177.1207230881787780, -27.83926365844663664 ) ) ;
#9809 = ORIENTED_EDGE ( 'NONE', *, *, #51347, .T. ) ;
#9810 = CARTESIAN_POINT ( 'NONE',  ( -70.58093260035830951, -189.7472609257535510, 122.0143860769388908 ) ) ;
#9811 = VECTOR ( 'NONE', #10610, 1000.000000000000114 ) ;
#9812 = ADVANCED_FACE ( 'NONE', ( #26339 ), #38677, .F. ) ;
#9813 = ORIENTED_EDGE ( 'NONE', *, *, #29055, .T. ) ;
#9814 = CARTESIAN_POINT ( 'NONE',  ( 49.03269102277813829, 30.00000000000000355, -50.83217377521822300 ) ) ;
#9815 = CARTESIAN_POINT ( 'NONE',  ( -339.1964088526558498, -124.0000000000002700, -59.99791663049643375 ) ) ;
#9816 = ORIENTED_EDGE ( 'NONE', *, *, #25590, .T. ) ;
#9817 = LINE ( 'NONE', #25846, #8131 ) ;
#9818 = EDGE_LOOP ( 'NONE', ( #49940, #12789, #23230, #912 ) ) ;
#9819 = VECTOR ( 'NONE', #15834, 1000.000000000000114 ) ;
#9820 = DIRECTION ( 'NONE',  ( -1.000000000000000000, 0.000000000000000000, 0.000000000000000000 ) ) ;
#9821 = VECTOR ( 'NONE', #47051, 1000.000000000000000 ) ;
#9822 = PLANE ( 'NONE',  #43793 ) ;
#9823 = EDGE_LOOP ( 'NONE', ( #13671, #26887, #46861, #19077 ) ) ;
#9824 = AXIS2_PLACEMENT_3D ( 'NONE', #7655, #2437, #47352 ) ;
#9825 = CIRCLE ( 'NONE', #4802, 125.0000000000000000 ) ;
#9826 = CARTESIAN_POINT ( 'NONE',  ( -48.47912675150885065, -175.3837268820161057, 6.938893903907228378E-15 ) ) ;
#9827 = CARTESIAN_POINT ( 'NONE',  ( -330.4913330509368166, -151.3613951634084742, 52.00954392751779665 ) ) ;
#9828 = CARTESIAN_POINT ( 'NONE',  ( -339.1964088526558498, -130.1153096980144426, 58.63009191191295599 ) ) ;
#9829 = EDGE_CURVE ( 'NONE', #12249, #46797, #6889, .T. ) ;
#9830 = AXIS2_PLACEMENT_3D ( 'NONE', #23949, #40488, #36551 ) ;
#9831 = CARTESIAN_POINT ( 'NONE',  ( -41.24387117724851493, -175.3837268820161057, 124.7904286264581231 ) ) ;
#9832 = ADVANCED_FACE ( 'NONE', ( #43414 ), #10316, .T. ) ;
#9833 = ORIENTED_EDGE ( 'NONE', *, *, #28832, .T. ) ;
#9835 = AXIS2_PLACEMENT_3D ( 'NONE', #1329, #29967, #1063 ) ;
#9834 = DIRECTION ( 'NONE',  ( 0.000000000000000000, 0.9709418174260511236, -0.2393156642875615969 ) ) ;
#9836 = ORIENTED_EDGE ( 'NONE', *, *, #34328, .T. ) ;
#9837 = EDGE_CURVE ( 'NONE', #13772, #5824, #18464, .T. ) ;
#9838 = CARTESIAN_POINT ( 'NONE',  ( -336.3521761649654422, -99.78295912235451226, 55.11353710303931308 ) ) ;
#9840 = ORIENTED_EDGE ( 'NONE', *, *, #45895, .T. ) ;
#9839 = LINE ( 'NONE', #6160, #28676 ) ;
#9841 = EDGE_LOOP ( 'NONE', ( #618, #48341, #49336, #50336 ) ) ;
#9842 = FACE_OUTER_BOUND ( 'NONE', #33965, .T. ) ;
#9843 = AXIS2_PLACEMENT_3D ( 'NONE', #20135, #27753, #48258 ) ;
#9844 = AXIS2_PLACEMENT_3D ( 'NONE', #16879, #16628, #44206 ) ;
#9845 = ORIENTED_EDGE ( 'NONE', *, *, #16746, .T. ) ;
#9846 = DIRECTION ( 'NONE',  ( 0.000000000000000000, 0.000000000000000000, 1.000000000000000000 ) ) ;
#9847 = EDGE_LOOP ( 'NONE', ( #20899, #23804, #1109, #49467 ) ) ;
#9848 = FACE_OUTER_BOUND ( 'NONE', #48014, .T. ) ;
#9849 = LINE ( 'NONE', #1702, #36742 ) ;
#9850 = AXIS2_PLACEMENT_3D ( 'NONE', #12607, #49418, #37040 ) ;
#9851 = CARTESIAN_POINT ( 'NONE',  ( -48.47912675150885065, -189.7472609257535510, 6.938893903907228378E-15 ) ) ;
#9852 = LINE ( 'NONE', #46375, #41703 ) ;
#9853 = VERTEX_POINT ( 'NONE', #26599 ) ;
#9854 = VERTEX_POINT ( 'NONE', #6647 ) ;
#9855 = ORIENTED_EDGE ( 'NONE', *, *, #32706, .T. ) ;
#9856 = CARTESIAN_POINT ( 'NONE',  ( -133.8011377042516301, -177.1207230881787780, -91.35181687837437892 ) ) ;
#9857 = LINE ( 'NONE', #25881, #35236 ) ;
#9858 = AXIS2_PLACEMENT_3D ( 'NONE', #18515, #30583, #46642 ) ;
#9859 = VECTOR ( 'NONE', #9793, 999.9999999999998863 ) ;
#9860 = AXIS2_PLACEMENT_3D ( 'NONE', #10959, #15174, #24857 ) ;
#9861 = DIRECTION ( 'NONE',  ( -1.000000000000000000, 0.000000000000000000, 0.000000000000000000 ) ) ;
#9862 = DIRECTION ( 'NONE',  ( -0.000000000000000000, 0.5680647467311625842, 0.8229838658936516893 ) ) ;
#9863 = ORIENTED_EDGE ( 'NONE', *, *, #30162, .F. ) ;
#9864 = AXIS2_PLACEMENT_3D ( 'NONE', #38629, #26541, #15243 ) ;
#9865 = VECTOR ( 'NONE', #36273, 1000.000000000000114 ) ;
#9866 = VERTEX_POINT ( 'NONE', #38932 ) ;
#9868 = VERTEX_POINT ( 'NONE', #31308 ) ;
#9867 = LINE ( 'NONE', #14077, #18970 ) ;
#9869 = ORIENTED_EDGE ( 'NONE', *, *, #47522, .T. ) ;
#9870 = CARTESIAN_POINT ( 'NONE',  ( -173.4190745413846457, -175.3837268820161057, -3.874202661594927211 ) ) ;
#9871 = PLANE ( 'NONE',  #51849 ) ;
#9872 = EDGE_CURVE ( 'NONE', #14916, #48059, #3064, .T. ) ;
#9873 = PLANE ( 'NONE',  #51406 ) ;
#9874 = EDGE_CURVE ( 'NONE', #9242, #14212, #47578, .T. ) ;
#9875 = ADVANCED_FACE ( 'NONE', ( #19242 ), #38432, .T. ) ;
#9876 = DIRECTION ( 'NONE',  ( 0.000000000000000000, -0.5000000000000054401, -0.8660254037844354880 ) ) ;
#9877 = VERTEX_POINT ( 'NONE', #35504 ) ;
#9878 = DIRECTION ( 'NONE',  ( -0.000000000000000000, -1.000000000000000000, 0.000000000000000000 ) ) ;
#9879 = ORIENTED_EDGE ( 'NONE', *, *, #40781, .T. ) ;
#9880 = EDGE_CURVE ( 'NONE', #41928, #25092, #36648, .T. ) ;
#9881 = ORIENTED_EDGE ( 'NONE', *, *, #13872, .T. ) ;
#9882 = CARTESIAN_POINT ( 'NONE',  ( -62.43888699632653783, -175.3837268820161057, 124.2180546213279371 ) ) ;
#9883 = CIRCLE ( 'NONE', #30020, 125.0000000000000000 ) ;
#9884 = AXIS2_PLACEMENT_3D ( 'NONE', #49377, #34106, #33589 ) ;
#9885 = ADVANCED_FACE ( 'NONE', ( #2680 ), #18720, .T. ) ;
#9886 = CARTESIAN_POINT ( 'NONE',  ( -170.0000000000000284, -173.5000000000000284, -60.00000000000001421 ) ) ;
#9887 = ORIENTED_EDGE ( 'NONE', *, *, #33600, .F. ) ;
#9888 = EDGE_CURVE ( 'NONE', #13637, #1466, #51552, .T. ) ;
#9889 = CIRCLE ( 'NONE', #19153, 125.0000000000000000 ) ;
#9890 = CARTESIAN_POINT ( 'NONE',  ( -48.47912675150885065, -117.5479369270332057, -14.99999999999999289 ) ) ;
#9891 = LINE ( 'NONE', #13036, #39758 ) ;
#9892 = FACE_OUTER_BOUND ( 'NONE', #50399, .T. ) ;
#9893 = EDGE_CURVE ( 'NONE', #35294, #26421, #45071, .T. ) ;
#9894 = FACE_OUTER_BOUND ( 'NONE', #13604, .T. ) ;
#9895 = EDGE_CURVE ( 'NONE', #9685, #23874, #43370, .T. ) ;
#9896 = DIRECTION ( 'NONE',  ( 0.000000000000000000, 1.000000000000000000, 0.000000000000000000 ) ) ;
#9897 = FACE_BOUND ( 'NONE', #19852, .T. ) ;
#9898 = ADVANCED_FACE ( 'NONE', ( #20006 ), #543, .F. ) ;
#9899 = EDGE_LOOP ( 'NONE', ( #47402, #14302, #17003, #24794 ) ) ;
#9900 = AXIS2_PLACEMENT_3D ( 'NONE', #33509, #913, #9584 ) ;
#9901 = EDGE_CURVE ( 'NONE', #16323, #27843, #32336, .T. ) ;
#9902 = CARTESIAN_POINT ( 'NONE',  ( -339.1964088526558498, -123.5000000000000284, 0.000000000000000000 ) ) ;
#9903 = AXIS2_PLACEMENT_3D ( 'NONE', #3527, #18786, #43484 ) ;
#9904 = ADVANCED_FACE ( 'NONE', ( #3709 ), #39962, .T. ) ;
#9905 = ORIENTED_EDGE ( 'NONE', *, *, #22043, .T. ) ;
#9906 = DIRECTION ( 'NONE',  ( 0.9266896074318291543, 0.000000000000000000, 0.3758275821142488260 ) ) ;
#9907 = ORIENTED_EDGE ( 'NONE', *, *, #13578, .F. ) ;
#9908 = VECTOR ( 'NONE', #20188, 1000.000000000000000 ) ;
#9909 = DIRECTION ( 'NONE',  ( 0.000000000000000000, 1.000000000000000000, 0.000000000000000000 ) ) ;
#9910 = DIRECTION ( 'NONE',  ( 0.000000000000000000, 0.000000000000000000, 1.000000000000000000 ) ) ;
#9912 = VERTEX_POINT ( 'NONE', #32085 ) ;
#9911 = LINE ( 'NONE', #25926, #6978 ) ;
#9913 = DIRECTION ( 'NONE',  ( 0.000000000000000000, 0.000000000000000000, -1.000000000000000000 ) ) ;
#9914 = CARTESIAN_POINT ( 'NONE',  ( -2.700932609314997457, -177.1207230881787780, -116.3157639405751809 ) ) ;
#9915 = EDGE_CURVE ( 'NONE', #31493, #10996, #31837, .T. ) ;
#9916 = VERTEX_POINT ( 'NONE', #27875 ) ;
#9917 = ORIENTED_EDGE ( 'NONE', *, *, #31161, .T. ) ;
#9918 = EDGE_LOOP ( 'NONE', ( #32684, #50827, #24457, #11066 ) ) ;
#9919 = DIRECTION ( 'NONE',  ( -0.000000000000000000, 1.000000000000000000, -0.000000000000000000 ) ) ;
#9920 = AXIS2_PLACEMENT_3D ( 'NONE', #1400, #8756, #17706 ) ;
#9921 = LINE ( 'NONE', #5728, #8396 ) ;
#9922 = AXIS2_PLACEMENT_3D ( 'NONE', #49627, #30410, #50158 ) ;
#9923 = DIRECTION ( 'NONE',  ( -0.000000000000000000, 1.000000000000000000, -0.000000000000000000 ) ) ;
#9924 = DIRECTION ( 'NONE',  ( -0.000000000000000000, 1.000000000000000000, -0.000000000000000000 ) ) ;
#9925 = DIRECTION ( 'NONE',  ( 0.9266896074318343723, 0.000000000000000000, -0.3758275821142357809 ) ) ;
#9926 = ORIENTED_EDGE ( 'NONE', *, *, #48142, .T. ) ;
#9927 = DIRECTION ( 'NONE',  ( 0.7378332790417239107, 0.000000000000000000, 0.6749830015182142207 ) ) ;
#9928 = EDGE_CURVE ( 'NONE', #4219, #27267, #47876, .T. ) ;
#9929 = ORIENTED_EDGE ( 'NONE', *, *, #12161, .T. ) ;
#9931 = VERTEX_POINT ( 'NONE', #28399 ) ;
#9930 = DIRECTION ( 'NONE',  ( -0.6965510290630033685, 0.000000000000000000, 0.7175072570443249420 ) ) ;
#9932 = AXIS2_PLACEMENT_3D ( 'NONE', #6294, #49153, #25484 ) ;
#9933 = VERTEX_POINT ( 'NONE', #40741 ) ;
#9934 = ORIENTED_EDGE ( 'NONE', *, *, #3598, .T. ) ;
#9935 = LINE ( 'NONE', #18838, #11533 ) ;
#9936 = LINE ( 'NONE', #51374, #36498 ) ;
#9937 = ORIENTED_EDGE ( 'NONE', *, *, #33060, .T. ) ;
#9938 = EDGE_CURVE ( 'NONE', #30058, #10177, #3900, .T. ) ;
#9939 = EDGE_CURVE ( 'NONE', #5079, #3221, #36035, .T. ) ;
#9940 = CARTESIAN_POINT ( 'NONE',  ( -336.3521761649654422, -127.9985676343858501, 58.88711093124869222 ) ) ;
#9941 = ADVANCED_FACE ( 'NONE', ( #31568 ), #20260, .T. ) ;
#9942 = EDGE_CURVE ( 'NONE', #34815, #23236, #19735, .T. ) ;
#9943 = FACE_OUTER_BOUND ( 'NONE', #41355, .T. ) ;
#9944 = EDGE_LOOP ( 'NONE', ( #27550, #19519, #2572, #7327 ) ) ;
#9945 = FACE_OUTER_BOUND ( 'NONE', #43815, .T. ) ;
#9946 = ORIENTED_EDGE ( 'NONE', *, *, #40048, .F. ) ;
#9947 = ADVANCED_FACE ( 'NONE', ( #11848 ), #47623, .F. ) ;
#9948 = AXIS2_PLACEMENT_3D ( 'NONE', #32018, #7594, #27300 ) ;
#9949 = ORIENTED_EDGE ( 'NONE', *, *, #3980, .F. ) ;
#9950 = DIRECTION ( 'NONE',  ( -1.000000000000000000, -0.000000000000000000, -0.000000000000000000 ) ) ;
#9951 = LINE ( 'NONE', #14157, #25586 ) ;
#9952 = EDGE_CURVE ( 'NONE', #8894, #14662, #11606, .T. ) ;
#9953 = CARTESIAN_POINT ( 'NONE',  ( -332.3517673607765914, -174.5186198893880771, 29.74944317415823392 ) ) ;
#9954 = LINE ( 'NONE', #1272, #29086 ) ;
#9955 = EDGE_LOOP ( 'NONE', ( #36006, #32432, #20944, #38901 ) ) ;
#9956 = PLANE ( 'NONE',  #13103 ) ;
#9957 = LINE ( 'NONE', #46469, #28954 ) ;
#9958 = DIRECTION ( 'NONE',  ( -0.000000000000000000, 1.000000000000000000, -0.000000000000000000 ) ) ;
#9959 = CARTESIAN_POINT ( 'NONE',  ( 48.69345348225014192, -189.7472609257535510, -78.62880929222870918 ) ) ;
#9960 = EDGE_CURVE ( 'NONE', #1071, #32381, #32480, .T. ) ;
#9961 = ORIENTED_EDGE ( 'NONE', *, *, #36828, .T. ) ;
#9962 = PLANE ( 'NONE',  #51526 ) ;
#9963 = DIRECTION ( 'NONE',  ( 0.000000000000000000, -0.2393156642875652051, -0.9709418174260502354 ) ) ;
#9964 = EDGE_CURVE ( 'NONE', #8561, #18461, #36542, .T. ) ;
#9965 = CARTESIAN_POINT ( 'NONE',  ( -155.4121128832437364, -193.5000000000000000, -62.78108192021939971 ) ) ;
#9966 = VECTOR ( 'NONE', #50365, 1000.000000000000000 ) ;
#9967 = ORIENTED_EDGE ( 'NONE', *, *, #24844, .F. ) ;
#9968 = VECTOR ( 'NONE', #17962, 1000.000000000000114 ) ;
#9969 = EDGE_CURVE ( 'NONE', #40473, #27857, #3982, .T. ) ;
#9970 =( GEOMETRIC_REPRESENTATION_CONTEXT ( 3 ) GLOBAL_UNCERTAINTY_ASSIGNED_CONTEXT ( ( #42696 ) ) GLOBAL_UNIT_ASSIGNED_CONTEXT ( ( #32535, #11255, #51743 ) ) REPRESENTATION_CONTEXT ( 'NONE', 'WORKASPACE' ) );
#9971 = CYLINDRICAL_SURFACE ( 'NONE', #20568, 125.0000000000000000 ) ;
#9972 = VECTOR ( 'NONE', #6567, 1000.000000000000000 ) ;
#9973 = DIRECTION ( 'NONE',  ( -1.000000000000000000, 0.000000000000000000, 0.000000000000000000 ) ) ;
#9974 = EDGE_CURVE ( 'NONE', #31069, #38530, #3942, .T. ) ;
#9975 = DIRECTION ( 'NONE',  ( 0.000000000000000000, 0.000000000000000000, 1.000000000000000000 ) ) ;
#9976 = ORIENTED_EDGE ( 'NONE', *, *, #50429, .T. ) ;
#9977 = LINE ( 'NONE', #13643, #44730 ) ;
#9978 = ORIENTED_EDGE ( 'NONE', *, *, #20866, .T. ) ;
#9979 = EDGE_CURVE ( 'NONE', #13526, #4036, #16557, .T. ) ;
#9980 = VECTOR ( 'NONE', #10945, 1000.000000000000114 ) ;
#9981 = DIRECTION ( 'NONE',  ( 0.000000000000000000, 1.000000000000000000, 0.000000000000000000 ) ) ;
#9982 = DIRECTION ( 'NONE',  ( 0.000000000000000000, 1.000000000000000000, 0.000000000000000000 ) ) ;
#9983 = CARTESIAN_POINT ( 'NONE',  ( -48.47912675150885065, -189.7472609257535510, 6.938893903907228378E-15 ) ) ;
#9984 = FACE_OUTER_BOUND ( 'NONE', #3746, .T. ) ;
#9985 = DIRECTION ( 'NONE',  ( 0.000000000000000000, 1.000000000000000000, 0.000000000000000000 ) ) ;
#9986 = ORIENTED_EDGE ( 'NONE', *, *, #23100, .T. ) ;
#9987 = VECTOR ( 'NONE', #4628, 1000.000000000000000 ) ;
#9989 = EDGE_CURVE ( 'NONE', #42327, #1307, #50133, .T. ) ;
#9988 = DIRECTION ( 'NONE',  ( 0.000000000000000000, 1.000000000000000000, 0.000000000000000000 ) ) ;
#9990 = ORIENTED_EDGE ( 'NONE', *, *, #47852, .F. ) ;
#9991 = DIRECTION ( 'NONE',  ( -0.000000000000000000, 1.000000000000000000, -0.000000000000000000 ) ) ;
#9992 = EDGE_LOOP ( 'NONE', ( #19717, #11128, #43821, #46814 ) ) ;
#9993 = LINE ( 'NONE', #30457, #51953 ) ;
#9994 = FACE_OUTER_BOUND ( 'NONE', #33830, .T. ) ;
#9995 = LINE ( 'NONE', #17872, #36523 ) ;
#9996 = ORIENTED_EDGE ( 'NONE', *, *, #37697, .T. ) ;
#9999 = ORIENTED_EDGE ( 'NONE', *, *, #44612, .T. ) ;
#9998 = CARTESIAN_POINT ( 'NONE',  ( -330.4913330509368166, -103.0458197858324496, 55.34326076196052213 ) ) ;
#9997 = CARTESIAN_POINT ( 'NONE',  ( -4.014990372510813366, 55.84036979173559700, -17.50138700720797402 ) ) ;
#10000 = CIRCLE ( 'NONE', #51988, 31.65769145387501027 ) ;
#10001 = PLANE ( 'NONE',  #1302 ) ;
#10002 = EDGE_LOOP ( 'NONE', ( #13414, #17926, #29895, #20660 ) ) ;
#10003 = DIRECTION ( 'NONE',  ( 0.000000000000000000, 0.000000000000000000, 1.000000000000000000 ) ) ;
#10004 = AXIS2_PLACEMENT_3D ( 'NONE', #45471, #25487, #24710 ) ;
#10005 = ORIENTED_EDGE ( 'NONE', *, *, #12492, .T. ) ;
#10006 = EDGE_CURVE ( 'NONE', #20725, #46128, #29438, .T. ) ;
#10007 = EDGE_CURVE ( 'NONE', #13237, #4441, #49447, .T. ) ;
#10008 = FACE_OUTER_BOUND ( 'NONE', #31019, .T. ) ;
#10011 = ORIENTED_EDGE ( 'NONE', *, *, #39163, .F. ) ;
#10010 = DIRECTION ( 'NONE',  ( 0.000000000000000000, 0.8854560256532093554, -0.4647231720437695057 ) ) ;
#10009 = CARTESIAN_POINT ( 'NONE',  ( -164.8312043469690593, -177.1207230881787780, -42.87565520599202529 ) ) ;
#10012 = ORIENTED_EDGE ( 'NONE', *, *, #3995, .T. ) ;
#10013 = AXIS2_PLACEMENT_3D ( 'NONE', #27473, #35355, #10676 ) ;
#10014 = CARTESIAN_POINT ( 'NONE',  ( -168.1141659785444915, -183.6283474603465606, -36.22785377503947046 ) ) ;
#10015 = ORIENTED_EDGE ( 'NONE', *, *, #32402, .T. ) ;
#10016 = CARTESIAN_POINT ( 'NONE',  ( 54.54686566053560881, -183.6283474603465606, 69.00559874123592863 ) ) ;
#10017 = DIRECTION ( 'NONE',  ( -0.000000000000000000, 1.000000000000000000, -0.000000000000000000 ) ) ;
#10018 = EDGE_LOOP ( 'NONE', ( #44712, #44178, #28716, #50511 ) ) ;
#10019 = CARTESIAN_POINT ( 'NONE',  ( -332.3517673607765914, -69.26746417191145611, -23.38292116578723068 ) ) ;
#10020 = FACE_OUTER_BOUND ( 'NONE', #26093, .T. ) ;
#10021 = CARTESIAN_POINT ( 'NONE',  ( -114.9600645115007040, -177.1207230881787780, 105.8550183720738431 ) ) ;
#10022 = DIRECTION ( 'NONE',  ( 0.000000000000000000, 0.000000000000000000, -1.000000000000000000 ) ) ;
#10023 = DIRECTION ( 'NONE',  ( 0.000000000000000000, 0.000000000000000000, 1.000000000000000000 ) ) ;
#10024 = ORIENTED_EDGE ( 'NONE', *, *, #17021, .F. ) ;
#10025 =( NAMED_UNIT ( * ) SI_UNIT ( $, .STERADIAN. ) SOLID_ANGLE_UNIT ( ) );
#10026 = CARTESIAN_POINT ( 'NONE',  ( -169.2746641285359317, -193.5000000000000000, -32.14713283941905786 ) ) ;
#10027 = LINE ( 'NONE', #14483, #2968 ) ;
#10028 = DIRECTION ( 'NONE',  ( 0.9646355819083576311, 0.000000000000000000, 0.2635871660690715101 ) ) ;
#10029 = VERTEX_POINT ( 'NONE', #33407 ) ;
#10030 = CARTESIAN_POINT ( 'NONE',  ( 6.443011874827243801, -193.5000000000000000, 112.2878385610370771 ) ) ;
#10031 = FACE_OUTER_BOUND ( 'NONE', #23039, .T. ) ;
#10032 = EDGE_CURVE ( 'NONE', #19616, #47019, #17117, .T. ) ;
#10033 = CARTESIAN_POINT ( 'NONE',  ( 3.652658254809380445, -193.5000000000000000, -112.5098962032389522 ) ) ;
#10034 = CARTESIAN_POINT ( 'NONE',  ( 75.51463005422468200, -183.6283474603465606, -1.322128892811231360 ) ) ;
#10035 = EDGE_CURVE ( 'NONE', #47727, #37884, #18238, .T. ) ;
#10036 = DIRECTION ( 'NONE',  ( 5.399917434947259359E-17, 1.000000000000000000, -0.000000000000000000 ) ) ;
#10037 = VECTOR ( 'NONE', #48756, 1000.000000000000000 ) ;
#10038 = LINE ( 'NONE', #2129, #5214 ) ;
#10039 = FACE_OUTER_BOUND ( 'NONE', #43050, .T. ) ;
#10040 = CARTESIAN_POINT ( 'NONE',  ( -6.081033889300858419, -189.7472609257535510, -116.5264228893325651 ) ) ;
#10041 = STYLED_ITEM ( 'NONE', ( #34349 ), #35805 ) ;
#10042 = ORIENTED_EDGE ( 'NONE', *, *, #1879, .T. ) ;
#10043 = CARTESIAN_POINT ( 'NONE',  ( 1.150725574412429175, -175.3837268820161057, -114.7252272087845739 ) ) ;
#10044 = LINE ( 'NONE', #6104, #10373 ) ;
#10046 = ORIENTED_EDGE ( 'NONE', *, *, #9901, .T. ) ;
#10045 = DIRECTION ( 'NONE',  ( 1.000000000000000000, 0.000000000000000000, 6.978251959525016136E-17 ) ) ;
#10047 = VERTEX_POINT ( 'NONE', #10009 ) ;
#10048 = EDGE_LOOP ( 'NONE', ( #19144, #51750, #6923, #5788 ) ) ;
#10049 = DIRECTION ( 'NONE',  ( -0.8757349421956379665, 0.000000000000000000, 0.4827922027307427477 ) ) ;
#10050 = CARTESIAN_POINT ( 'NONE',  ( -47.70260288879080690, -193.5000000000000000, -0.6300878435817026668 ) ) ;
#10051 = CYLINDRICAL_SURFACE ( 'NONE', #24675, 125.0000000000000000 ) ;
#10052 = ORIENTED_EDGE ( 'NONE', *, *, #34379, .F. ) ;
#10053 = VECTOR ( 'NONE', #50387, 1000.000000000000000 ) ;
#10054 = PLANE ( 'NONE',  #35186 ) ;
#10055 = CARTESIAN_POINT ( 'NONE',  ( 20.10322172534453244, -189.7472609257535510, -103.3076327631962954 ) ) ;
#10057 = ORIENTED_EDGE ( 'NONE', *, *, #13683, .T. ) ;
#10056 = LINE ( 'NONE', #14518, #3962 ) ;
#10058 = CARTESIAN_POINT ( 'NONE',  ( -339.1964088526558498, -124.0000000000002700, -59.00000000000002132 ) ) ;
#10059 = VERTEX_POINT ( 'NONE', #13420 ) ;
#10060 = DIRECTION ( 'NONE',  ( 0.000000000000000000, 0.8660254037844379305, 0.5000000000000012212 ) ) ;
#10061 = ORIENTED_EDGE ( 'NONE', *, *, #4135, .T. ) ;
#10062 = EDGE_CURVE ( 'NONE', #27996, #21361, #13679, .T. ) ;
#10063 = DIRECTION ( 'NONE',  ( -0.6068001458185890984, 0.000000000000000000, -0.7948544414133565938 ) ) ;
#10064 = CARTESIAN_POINT ( 'NONE',  ( -180.0000000000000568, -123.5000000000000284, 20.00000000000001776 ) ) ;
#10065 = CARTESIAN_POINT ( 'NONE',  ( -330.4913330509368166, -180.6659093959932250, 14.60509510167933556 ) ) ;
#10066 = ORIENTED_EDGE ( 'NONE', *, *, #40048, .T. ) ;
#10067 = EDGE_LOOP ( 'NONE', ( #22010, #32577, #19119, #35112 ) ) ;
#10068 = DIRECTION ( 'NONE',  ( 1.043714542225393381E-14, -0.9350162426854158326, -0.3546048870425331789 ) ) ;
#10070 = CIRCLE ( 'NONE', #2521, 125.0000000000000000 ) ;
#10069 = DIRECTION ( 'NONE',  ( 0.2059786187410889424, 0.000000000000000000, 0.9785564922995060311 ) ) ;
#10071 = EDGE_LOOP ( 'NONE', ( #12466, #40388 ) ) ;
#10072 = LINE ( 'NONE', #38166, #8203 ) ;
#10073 = ORIENTED_EDGE ( 'NONE', *, *, #12722, .F. ) ;
#10074 = CARTESIAN_POINT ( 'NONE',  ( -149.3265790242249125, -175.3837268820161057, 72.15117186584559761 ) ) ;
#10075 = CARTESIAN_POINT ( 'NONE',  ( -48.47912675150885065, -183.6283474603465606, 6.938893903907228378E-15 ) ) ;
#10076 = ORIENTED_EDGE ( 'NONE', *, *, #21894, .T. ) ;
#10077 = CARTESIAN_POINT ( 'NONE',  ( -132.6364218684650211, -177.1207230881787780, 92.42591454022807795 ) ) ;
#10078 = ORIENTED_EDGE ( 'NONE', *, *, #34010, .T. ) ;
#10079 = DIRECTION ( 'NONE',  ( -0.9890401873221654760, 0.000000000000000000, 0.1476465640024710868 ) ) ;
#10080 = FACE_OUTER_BOUND ( 'NONE', #5909, .T. ) ;
#10081 = PLANE ( 'NONE',  #8453 ) ;
#10082 = EDGE_CURVE ( 'NONE', #28841, #17017, #24998, .T. ) ;
#10083 = EDGE_LOOP ( 'NONE', ( #14002, #34590, #40536, #12439 ) ) ;
#10084 = LINE ( 'NONE', #26099, #33607 ) ;
#10085 = CARTESIAN_POINT ( 'NONE',  ( -124.1938582159088043, -189.7472609257535510, -99.45993886622794378 ) ) ;
#10086 = CARTESIAN_POINT ( 'NONE',  ( -49.03777351731250889, -193.5000000000000000, 0.8294056854502042109 ) ) ;
#10087 = AXIS2_PLACEMENT_3D ( 'NONE', #21691, #13283, #1450 ) ;
#10088 = ORIENTED_EDGE ( 'NONE', *, *, #30159, .F. ) ;
#10089 = AXIS2_PLACEMENT_3D ( 'NONE', #38709, #50816, #14823 ) ;
#10090 = CARTESIAN_POINT ( 'NONE',  ( -330.4913330509368166, -103.0458197858332312, -55.34326076196081345 ) ) ;
#10091 = EDGE_LOOP ( 'NONE', ( #26263, #50478, #51324, #27982 ) ) ;
#10092 = FACE_OUTER_BOUND ( 'NONE', #29113, .T. ) ;
#10094 = EDGE_LOOP ( 'NONE', ( #15296, #6686, #45387, #7262 ) ) ;
#10093 = DIRECTION ( 'NONE',  ( -1.000000000000000000, -0.000000000000000000, -1.043714542225393381E-14 ) ) ;
#10095 = ORIENTED_EDGE ( 'NONE', *, *, #42716, .T. ) ;
#10096 = CARTESIAN_POINT ( 'NONE',  ( 61.06976976088564157, -175.3837268820161057, -60.19999396110172540 ) ) ;
#10097 = CARTESIAN_POINT ( 'NONE',  ( 0.000000000000000000, -64.93017642821482127, -7.111664135064078351 ) ) ;
#10098 = VERTEX_POINT ( 'NONE', #9482 ) ;
#10099 = AXIS2_PLACEMENT_3D ( 'NONE', #17551, #46179, #26177 ) ;
#10100 = CARTESIAN_POINT ( 'NONE',  ( -165.6791976657750354, -175.3837268820161057, 40.49875167739065773 ) ) ;
#10101 = ORIENTED_EDGE ( 'NONE', *, *, #35030, .F. ) ;
#10102 = DIRECTION ( 'NONE',  ( -1.000000000000000000, 0.000000000000000000, 0.000000000000000000 ) ) ;
#10103 = CARTESIAN_POINT ( 'NONE',  ( -80.85382946868864451, -177.1207230881787780, 119.6996507684852844 ) ) ;
#10104 = EDGE_CURVE ( 'NONE', #9678, #20898, #19061, .T. ) ;
#10105 = LINE ( 'NONE', #5398, #32788 ) ;
#10106 = CARTESIAN_POINT ( 'NONE',  ( -170.0000000000000284, -173.5000000000000284, -60.00000000000001421 ) ) ;
#10107 = ORIENTED_EDGE ( 'NONE', *, *, #6643, .F. ) ;
#10108 = ORIENTED_EDGE ( 'NONE', *, *, #47440, .T. ) ;
#10109 = ORIENTED_EDGE ( 'NONE', *, *, #24077, .T. ) ;
#10110 = EDGE_CURVE ( 'NONE', #14029, #32415, #42046, .T. ) ;
#10111 = DIRECTION ( 'NONE',  ( 0.000000000000000000, -1.000000000000000000, 0.000000000000000000 ) ) ;
#10112 = DIRECTION ( 'NONE',  ( 0.000000000000000000, 0.000000000000000000, 1.000000000000000000 ) ) ;
#10113 = CARTESIAN_POINT ( 'NONE',  ( -48.47912675150885065, -189.7472609257535510, 6.938893903907228378E-15 ) ) ;
#10114 = CARTESIAN_POINT ( 'NONE',  ( 30.00000000000000711, 0.000000000000000000, -30.00000000000000355 ) ) ;
#10115 = VERTEX_POINT ( 'NONE', #36821 ) ;
#10116 = EDGE_CURVE ( 'NONE', #19768, #35535, #33898, .T. ) ;
#10117 = CARTESIAN_POINT ( 'NONE',  ( -152.8713435144644848, -193.5000000000000000, -68.75510947788595217 ) ) ;
#10118 = EDGE_CURVE ( 'NONE', #10459, #24955, #21307, .T. ) ;
#10119 = AXIS2_PLACEMENT_3D ( 'NONE', #19231, #35239, #23172 ) ;
#10120 = VECTOR ( 'NONE', #12125, 1000.000000000000000 ) ;
#10121 = VERTEX_POINT ( 'NONE', #16858 ) ;
#10123 = VERTEX_POINT ( 'NONE', #37066 ) ;
#10122 = CARTESIAN_POINT ( 'NONE',  ( -339.1964088526558498, -183.1207326066167695, -6.735595255826207328 ) ) ;
#10124 = CARTESIAN_POINT ( 'NONE',  ( -330.4913330509368166, -123.5000000000000284, 0.000000000000000000 ) ) ;
#10125 = EDGE_CURVE ( 'NONE', #14296, #20982, #45489, .T. ) ;
#10126 = CARTESIAN_POINT ( 'NONE',  ( -95.72791768350688812, -177.1207230881787780, -115.7261930397105232 ) ) ;
#10127 = CARTESIAN_POINT ( 'NONE',  ( -23.01747912075237679, -183.6283474603465606, -122.3793467049370776 ) ) ;
#10128 = DIRECTION ( 'NONE',  ( 1.000000000000000000, 0.000000000000000000, 0.000000000000000000 ) ) ;
#10129 = CARTESIAN_POINT ( 'NONE',  ( -305.0000000000000568, -129.1091364105427033, 59.73723787327234191 ) ) ;
#10130 = VERTEX_POINT ( 'NONE', #28914 ) ;
#10131 = FACE_OUTER_BOUND ( 'NONE', #35293, .T. ) ;
#10132 = VERTEX_POINT ( 'NONE', #41521 ) ;
#10133 = VERTEX_POINT ( 'NONE', #1603 ) ;
#10134 = FACE_OUTER_BOUND ( 'NONE', #39211, .T. ) ;
#10135 = PLANE ( 'NONE',  #11861 ) ;
#10136 = EDGE_CURVE ( 'NONE', #15154, #26719, #44975, .T. ) ;
#10137 = ORIENTED_EDGE ( 'NONE', *, *, #13166, .F. ) ;
#10138 = CARTESIAN_POINT ( 'NONE',  ( -103.4012653778457462, -183.6283474603465606, -112.2878385610366649 ) ) ;
#10139 = CARTESIAN_POINT ( 'NONE',  ( -18.31235070009513777, -175.3837268820161057, 121.3052580173829824 ) ) ;
#10140 = DIRECTION ( 'NONE',  ( -1.000000000000000000, -0.000000000000000000, 0.000000000000000000 ) ) ;
#10141 = PLANE ( 'NONE',  #29903 ) ;
#10142 = CARTESIAN_POINT ( 'NONE',  ( 75.43907105790114542, -175.3837268820161057, -4.503971736580769658 ) ) ;
#10143 = ORIENTED_EDGE ( 'NONE', *, *, #28179, .F. ) ;
#10144 = CARTESIAN_POINT ( 'NONE',  ( 38.71172987070728055, -175.3837268820161057, -89.56983042009262874 ) ) ;
#10145 = VERTEX_POINT ( 'NONE', #41801 ) ;
#10146 = VECTOR ( 'NONE', #29718, 1000.000000000000000 ) ;
#10147 = VERTEX_POINT ( 'NONE', #21047 ) ;
#10148 = CARTESIAN_POINT ( 'NONE',  ( 49.27559354810669845, -183.6283474603465606, -76.29032973288636299 ) ) ;
#10149 = ORIENTED_EDGE ( 'NONE', *, *, #12695, .F. ) ;
#10150 = AXIS2_PLACEMENT_3D ( 'NONE', #4459, #36784, #20476 ) ;
#10151 = PLANE ( 'NONE',  #34372 ) ;
#10152 = PLANE ( 'NONE',  #32650 ) ;
#10154 = EDGE_LOOP ( 'NONE', ( #35297, #17908, #42733, #46513 ) ) ;
#10153 = FACE_OUTER_BOUND ( 'NONE', #45646, .T. ) ;
#10155 = ORIENTED_EDGE ( 'NONE', *, *, #40831, .T. ) ;
#10156 = DIRECTION ( 'NONE',  ( 0.7948544414133481562, 0.000000000000000000, 0.6068001458186002006 ) ) ;
#10157 = EDGE_CURVE ( 'NONE', #42041, #45184, #5291, .T. ) ;
#10158 = EDGE_CURVE ( 'NONE', #13339, #45638, #29186, .T. ) ;
#10159 = DIRECTION ( 'NONE',  ( 0.000000000000000000, -1.000000000000000000, -0.000000000000000000 ) ) ;
#10160 = LINE ( 'NONE', #5969, #505 ) ;
#10161 = ORIENTED_EDGE ( 'NONE', *, *, #27431, .T. ) ;
#10162 = VERTEX_POINT ( 'NONE', #50720 ) ;
#10163 = ORIENTED_EDGE ( 'NONE', *, *, #14322, .F. ) ;
#10164 = PLANE ( 'NONE',  #15863 ) ;
#10165 = DIRECTION ( 'NONE',  ( -0.9890401873221644768, 0.000000000000000000, 0.1476465640024779702 ) ) ;
#10166 = AXIS2_PLACEMENT_3D ( 'NONE', #36596, #51598, #326 ) ;
#10167 = DIRECTION ( 'NONE',  ( -1.000000000000000000, 0.000000000000000000, -0.000000000000000000 ) ) ;
#10168 = CARTESIAN_POINT ( 'NONE',  ( -305.0000000000000568, -162.9117225908387070, 45.24064679492076380 ) ) ;
#10169 = LINE ( 'NONE', #5980, #30558 ) ;
#10170 = VERTEX_POINT ( 'NONE', #18143 ) ;
#10171 = ADVANCED_FACE ( 'NONE', ( #51243 ), #14209, .T. ) ;
#10172 = EDGE_CURVE ( 'NONE', #30279, #39399, #45934, .T. ) ;
#10173 = DIRECTION ( 'NONE',  ( 0.6300878435817038881, 0.000000000000000000, 0.7765238627180482966 ) ) ;
#10174 = VERTEX_POINT ( 'NONE', #22607 ) ;
#10176 = ORIENTED_EDGE ( 'NONE', *, *, #13884, .T. ) ;
#10175 = LINE ( 'NONE', #45674, #31486 ) ;
#10177 = VERTEX_POINT ( 'NONE', #10497 ) ;
#10178 = ADVANCED_FACE ( 'NONE', ( #50989 ), #26530, .T. ) ;
#10179 = DIRECTION ( 'NONE',  ( 0.000000000000000000, 1.000000000000000000, -1.156482317317871232E-16 ) ) ;
#10180 = VERTEX_POINT ( 'NONE', #11267 ) ;
#10181 = CARTESIAN_POINT ( 'NONE',  ( -339.1964088526558498, -68.15673923803930734, -20.45418021416698551 ) ) ;
#10182 = CIRCLE ( 'NONE', #2643, 125.0000000000000000 ) ;
#10183 = EDGE_LOOP ( 'NONE', ( #5224, #40217, #37398, #23598 ) ) ;
#10184 = EDGE_CURVE ( 'NONE', #6892, #1866, #22855, .T. ) ;
#10185 = DIRECTION ( 'NONE',  ( 0.000000000000000000, 0.000000000000000000, 1.000000000000000000 ) ) ;
#10186 = CARTESIAN_POINT ( 'NONE',  ( -8.461066480258370603, -177.1207230881787780, 117.3655938605930231 ) ) ;
#10187 = VERTEX_POINT ( 'NONE', #22076 ) ;
#10188 = DIRECTION ( 'NONE',  ( -0.9720229140804139689, 0.000000000000000000, 0.2348860457809708036 ) ) ;
#10189 = EDGE_LOOP ( 'NONE', ( #37011, #31868, #1008, #4724 ) ) ;
#10190 = VECTOR ( 'NONE', #2710, 1000.000000000000000 ) ;
#10191 = ORIENTED_EDGE ( 'NONE', *, *, #47518, .T. ) ;
#10192 = DIRECTION ( 'NONE',  ( 0.4031234292879730674, 0.000000000000000000, -0.9151456172430181280 ) ) ;
#10193 = PLANE ( 'NONE',  #19000 ) ;
#10194 = CARTESIAN_POINT ( 'NONE',  ( -48.47912675150885065, -193.5000000000000000, 6.938893903907228378E-15 ) ) ;
#10195 = EDGE_LOOP ( 'NONE', ( #32726, #50782, #19623, #13226 ) ) ;
#10196 = DIRECTION ( 'NONE',  ( 0.1476465640024710868, 0.000000000000000000, 0.9890401873221654760 ) ) ;
#10197 = FACE_OUTER_BOUND ( 'NONE', #37361, .T. ) ;
#10198 = CONTEXT_DEPENDENT_SHAPE_REPRESENTATION ( #28655, #22678 ) ;
#10199 = DIRECTION ( 'NONE',  ( 0.000000000000000000, 0.000000000000000000, 1.000000000000000000 ) ) ;
#10200 = LINE ( 'NONE', #37795, #18650 ) ;
#10201 = EDGE_LOOP ( 'NONE', ( #8728, #36120, #4406, #20556 ) ) ;
#10202 = DIRECTION ( 'NONE',  ( 0.000000000000000000, 0.3546048870425267951, -0.9350162426854181641 ) ) ;
#10203 = CARTESIAN_POINT ( 'NONE',  ( 11.52087324849114580, -132.5479369270331915, -60.00000000000002842 ) ) ;
#10204 = AXIS2_PLACEMENT_3D ( 'NONE', #24556, #28238, #9065 ) ;
#10205 = CARTESIAN_POINT ( 'NONE',  ( -48.47912675150885065, -177.1207230881787780, 6.938893903907228378E-15 ) ) ;
#10206 = ORIENTED_EDGE ( 'NONE', *, *, #7612, .T. ) ;
#10207 = VECTOR ( 'NONE', #21749, 1000.000000000000114 ) ;
#10208 = DIRECTION ( 'NONE',  ( 0.000000000000000000, 0.000000000000000000, 1.000000000000000000 ) ) ;
#10209 = DIRECTION ( 'NONE',  ( 0.000000000000000000, -0.000000000000000000, 1.000000000000000000 ) ) ;
#10210 = VERTEX_POINT ( 'NONE', #38874 ) ;
#10211 = CARTESIAN_POINT ( 'NONE',  ( -330.4913330509368166, -95.63860483659048839, 52.00954392751722111 ) ) ;
#10212 = ORIENTED_EDGE ( 'NONE', *, *, #19759, .T. ) ;
#10213 = EDGE_CURVE ( 'NONE', #25533, #47448, #39188, .T. ) ;
#10214 = CARTESIAN_POINT ( 'NONE',  ( -305.0000000000000568, -183.1207326066166559, 6.735595255827129257 ) ) ;
#10215 = LINE ( 'NONE', #34398, #49707 ) ;
#10216 = CARTESIAN_POINT ( 'NONE',  ( -339.1964088526558498, -75.22798428563942252, 33.92731199008440512 ) ) ;
#10217 = VECTOR ( 'NONE', #17393, 1000.000000000000000 ) ;
#10218 = EDGE_CURVE ( 'NONE', #28909, #5759, #3141, .T. ) ;
#10219 = EDGE_CURVE ( 'NONE', #49982, #48449, #15232, .T. ) ;
#10220 = LINE ( 'NONE', #10743, #24971 ) ;
#10221 = EDGE_CURVE ( 'NONE', #9326, #6776, #31246, .T. ) ;
#10222 = CIRCLE ( 'NONE', #41238, 60.00000000000000000 ) ;
#10223 = CARTESIAN_POINT ( 'NONE',  ( -47.64924157374594671, -193.5000000000000000, 124.9972451320097377 ) ) ;
#10224 = ORIENTED_EDGE ( 'NONE', *, *, #14789, .F. ) ;
#10225 = EDGE_CURVE ( 'NONE', #8474, #42568, #34169, .T. ) ;
#10226 = CIRCLE ( 'NONE', #39582, 125.0000000000000000 ) ;
#10227 = DIRECTION ( 'NONE',  ( 0.5829794791144650157, 0.000000000000000000, 0.8124868780056864193 ) ) ;
#10228 = ORIENTED_EDGE ( 'NONE', *, *, #6275, .T. ) ;
#10229 = LINE ( 'NONE', #26248, #2397 ) ;
#10230 = VERTEX_POINT ( 'NONE', #47037 ) ;
#10231 = ADVANCED_FACE ( 'NONE', ( #38364 ), #14464, .T. ) ;
#10232 = CARTESIAN_POINT ( 'NONE',  ( -41.30311180514221547, -193.5000000000000000, 123.7921848946937899 ) ) ;
#10233 = ADVANCED_FACE ( 'NONE', ( #10251 ), #23118, .F. ) ;
#10234 = VECTOR ( 'NONE', #41620, 1000.000000000000000 ) ;
#10235 = EDGE_CURVE ( 'NONE', #42695, #37425, #29971, .T. ) ;
#10236 = CARTESIAN_POINT ( 'NONE',  ( -339.1964088526558498, -68.51134412508183402, -21.38919645685240312 ) ) ;
#10237 = LINE ( 'NONE', #34662, #13885 ) ;
#10238 = ORIENTED_EDGE ( 'NONE', *, *, #20828, .F. ) ;
#10241 = EDGE_LOOP ( 'NONE', ( #32459, #44604, #31159, #47780 ) ) ;
#10240 = LINE ( 'NONE', #1317, #36511 ) ;
#10239 = DIRECTION ( 'NONE',  ( -1.000000000000000000, 0.000000000000000000, 0.000000000000000000 ) ) ;
#10242 = AXIS2_PLACEMENT_3D ( 'NONE', #39801, #19344, #35884 ) ;
#10243 = AXIS2_PLACEMENT_3D ( 'NONE', #46644, #46908, #22717 ) ;
#10244 = EDGE_CURVE ( 'NONE', #36752, #20294, #1425, .T. ) ;
#10245 = DIRECTION ( 'NONE',  ( 0.000000000000000000, 1.000000000000000000, 0.000000000000000000 ) ) ;
#10246 = ORIENTED_EDGE ( 'NONE', *, *, #18740, .F. ) ;
#10247 = CARTESIAN_POINT ( 'NONE',  ( -336.3521761649654422, -154.8494888031386836, 50.05135858667791382 ) ) ;
#10248 = ORIENTED_EDGE ( 'NONE', *, *, #41678, .F. ) ;
#10249 = EDGE_CURVE ( 'NONE', #29042, #39776, #34672, .T. ) ;
#10250 = DIRECTION ( 'NONE',  ( -0.000000000000000000, 1.000000000000000000, -0.000000000000000000 ) ) ;
#10253 = ORIENTED_EDGE ( 'NONE', *, *, #2819, .T. ) ;
#10252 = FACE_OUTER_BOUND ( 'NONE', #35603, .T. ) ;
#10251 = FACE_OUTER_BOUND ( 'NONE', #49541, .T. ) ;
#10254 = ORIENTED_EDGE ( 'NONE', *, *, #26896, .F. ) ;
#10255 = ADVANCED_FACE ( 'NONE', ( #39130 ), #43080, .F. ) ;
#10256 = EDGE_CURVE ( 'NONE', #17894, #39559, #5647, .T. ) ;
#10257 = CARTESIAN_POINT ( 'NONE',  ( 53.18081239921338010, -189.7472609257535510, -72.73415134495935774 ) ) ;
#10258 = EDGE_LOOP ( 'NONE', ( #29017, #14513, #35786, #7480 ) ) ;
#10259 = CARTESIAN_POINT ( 'NONE',  ( -332.3517673607765914, -63.55776901541228341, -2.632288850093980503 ) ) ;
#10260 = CARTESIAN_POINT ( 'NONE',  ( -114.1105527140175155, -193.5000000000000000, 106.3838142112217611 ) ) ;
#10261 = ORIENTED_EDGE ( 'NONE', *, *, #35779, .T. ) ;
#10262 = DIRECTION ( 'NONE',  ( -0.000000000000000000, 1.000000000000000000, -0.000000000000000000 ) ) ;
#10263 = PLANE ( 'NONE',  #15767 ) ;
#10264 = DIRECTION ( 'NONE',  ( 0.000000000000000000, 7.632783294297951215E-14, -1.000000000000000000 ) ) ;
#10265 = CARTESIAN_POINT ( 'NONE',  ( -339.1964088526558498, -64.99044476834248485, -7.608018572113150135 ) ) ;
#10266 = VECTOR ( 'NONE', #30415, 1000.000000000000227 ) ;
#10267 = DIRECTION ( 'NONE',  ( 0.000000000000000000, 0.000000000000000000, -1.000000000000000000 ) ) ;
#10268 = ORIENTED_EDGE ( 'NONE', *, *, #20343, .T. ) ;
#10269 = CARTESIAN_POINT ( 'NONE',  ( 51.65665342072240662, -183.6283474603465606, 74.81861753132422166 ) ) ;
#10270 = EDGE_CURVE ( 'NONE', #34518, #18747, #33309, .T. ) ;
#10271 = PLANE ( 'NONE',  #13101 ) ;
#10272 = VECTOR ( 'NONE', #10469, 1000.000000000000114 ) ;
#10273 = FACE_OUTER_BOUND ( 'NONE', #7837, .T. ) ;
#10274 = ORIENTED_EDGE ( 'NONE', *, *, #11877, .T. ) ;
#10275 = LINE ( 'NONE', #6848, #24811 ) ;
#10276 = LINE ( 'NONE', #34446, #28627 ) ;
#10277 = PLANE ( 'NONE',  #14359 ) ;
#10278 = PLANE ( 'NONE',  #42543 ) ;
#10279 = VECTOR ( 'NONE', #40452, 1000.000000000000000 ) ;
#10280 = VECTOR ( 'NONE', #43209, 1000.000000000000000 ) ;
#10281 = DIRECTION ( 'NONE',  ( -0.000000000000000000, 1.000000000000000000, -0.000000000000000000 ) ) ;
#10282 = VECTOR ( 'NONE', #7805, 999.9999999999998863 ) ;
#10283 = VECTOR ( 'NONE', #30586, 1000.000000000000000 ) ;
#10284 = PLANE ( 'NONE',  #6037 ) ;
#10285 = CARTESIAN_POINT ( 'NONE',  ( 71.87891646118019651, -175.3837268820161057, -33.74820638215424395 ) ) ;
#10286 = CARTESIAN_POINT ( 'NONE',  ( -108.4791267515088435, -132.5479369270331915, -186.7953921478704729 ) ) ;
#10287 = ORIENTED_EDGE ( 'NONE', *, *, #22770, .T. ) ;
#10288 = EDGE_CURVE ( 'NONE', #44335, #4324, #36224, .T. ) ;
#10289 = ADVANCED_FACE ( 'NONE', ( #7596 ), #39893, .F. ) ;
#10290 = LINE ( 'NONE', #26311, #45343 ) ;
#10291 = ADVANCED_FACE ( 'NONE', ( #7850 ), #16263, .T. ) ;
#10292 = ADVANCED_FACE ( 'NONE', ( #28340 ), #27569, .F. ) ;
#10293 = LINE ( 'NONE', #34711, #2836 ) ;
#10295 = ORIENTED_EDGE ( 'NONE', *, *, #49794, .F. ) ;
#10294 = DIRECTION ( 'NONE',  ( -1.000000000000000000, 0.000000000000000000, 0.000000000000000000 ) ) ;
#10296 = ORIENTED_EDGE ( 'NONE', *, *, #25440, .T. ) ;
#10297 = ORIENTED_EDGE ( 'NONE', *, *, #10584, .T. ) ;
#10298 = DIRECTION ( 'NONE',  ( -0.000000000000000000, 1.000000000000000000, -0.000000000000000000 ) ) ;
#10299 = AXIS2_PLACEMENT_3D ( 'NONE', #40886, #16994, #33002 ) ;
#10300 = CARTESIAN_POINT ( 'NONE',  ( -49.47868758801764955, -189.7472609257535510, -0.02963332782256313663 ) ) ;
#10301 = DIRECTION ( 'NONE',  ( 0.2348860457809911206, 0.000000000000000000, -0.9720229140804089729 ) ) ;
#10302 = ORIENTED_EDGE ( 'NONE', *, *, #38879, .F. ) ;
#10303 = VECTOR ( 'NONE', #46302, 999.9999999999998863 ) ;
#10304 = DIRECTION ( 'NONE',  ( 0.9027978299657416494, 0.000000000000000000, 0.4300652022765245608 ) ) ;
#10305 = DIRECTION ( 'NONE',  ( -0.9785564922995060311, 0.000000000000000000, 0.2059786187410889424 ) ) ;
#10308 = VERTEX_POINT ( 'NONE', #39386 ) ;
#10307 = PLANE ( 'NONE',  #3132 ) ;
#10306 = FACE_OUTER_BOUND ( 'NONE', #47351, .T. ) ;
#10309 = ADVANCED_FACE ( 'NONE', ( #43601 ), #3649, .F. ) ;
#10310 = DIRECTION ( 'NONE',  ( 0.000000000000000000, 0.000000000000000000, -1.000000000000000000 ) ) ;
#10311 = EDGE_LOOP ( 'NONE', ( #2525, #46067, #51159, #5322 ) ) ;
#10312 = DIRECTION ( 'NONE',  ( -0.000000000000000000, 1.000000000000000000, -0.000000000000000000 ) ) ;
#10313 = ORIENTED_EDGE ( 'NONE', *, *, #26481, .T. ) ;
#10314 = DIRECTION ( 'NONE',  ( 0.000000000000000000, 1.000000000000000000, -1.047444401652940007E-14 ) ) ;
#10315 = LINE ( 'NONE', #50528, #23778 ) ;
#10316 = CYLINDRICAL_SURFACE ( 'NONE', #44185, 125.0000000000000000 ) ;
#10317 = VECTOR ( 'NONE', #44365, 1000.000000000000000 ) ;
#10318 = EDGE_CURVE ( 'NONE', #26071, #43135, #12328, .T. ) ;
#10319 = CIRCLE ( 'NONE', #1084, 125.0000000000000000 ) ;
#10320 = ORIENTED_EDGE ( 'NONE', *, *, #11231, .F. ) ;
#10321 = AXIS2_PLACEMENT_3D ( 'NONE', #31812, #51273, #34962 ) ;
#10322 = CARTESIAN_POINT ( 'NONE',  ( -120.5074237604784457, -193.5000000000000000, 100.9358816284415639 ) ) ;
#10323 = DIRECTION ( 'NONE',  ( 0.05924062789372142729, 0.000000000000000000, -0.9982437317643209074 ) ) ;
#10324 = EDGE_LOOP ( 'NONE', ( #38651, #16401, #41665, #28171 ) ) ;
#10325 = DIRECTION ( 'NONE',  ( -0.7948544414133608127, 0.000000000000000000, 0.6068001458185834363 ) ) ;
#10326 = CARTESIAN_POINT ( 'NONE',  ( 74.18685885783125400, -175.3837268820161057, -18.13990644964003351 ) ) ;
#10327 = VERTEX_POINT ( 'NONE', #44392 ) ;
#10328 = FACE_BOUND ( 'NONE', #44890, .T. ) ;
#10329 = PLANE ( 'NONE',  #13053 ) ;
#10330 = ORIENTED_EDGE ( 'NONE', *, *, #34271, .T. ) ;
#10331 = DIRECTION ( 'NONE',  ( -0.000000000000000000, 1.000000000000000000, -0.000000000000000000 ) ) ;
#10332 = ORIENTED_EDGE ( 'NONE', *, *, #24055, .T. ) ;
#10333 = DIRECTION ( 'NONE',  ( 0.000000000000000000, 0.000000000000000000, -1.000000000000000000 ) ) ;
#10334 = LINE ( 'NONE', #14547, #5213 ) ;
#10335 = ORIENTED_EDGE ( 'NONE', *, *, #16828, .F. ) ;
#10336 = AXIS2_PLACEMENT_3D ( 'NONE', #19323, #23769, #35584 ) ;
#10337 = CARTESIAN_POINT ( 'NONE',  ( -67.22356632362124174, -193.5000000000000000, -123.5865930638409509 ) ) ;
#10338 = DIRECTION ( 'NONE',  ( 0.000000000000000000, -1.000000000000000000, -0.000000000000000000 ) ) ;
#10339 = PLANE ( 'NONE',  #30768 ) ;
#10340 = CIRCLE ( 'NONE', #17078, 125.0000000000000000 ) ;
#10341 = ORIENTED_EDGE ( 'NONE', *, *, #35058, .F. ) ;
#10342 = LINE ( 'NONE', #41615, #33799 ) ;
#10343 = ORIENTED_EDGE ( 'NONE', *, *, #3239, .F. ) ;
#10344 = FACE_OUTER_BOUND ( 'NONE', #46322, .T. ) ;
#10345 = FACE_OUTER_BOUND ( 'NONE', #27545, .T. ) ;
#10347 = ORIENTED_EDGE ( 'NONE', *, *, #26937, .T. ) ;
#10346 = CARTESIAN_POINT ( 'NONE',  ( -332.3517673607765914, -92.15051119686104641, -50.05135858667769355 ) ) ;
#10348 = EDGE_LOOP ( 'NONE', ( #9536, #13626, #37701, #9879 ) ) ;
#10349 = EDGE_CURVE ( 'NONE', #20987, #35554, #8167, .T. ) ;
#10350 = CARTESIAN_POINT ( 'NONE',  ( 73.32083127613157103, -177.1207230881787780, 28.10285082451656535 ) ) ;
#10351 = AXIS2_PLACEMENT_3D ( 'NONE', #21854, #6081, #42067 ) ;
#10352 = CARTESIAN_POINT ( 'NONE',  ( -173.2765435274470178, -183.6283474603465606, -7.113702696401515979 ) ) ;
#10353 = VECTOR ( 'NONE', #43691, 1000.000000000000000 ) ;
#10354 = ORIENTED_EDGE ( 'NONE', *, *, #39749, .F. ) ;
#10355 = DIRECTION ( 'NONE',  ( 0.000000000000000000, 0.000000000000000000, 1.000000000000000000 ) ) ;
#10356 = EDGE_LOOP ( 'NONE', ( #24313, #24164, #49378, #34675, #49345, #52015, #40532, #11783 ) ) ;
#10357 = LINE ( 'NONE', #1958, #51844 ) ;
#10358 = CARTESIAN_POINT ( 'NONE',  ( 48.33059356687145680, -193.5000000000000000, 77.48473115145309009 ) ) ;
#10359 = VECTOR ( 'NONE', #49067, 1000.000000000000114 ) ;
#10360 = FACE_OUTER_BOUND ( 'NONE', #15347, .T. ) ;
#10361 = DIRECTION ( 'NONE',  ( 0.000000000000000000, 0.000000000000000000, 1.000000000000000000 ) ) ;
#10362 = ORIENTED_EDGE ( 'NONE', *, *, #40743, .F. ) ;
#10363 = ORIENTED_EDGE ( 'NONE', *, *, #12192, .F. ) ;
#10364 = ORIENTED_EDGE ( 'NONE', *, *, #40280, .F. ) ;
#10365 = FACE_OUTER_BOUND ( 'NONE', #38556, .T. ) ;
#10366 = DIRECTION ( 'NONE',  ( 0.000000000000000000, 0.000000000000000000, -1.000000000000000000 ) ) ;
#10367 = EDGE_CURVE ( 'NONE', #2629, #45033, #4439, .T. ) ;
#10368 = CARTESIAN_POINT ( 'NONE',  ( -173.4190745413846741, -189.7472609257535510, -3.874202661595026687 ) ) ;
#10369 = DIRECTION ( 'NONE',  ( 0.000000000000000000, 1.000000000000000000, 0.000000000000000000 ) ) ;
#10370 = AXIS2_PLACEMENT_3D ( 'NONE', #51386, #39527, #31654 ) ;
#10371 = ORIENTED_EDGE ( 'NONE', *, *, #44869, .T. ) ;
#10372 = DIRECTION ( 'NONE',  ( -0.000000000000000000, 1.000000000000000000, -0.000000000000000000 ) ) ;
#10373 = VECTOR ( 'NONE', #18182, 1000.000000000000114 ) ;
#10374 = ORIENTED_EDGE ( 'NONE', *, *, #12712, .T. ) ;
#10375 = ORIENTED_EDGE ( 'NONE', *, *, #32035, .F. ) ;
#10376 = CARTESIAN_POINT ( 'NONE',  ( -19.92568551777507224, -175.3837268820161057, -121.6951149130962904 ) ) ;
#10377 = CARTESIAN_POINT ( 'NONE',  ( -128.2395503755045638, -193.5000000000000000, -96.24590808611419845 ) ) ;
#10378 = DIRECTION ( 'NONE',  ( 0.000000000000000000, 1.000000000000000000, 0.000000000000000000 ) ) ;
#10379 = LINE ( 'NONE', #1978, #1910 ) ;
#10380 = PLANE ( 'NONE',  #4132 ) ;
#10381 = VERTEX_POINT ( 'NONE', #15770 ) ;
#10383 = EDGE_CURVE ( 'NONE', #9092, #14259, #35978, .T. ) ;
#10382 = LINE ( 'NONE', #26406, #18368 ) ;
#10384 = VECTOR ( 'NONE', #14007, 1000.000000000000000 ) ;
#10385 = EDGE_LOOP ( 'NONE', ( #29483, #102, #51673, #51801 ) ) ;
#10386 = DIRECTION ( 'NONE',  ( 0.1182731709213660498, 0.000000000000000000, -0.9929810960135169173 ) ) ;
#10387 = ADVANCED_FACE ( 'NONE', ( #52029 ), #31779, .F. ) ;
#10388 = LINE ( 'NONE', #7228, #45463 ) ;
#10389 = EDGE_LOOP ( 'NONE', ( #37796, #17128, #25499, #49878 ) ) ;
#10390 = PLANE ( 'NONE',  #31527 ) ;
#10391 = DIRECTION ( 'NONE',  ( 0.000000000000000000, -2.201942332173227054E-13, -1.000000000000000000 ) ) ;
#10392 = CARTESIAN_POINT ( 'NONE',  ( -160.9694636715425702, -175.3837268820161057, 54.50618404931040573 ) ) ;
#10393 = LINE ( 'NONE', #46669, #5577 ) ;
#10394 = EDGE_CURVE ( 'NONE', #26301, #15638, #8380, .T. ) ;
#10395 = CARTESIAN_POINT ( 'NONE',  ( -83.89965873179622236, -193.5000000000000000, 118.8334608768482497 ) ) ;
#10396 = ORIENTED_EDGE ( 'NONE', *, *, #49158, .T. ) ;
#10397 = LINE ( 'NONE', #15140, #7571 ) ;
#10398 = ORIENTED_EDGE ( 'NONE', *, *, #22742, .T. ) ;
#10399 = VECTOR ( 'NONE', #51205, 1000.000000000000000 ) ;
#10400 = AXIS2_PLACEMENT_3D ( 'NONE', #9381, #36970, #17783 ) ;
#10401 = ORIENTED_EDGE ( 'NONE', *, *, #16996, .T. ) ;
#10402 = FACE_OUTER_BOUND ( 'NONE', #33728, .T. ) ;
#10403 = EDGE_CURVE ( 'NONE', #15221, #13319, #46786, .T. ) ;
#10404 = ORIENTED_EDGE ( 'NONE', *, *, #16599, .T. ) ;
#10405 = AXIS2_PLACEMENT_3D ( 'NONE', #17774, #29329, #21719 ) ;
#10406 = DIRECTION ( 'NONE',  ( 0.000000000000000000, -5.782411586589357402E-14, 1.000000000000000000 ) ) ;
#10407 = ADVANCED_FACE ( 'NONE', ( #40416 ), #20201, .T. ) ;
#10408 = ORIENTED_EDGE ( 'NONE', *, *, #5860, .F. ) ;
#10409 = FACE_OUTER_BOUND ( 'NONE', #3150, .T. ) ;
#10410 = DIRECTION ( 'NONE',  ( -0.000000000000000000, 0.7485107481710999711, -0.6631226582407964143 ) ) ;
#10411 = ORIENTED_EDGE ( 'NONE', *, *, #45908, .T. ) ;
#10412 = FACE_OUTER_BOUND ( 'NONE', #26476, .T. ) ;
#10414 = AXIS2_PLACEMENT_3D ( 'NONE', #50641, #22000, #14912 ) ;
#10413 = PLANE ( 'NONE',  #4245 ) ;
#10415 = DIRECTION ( 'NONE',  ( -0.6068001458185834363, 0.000000000000000000, -0.7948544414133608127 ) ) ;
#10416 = ORIENTED_EDGE ( 'NONE', *, *, #47228, .F. ) ;
#10417 = ORIENTED_EDGE ( 'NONE', *, *, #50246, .T. ) ;
#10418 = ORIENTED_EDGE ( 'NONE', *, *, #40655, .T. ) ;
#10419 = CARTESIAN_POINT ( 'NONE',  ( -170.5806857741408180, -193.5000000000000000, -21.61797988633145451 ) ) ;
#10420 = CARTESIAN_POINT ( 'NONE',  ( -173.4724443937511751, -177.1207230881787780, 1.292495564989516454 ) ) ;
#10421 = EDGE_CURVE ( 'NONE', #45486, #19065, #20456, .T. ) ;
#10422 = CARTESIAN_POINT ( 'NONE',  ( -48.47912675150885065, -177.1207230881787780, 6.938893903907228378E-15 ) ) ;
#10423 = CARTESIAN_POINT ( 'NONE',  ( -20.16057156355605784, -189.7472609257535510, -120.7230919990158782 ) ) ;
#10424 = ORIENTED_EDGE ( 'NONE', *, *, #29995, .T. ) ;
#10425 = ADVANCED_FACE ( 'NONE', ( #48600 ), #24662, .F. ) ;
#10426 = DIRECTION ( 'NONE',  ( 0.9646355819083614058, 0.000000000000000000, -0.2635871660690581320 ) ) ;
#10427 = ORIENTED_EDGE ( 'NONE', *, *, #13019, .F. ) ;
#10429 = ORIENTED_EDGE ( 'NONE', *, *, #1582, .F. ) ;
#10428 = LINE ( 'NONE', #2556, #2981 ) ;
#10430 = ORIENTED_EDGE ( 'NONE', *, *, #33174, .T. ) ;
#10431 = LINE ( 'NONE', #26458, #4821 ) ;
#10432 = ORIENTED_EDGE ( 'NONE', *, *, #34549, .F. ) ;
#10433 = PLANE ( 'NONE',  #45968 ) ;
#10434 = AXIS2_PLACEMENT_3D ( 'NONE', #4645, #36709, #9118 ) ;
#10435 = ORIENTED_EDGE ( 'NONE', *, *, #50050, .T. ) ;
#10436 = VECTOR ( 'NONE', #10781, 1000.000000000000000 ) ;
#10437 = CARTESIAN_POINT ( 'NONE',  ( -339.1964088526558498, -171.7720157143598669, 33.92731199008546383 ) ) ;
#10438 = DIRECTION ( 'NONE',  ( 0.000000000000000000, 1.249000902703301108E-14, -1.000000000000000000 ) ) ;
#10439 = VERTEX_POINT ( 'NONE', #8633 ) ;
#10440 = CARTESIAN_POINT ( 'NONE',  ( -95.72791768350688812, -193.5000000000000000, -115.7261930397105232 ) ) ;
#10441 = ORIENTED_EDGE ( 'NONE', *, *, #14304, .F. ) ;
#10442 = VECTOR ( 'NONE', #45831, 1000.000000000000000 ) ;
#10443 = EDGE_LOOP ( 'NONE', ( #1224, #8653, #6365, #47293 ) ) ;
#10444 = CARTESIAN_POINT ( 'NONE',  ( -336.3521761649654422, -169.4076645216271402, -37.15394033962039089 ) ) ;
#10445 = DIRECTION ( 'NONE',  ( 0.000000000000000000, 0.000000000000000000, -1.000000000000000000 ) ) ;
#10446 = CARTESIAN_POINT ( 'NONE',  ( -53.47502265695599277, -177.1207230881787780, -124.9001241957025883 ) ) ;
#10447 = ORIENTED_EDGE ( 'NONE', *, *, #30104, .T. ) ;
#10448 = DIRECTION ( 'NONE',  ( 1.000000000000000000, 0.000000000000000000, -0.000000000000000000 ) ) ;
#10449 = LINE ( 'NONE', #2330, #33998 ) ;
#10450 = EDGE_CURVE ( 'NONE', #31317, #34375, #47652, .T. ) ;
#10451 = EDGE_CURVE ( 'NONE', #40019, #43044, #20726, .T. ) ;
#10452 = ITEM_DEFINED_TRANSFORMATION ( 'NONE', 'NONE', #15851,  #31742 ) ;
#10453 = DIRECTION ( 'NONE',  ( -0.000000000000000000, 1.000000000000000000, -0.000000000000000000 ) ) ;
#10454 = CARTESIAN_POINT ( 'NONE',  ( 54.46899307705341187, -177.1207230881787780, -70.89911581792813422 ) ) ;
#10455 = VERTEX_POINT ( 'NONE', #44640 ) ;
#10456 = DIRECTION ( 'NONE',  ( 0.000000000000000000, 1.000000000000000000, -0.000000000000000000 ) ) ;
#10457 = DIRECTION ( 'NONE',  ( -0.000000000000000000, 1.000000000000000000, 0.000000000000000000 ) ) ;
#10458 = DIRECTION ( 'NONE',  ( 0.000000000000000000, 0.8854560256532157947, 0.4647231720437573488 ) ) ;
#10459 = VERTEX_POINT ( 'NONE', #38922 ) ;
#10460 = CARTESIAN_POINT ( 'NONE',  ( -170.8336150310144887, -193.5000000000000000, 25.58083653558494319 ) ) ;
#10461 = DIRECTION ( 'NONE',  ( 0.000000000000000000, 0.000000000000000000, 1.000000000000000000 ) ) ;
#10462 = ORIENTED_EDGE ( 'NONE', *, *, #42711, .T. ) ;
#10463 = DIRECTION ( 'NONE',  ( -1.000000000000000000, 0.000000000000000000, -0.000000000000000000 ) ) ;
#10464 = EDGE_CURVE ( 'NONE', #76, #7181, #15282, .T. ) ;
#10465 = EDGE_LOOP ( 'NONE', ( #38724, #20304, #21029, #24277 ) ) ;
#10466 = EDGE_CURVE ( 'NONE', #7849, #51485, #14907, .T. ) ;
#10467 = ADVANCED_FACE ( 'NONE', ( #10306 ), #34992, .F. ) ;
#10468 = VECTOR ( 'NONE', #44649, 1000.000000000000000 ) ;
#10469 = DIRECTION ( 'NONE',  ( -0.7765238627180482966, 0.000000000000000000, 0.6300878435817038881 ) ) ;
#10470 = CARTESIAN_POINT ( 'NONE',  ( -47.53180039765465636, -183.6283474603465606, -0.3202698538628280800 ) ) ;
#10471 = VECTOR ( 'NONE', #51819, 999.9999999999998863 ) ;
#10472 = EDGE_CURVE ( 'NONE', #48687, #8761, #10687, .T. ) ;
#10473 = VECTOR ( 'NONE', #42135, 1000.000000000000227 ) ;
#10474 = LINE ( 'NONE', #34141, #40891 ) ;
#10475 = FACE_OUTER_BOUND ( 'NONE', #26639, .T. ) ;
#10476 = ORIENTED_EDGE ( 'NONE', *, *, #32585, .T. ) ;
#10477 = CIRCLE ( 'NONE', #22226, 60.00000000000000000 ) ;
#10478 = FACE_OUTER_BOUND ( 'NONE', #29262, .T. ) ;
#10479 = ORIENTED_EDGE ( 'NONE', *, *, #36626, .F. ) ;
#10480 = CARTESIAN_POINT ( 'NONE',  ( -332.3517673607765914, -169.4764303083190384, -38.55084767037274673 ) ) ;
#10481 = ORIENTED_EDGE ( 'NONE', *, *, #12788, .F. ) ;
#10482 = VECTOR ( 'NONE', #28059, 1000.000000000000114 ) ;
#10483 = PLANE ( 'NONE',  #4941 ) ;
#10484 = AXIS2_PLACEMENT_3D ( 'NONE', #50056, #21406, #1437 ) ;
#10485 = AXIS2_PLACEMENT_3D ( 'NONE', #9023, #41578, #48453 ) ;
#10486 = LINE ( 'NONE', #6046, #12454 ) ;
#10487 = CARTESIAN_POINT ( 'NONE',  ( -330.4913330509368166, -115.8919814278863356, 58.50955523165747252 ) ) ;
#10488 = ORIENTED_EDGE ( 'NONE', *, *, #42366, .F. ) ;
#10491 = ORIENTED_EDGE ( 'NONE', *, *, #27428, .T. ) ;
#10490 = DIRECTION ( 'NONE',  ( 0.000000000000000000, 0.000000000000000000, 1.000000000000000000 ) ) ;
#10489 = LINE ( 'NONE', #18897, #13281 ) ;
#10492 = DIRECTION ( 'NONE',  ( -8.718379230999708359E-17, -0.2393156642875449158, 0.9709418174260553425 ) ) ;
#10493 = EDGE_LOOP ( 'NONE', ( #23481, #104, #46016, #41854 ) ) ;
#10494 = CARTESIAN_POINT ( 'NONE',  ( -330.4913330509368166, -182.5000000000000568, -0.4999999999999551470 ) ) ;
#10495 = ORIENTED_EDGE ( 'NONE', *, *, #21766, .F. ) ;
#10496 = DIRECTION ( 'NONE',  ( 0.000000000000000000, -1.000000000000000000, 0.000000000000000000 ) ) ;
#10499 = VERTEX_POINT ( 'NONE', #30792 ) ;
#10498 = CARTESIAN_POINT ( 'NONE',  ( -48.30901192927175458, -193.5000000000000000, -124.9998842437354227 ) ) ;
#10497 = CARTESIAN_POINT ( 'NONE',  ( -152.0588566364587848, -183.6283474603465606, -68.17212999877148150 ) ) ;
#10500 = EDGE_LOOP ( 'NONE', ( #48122, #16460, #43190, #2038 ) ) ;
#10501 = LINE ( 'NONE', #34428, #16471 ) ;
#10502 = EDGE_LOOP ( 'NONE', ( #13287, #24330, #25751, #42278 ) ) ;
#10503 = FACE_OUTER_BOUND ( 'NONE', #38385, .T. ) ;
#10504 = VECTOR ( 'NONE', #31581, 1000.000000000000000 ) ;
#10505 = CARTESIAN_POINT ( 'NONE',  ( 35.67816836544800907, -193.5000000000000000, -92.42591454022745268 ) ) ;
#10506 = EDGE_LOOP ( 'NONE', ( #36362, #41438, #6048, #7514 ) ) ;
#10507 = LINE ( 'NONE', #22616, #33100 ) ;
#10508 = LINE ( 'NONE', #6595, #10724 ) ;
#10509 = FACE_OUTER_BOUND ( 'NONE', #13877, .T. ) ;
#10510 = DIRECTION ( 'NONE',  ( 0.000000000000000000, 0.000000000000000000, 1.000000000000000000 ) ) ;
#10511 = AXIS2_PLACEMENT_3D ( 'NONE', #9162, #44633, #25189 ) ;
#10512 = FACE_OUTER_BOUND ( 'NONE', #32584, .T. ) ;
#10513 = AXIS2_PLACEMENT_3D ( 'NONE', #6785, #2049, #26478 ) ;
#10514 = EDGE_CURVE ( 'NONE', #40054, #18957, #43129, .T. ) ;
#10515 = ADVANCED_FACE ( 'NONE', ( #6636 ), #23173, .F. ) ;
#10516 = ORIENTED_EDGE ( 'NONE', *, *, #16352, .F. ) ;
#10517 = EDGE_CURVE ( 'NONE', #16252, #17485, #50773, .T. ) ;
#10518 = CARTESIAN_POINT ( 'NONE',  ( -336.3521761649654422, -166.5797264208035244, 40.34602258462248159 ) ) ;
#10520 = AXIS2_PLACEMENT_3D ( 'NONE', #22753, #39020, #26423 ) ;
#10519 = DIRECTION ( 'NONE',  ( -0.000000000000000000, 1.000000000000000000, -0.000000000000000000 ) ) ;
#10521 = EDGE_CURVE ( 'NONE', #11143, #41973, #46836, .T. ) ;
#10522 = DIRECTION ( 'NONE',  ( 1.000000000000000000, -0.000000000000000000, -0.000000000000000000 ) ) ;
#10523 = ORIENTED_EDGE ( 'NONE', *, *, #20230, .F. ) ;
#10524 = CARTESIAN_POINT ( 'NONE',  ( -145.0195698084541505, -175.3837268820161057, 79.40367028273126948 ) ) ;
#10525 = EDGE_CURVE ( 'NONE', #37576, #45084, #9045, .T. ) ;
#10526 = CARTESIAN_POINT ( 'NONE',  ( 43.12693905415815010, -175.3837268820161057, -83.57229767764155781 ) ) ;
#10527 = VECTOR ( 'NONE', #41140, 1000.000000000000000 ) ;
#10528 = EDGE_CURVE ( 'NONE', #50173, #10187, #7133, .T. ) ;
#10529 = AXIS2_PLACEMENT_3D ( 'NONE', #27408, #43456, #35545 ) ;
#10530 = DIRECTION ( 'NONE',  ( 0.000000000000000000, -1.000000000000000000, 0.000000000000000000 ) ) ;
#10531 = CARTESIAN_POINT ( 'NONE',  ( -109.0835867659424565, -193.5000000000000000, -109.3256576763154726 ) ) ;
#10532 = ORIENTED_EDGE ( 'NONE', *, *, #46549, .T. ) ;
#10533 = EDGE_CURVE ( 'NONE', #34277, #15815, #1461, .T. ) ;
#10534 = AXIS2_PLACEMENT_3D ( 'NONE', #10761, #23610, #15761 ) ;
#10535 = EDGE_CURVE ( 'NONE', #14596, #45545, #34471, .T. ) ;
#10536 = AXIS2_PLACEMENT_3D ( 'NONE', #13352, #38732, #14586 ) ;
#10537 = EDGE_CURVE ( 'NONE', #32593, #8246, #3144, .T. ) ;
#10538 = LINE ( 'NONE', #22888, #43795 ) ;
#10539 = DIRECTION ( 'NONE',  ( 1.000000000000000000, -5.399917434947259359E-17, 0.000000000000000000 ) ) ;
#10540 = PLANE ( 'NONE',  #12776 ) ;
#10541 = EDGE_CURVE ( 'NONE', #29842, #41150, #50993, .T. ) ;
#10542 = ORIENTED_EDGE ( 'NONE', *, *, #14677, .T. ) ;
#10543 = DIRECTION ( 'NONE',  ( 0.9995608365087942371, 0.000000000000000000, 0.02963332782256331357 ) ) ;
#10544 = CARTESIAN_POINT ( 'NONE',  ( -170.2837019307126809, -177.1207230881787780, 23.23456943914128203 ) ) ;
#10545 = ORIENTED_EDGE ( 'NONE', *, *, #27435, .F. ) ;
#10546 = ORIENTED_EDGE ( 'NONE', *, *, #14754, .F. ) ;
#10547 = CIRCLE ( 'NONE', #39084, 125.0000000000000000 ) ;
#10548 = ORIENTED_EDGE ( 'NONE', *, *, #46483, .T. ) ;
#10549 = CARTESIAN_POINT ( 'NONE',  ( -305.0000000000000568, -63.87926739338328730, 6.735595255826143379 ) ) ;
#10550 = AXIS2_PLACEMENT_3D ( 'NONE', #41333, #5353, #37394 ) ;
#10551 = CIRCLE ( 'NONE', #2974, 125.0000000000000000 ) ;
#10552 = DIRECTION ( 'NONE',  ( -0.000000000000000000, 1.000000000000000000, -0.000000000000000000 ) ) ;
#10553 = CARTESIAN_POINT ( 'NONE',  ( -11.17913199888832843, -193.5000000000000000, 119.3051146910914326 ) ) ;
#10554 = EDGE_LOOP ( 'NONE', ( #18312, #34987, #41382, #27060 ) ) ;
#10555 = EDGE_CURVE ( 'NONE', #23501, #14662, #10823, .T. ) ;
#10556 = DIRECTION ( 'NONE',  ( 0.000000000000000000, 0.000000000000000000, -1.000000000000000000 ) ) ;
#10557 = APPLICATION_CONTEXT ( 'automotive_design' ) ;
#10558 = CARTESIAN_POINT ( 'NONE',  ( -117.6201219941651601, -193.5000000000000000, 104.1370384486469902 ) ) ;
#10561 = VERTEX_POINT ( 'NONE', #22909 ) ;
#10560 = CARTESIAN_POINT ( 'NONE',  ( -170.0000000000000284, -173.5000000000000284, 60.00000000000000000 ) ) ;
#10559 = DIRECTION ( 'NONE',  ( 0.000000000000000000, -1.000000000000000000, -0.000000000000000000 ) ) ;
#10562 = CIRCLE ( 'NONE', #50041, 125.0000000000000000 ) ;
#10563 = DIRECTION ( 'NONE',  ( 0.000000000000000000, -1.000000000000000000, 0.000000000000000000 ) ) ;
#10564 = ORIENTED_EDGE ( 'NONE', *, *, #13614, .F. ) ;
#10565 = DIRECTION ( 'NONE',  ( -0.000000000000000000, -1.000000000000000000, -0.000000000000000000 ) ) ;
#10566 = VERTEX_POINT ( 'NONE', #11317 ) ;
#10567 = PLANE ( 'NONE',  #19053 ) ;
#10568 = VECTOR ( 'NONE', #44979, 1000.000000000000000 ) ;
#10569 = PLANE ( 'NONE',  #38065 ) ;
#10570 = CARTESIAN_POINT ( 'NONE',  ( -330.4913330509368166, -84.00150778970706256, 43.83057281297416097 ) ) ;
#10571 = EDGE_CURVE ( 'NONE', #7135, #41798, #2928, .T. ) ;
#10572 = ORIENTED_EDGE ( 'NONE', *, *, #39814, .F. ) ;
#10573 = LINE ( 'NONE', #2685, #28122 ) ;
#10574 = CARTESIAN_POINT ( 'NONE',  ( -65.65563056894596627, -183.6283474603465606, 123.8142468240612999 ) ) ;
#10575 = ORIENTED_EDGE ( 'NONE', *, *, #45851, .F. ) ;
#10576 = DIRECTION ( 'NONE',  ( 5.399917434947259359E-17, 1.000000000000000000, -0.000000000000000000 ) ) ;
#10577 = LINE ( 'NONE', #22674, #13108 ) ;
#10578 = EDGE_CURVE ( 'NONE', #50151, #10964, #42098, .T. ) ;
#10579 = EDGE_CURVE ( 'NONE', #34048, #6061, #47088, .T. ) ;
#10580 = ORIENTED_EDGE ( 'NONE', *, *, #7338, .T. ) ;
#10581 = EDGE_CURVE ( 'NONE', #23257, #22776, #35035, .T. ) ;
#10582 = DIRECTION ( 'NONE',  ( 0.5586467658036535777, 0.000000000000000000, -0.8294056854502011022 ) ) ;
#10583 = LINE ( 'NONE', #42647, #29827 ) ;
#10584 = EDGE_CURVE ( 'NONE', #4360, #23329, #44436, .T. ) ;
#10585 = ORIENTED_EDGE ( 'NONE', *, *, #32867, .F. ) ;
#10586 = LINE ( 'NONE', #9555, #28268 ) ;
#10587 = VERTEX_POINT ( 'NONE', #32600 ) ;
#10588 = VECTOR ( 'NONE', #43040, 1000.000000000000000 ) ;
#10589 = CIRCLE ( 'NONE', #14806, 125.0000000000000000 ) ;
#10590 = CARTESIAN_POINT ( 'NONE',  ( -142.9772358822569629, -193.5000000000000000, 81.82363577055969017 ) ) ;
#10591 = CARTESIAN_POINT ( 'NONE',  ( 64.01121016852529522, -193.5000000000000000, -54.50618404930953176 ) ) ;
#10592 = EDGE_LOOP ( 'NONE', ( #2300, #20158, #25562, #50717 ) ) ;
#10593 = VECTOR ( 'NONE', #21843, 1000.000000000000000 ) ;
#10594 = VECTOR ( 'NONE', #295, 1000.000000000000114 ) ;
#10595 = DIRECTION ( 'NONE',  ( 0.000000000000000000, 0.7071067811865444641, 0.7071067811865505703 ) ) ;
#10596 = CARTESIAN_POINT ( 'NONE',  ( -142.3192003680973130, -193.5000000000000000, 82.57748230379306165 ) ) ;
#10597 = CARTESIAN_POINT ( 'NONE',  ( -46.12632737020501850, -183.6283474603465606, -123.9784823535113532 ) ) ;
#10598 = VERTEX_POINT ( 'NONE', #11838 ) ;
#10599 = CARTESIAN_POINT ( 'NONE',  ( -48.36085358058748085, -189.7472609257535510, -0.9929810960135100339 ) ) ;
#10600 = ADVANCED_FACE ( 'NONE', ( #35493 ), #48374, .T. ) ;
#10601 = CIRCLE ( 'NONE', #25727, 125.0000000000000000 ) ;
#10602 = DIRECTION ( 'NONE',  ( -0.000000000000000000, 0.9927088740980556381, 0.1205366802553095307 ) ) ;
#10603 = CARTESIAN_POINT ( 'NONE',  ( 75.02564229359539638, -189.7472609257535510, -19.27620354518634826 ) ) ;
#10605 = ORIENTED_EDGE ( 'NONE', *, *, #47659, .F. ) ;
#10604 = CARTESIAN_POINT ( 'NONE',  ( -330.4913330509368166, -123.0000000000002700, -59.99791663049643375 ) ) ;
#10606 = CIRCLE ( 'NONE', #51771, 125.0000000000000000 ) ;
#10607 = AXIS2_PLACEMENT_3D ( 'NONE', #26214, #21777, #46219 ) ;
#10608 = ADVANCED_FACE ( 'NONE', ( #51542 ), #12361, .T. ) ;
#10609 = ORIENTED_EDGE ( 'NONE', *, *, #11709, .F. ) ;
#10610 = DIRECTION ( 'NONE',  ( -0.8124868780056863082, 0.000000000000000000, 0.5829794791144649047 ) ) ;
#10611 = VECTOR ( 'NONE', #15497, 1000.000000000000000 ) ;
#10612 = ADVANCED_FACE ( 'NONE', ( #3698 ), #51814, .T. ) ;
#10613 = VECTOR ( 'NONE', #8489, 1000.000000000000000 ) ;
#10614 = CARTESIAN_POINT ( 'NONE',  ( -48.47912675150885065, -175.3837268820161057, 6.938893903907228378E-15 ) ) ;
#10615 = ORIENTED_EDGE ( 'NONE', *, *, #47967, .T. ) ;
#10616 = CARTESIAN_POINT ( 'NONE',  ( 8.750818922897904528, -193.5000000000000000, -111.1293539894138434 ) ) ;
#10617 = ORIENTED_EDGE ( 'NONE', *, *, #15887, .T. ) ;
#10618 = DIRECTION ( 'NONE',  ( 1.000000000000000000, -0.000000000000000000, -0.000000000000000000 ) ) ;
#10619 = LINE ( 'NONE', #26650, #49361 ) ;
#10620 = CARTESIAN_POINT ( 'NONE',  ( -159.5526844214375899, -183.6283474603465606, 57.33816169485221081 ) ) ;
#10621 = DIRECTION ( 'NONE',  ( 0.000000000000000000, 1.000000000000000000, -0.000000000000000000 ) ) ;
#10622 = ORIENTED_EDGE ( 'NONE', *, *, #6330, .T. ) ;
#10623 = ORIENTED_EDGE ( 'NONE', *, *, #40134, .T. ) ;
#10624 = ORIENTED_EDGE ( 'NONE', *, *, #12854, .F. ) ;
#10625 = ADVANCED_FACE ( 'NONE', ( #11594 ), #27865, .T. ) ;
#10626 = CARTESIAN_POINT ( 'NONE',  ( -166.1003692892502102, -193.5000000000000000, -42.31126686685032467 ) ) ;
#10627 = CARTESIAN_POINT ( 'NONE',  ( -305.0000000000000568, -69.20050475944881896, 25.52576769896171882 ) ) ;
#10628 = VECTOR ( 'NONE', #46809, 1000.000000000000000 ) ;
#10629 = VECTOR ( 'NONE', #39719, 1000.000000000000000 ) ;
#10630 = LINE ( 'NONE', #19540, #2700 ) ;
#10631 = DIRECTION ( 'NONE',  ( 0.000000000000000000, 0.000000000000000000, 1.000000000000000000 ) ) ;
#10632 = ORIENTED_EDGE ( 'NONE', *, *, #23110, .T. ) ;
#10633 = CIRCLE ( 'NONE', #44203, 125.0000000000000000 ) ;
#10634 = CARTESIAN_POINT ( 'NONE',  ( -180.0000000000000568, -123.5000000000000284, 37.63467731922665394 ) ) ;
#10635 = DIRECTION ( 'NONE',  ( 0.7765238627180437447, 0.000000000000000000, -0.6300878435817094392 ) ) ;
#10636 = VERTEX_POINT ( 'NONE', #48116 ) ;
#10637 = ORIENTED_EDGE ( 'NONE', *, *, #32859, .F. ) ;
#10638 = VECTOR ( 'NONE', #47984, 1000.000000000000114 ) ;
#10639 = PLANE ( 'NONE',  #25648 ) ;
#10640 = CARTESIAN_POINT ( 'NONE',  ( -336.3521761649654422, -123.5000000000000284, 0.000000000000000000 ) ) ;
#10641 = AXIS2_PLACEMENT_3D ( 'NONE', #50734, #38887, #11277 ) ;
#10642 = DIRECTION ( 'NONE',  ( -0.000000000000000000, 1.000000000000000000, -0.000000000000000000 ) ) ;
#10643 = VECTOR ( 'NONE', #34233, 999.9999999999998863 ) ;
#10644 = AXIS2_PLACEMENT_3D ( 'NONE', #43995, #34621, #50665 ) ;
#10645 = DIRECTION ( 'NONE',  ( -0.000000000000000000, 1.000000000000000000, -0.000000000000000000 ) ) ;
#10646 = EDGE_CURVE ( 'NONE', #49014, #18461, #32075, .T. ) ;
#10648 = EDGE_CURVE ( 'NONE', #51184, #7509, #4850, .T. ) ;
#10647 = DIRECTION ( 'NONE',  ( 0.000000000000000000, 0.5000000000000012212, -0.8660254037844378194 ) ) ;
#10649 = VERTEX_POINT ( 'NONE', #16590 ) ;
#10650 = DIRECTION ( 'NONE',  ( 0.000000000000000000, 0.000000000000000000, -1.000000000000000000 ) ) ;
#10651 = VECTOR ( 'NONE', #13792, 1000.000000000000000 ) ;
#10652 = AXIS2_PLACEMENT_3D ( 'NONE', #40480, #28130, #27634 ) ;
#10653 = ORIENTED_EDGE ( 'NONE', *, *, #1191, .F. ) ;
#10654 = PLANE ( 'NONE',  #9479 ) ;
#10655 = LINE ( 'NONE', #18793, #17777 ) ;
#10656 = ORIENTED_EDGE ( 'NONE', *, *, #32716, .F. ) ;
#10657 = CARTESIAN_POINT ( 'NONE',  ( -148.7414553014637306, -193.5000000000000000, 72.96212019587208886 ) ) ;
#10658 = DIRECTION ( 'NONE',  ( 0.000000000000000000, 0.5680647467311457088, -0.8229838658936634577 ) ) ;
#10659 = DIRECTION ( 'NONE',  ( 0.000000000000000000, 1.000000000000000000, 0.000000000000000000 ) ) ;
#10660 = DIRECTION ( 'NONE',  ( -0.000000000000000000, 0.9927088740980538617, -0.1205366802553232974 ) ) ;
#10661 = DIRECTION ( 'NONE',  ( 0.4031234292879730674, 0.000000000000000000, -0.9151456172430181280 ) ) ;
#10662 = VERTEX_POINT ( 'NONE', #24450 ) ;
#10663 = AXIS2_PLACEMENT_3D ( 'NONE', #35130, #39572, #38560 ) ;
#10664 = AXIS2_PLACEMENT_3D ( 'NONE', #46046, #21860, #33433 ) ;
#10665 = EDGE_CURVE ( 'NONE', #49241, #19447, #15813, .T. ) ;
#10666 = DIRECTION ( 'NONE',  ( -0.000000000000000000, 1.000000000000000000, -0.000000000000000000 ) ) ;
#10667 = VERTEX_POINT ( 'NONE', #4229 ) ;
#10668 = VECTOR ( 'NONE', #41300, 1000.000000000000000 ) ;
#10669 = EDGE_LOOP ( 'NONE', ( #41049, #27759, #43126, #35745 ) ) ;
#10670 = DIRECTION ( 'NONE',  ( 0.6528221181905119463, 0.000000000000000000, 0.7575112421616284619 ) ) ;
#10671 = VERTEX_POINT ( 'NONE', #8423 ) ;
#10672 = EDGE_CURVE ( 'NONE', #4273, #4514, #39944, .T. ) ;
#10673 = CARTESIAN_POINT ( 'NONE',  ( -70.24606818074175862, -193.5000000000000000, -122.0745693923548885 ) ) ;
#10674 = AXIS2_PLACEMENT_3D ( 'NONE', #27418, #79, #43467 ) ;
#10675 = EDGE_LOOP ( 'NONE', ( #11925, #34064, #49511, #44492 ) ) ;
#10676 = DIRECTION ( 'NONE',  ( 0.000000000000000000, 0.000000000000000000, 1.000000000000000000 ) ) ;
#10677 = AXIS2_PLACEMENT_3D ( 'NONE', #16063, #40730, #4750 ) ;
#10678 = DIRECTION ( 'NONE',  ( 0.000000000000000000, 0.000000000000000000, 1.000000000000000000 ) ) ;
#10679 = ORIENTED_EDGE ( 'NONE', *, *, #50433, .T. ) ;
#10680 = DIRECTION ( 'NONE',  ( 0.000000000000000000, 1.000000000000000000, 0.000000000000000000 ) ) ;
#10681 = VECTOR ( 'NONE', #21087, 1000.000000000000000 ) ;
#10682 = FACE_OUTER_BOUND ( 'NONE', #38413, .T. ) ;
#10683 = CARTESIAN_POINT ( 'NONE',  ( 28.02885774092381865, -189.7472609257535510, 98.85104101073331151 ) ) ;
#10684 = VERTEX_POINT ( 'NONE', #8170 ) ;
#10685 = EDGE_LOOP ( 'NONE', ( #32329, #50048, #50366, #30804 ) ) ;
#10686 = EDGE_LOOP ( 'NONE', ( #47887, #14202, #1728, #624 ) ) ;
#10687 = CIRCLE ( 'NONE', #16587, 15.00000000000000000 ) ;
#10688 = CARTESIAN_POINT ( 'NONE',  ( -129.9529520667707914, -175.3837268820161057, -94.79987230211959570 ) ) ;
#10689 = DIRECTION ( 'NONE',  ( 0.000000000000000000, 1.000000000000000000, -0.000000000000000000 ) ) ;
#10690 = FACE_OUTER_BOUND ( 'NONE', #41167, .T. ) ;
#10691 = CARTESIAN_POINT ( 'NONE',  ( 11.52087324849114580, -173.5000000000000284, -60.00000000000002842 ) ) ;
#10692 = CARTESIAN_POINT ( 'NONE',  ( -330.4913330509368166, -79.66942718702547666, -39.49849221029252533 ) ) ;
#10693 = ORIENTED_EDGE ( 'NONE', *, *, #10706, .T. ) ;
#10694 = ADVANCED_FACE ( 'NONE', ( #4490 ), #28385, .T. ) ;
#10695 = PLANE ( 'NONE',  #12269 ) ;
#10696 = ORIENTED_EDGE ( 'NONE', *, *, #40919, .F. ) ;
#10698 = VERTEX_POINT ( 'NONE', #20506 ) ;
#10697 = CARTESIAN_POINT ( 'NONE',  ( -330.4913330509368166, -145.2430625708868206, 55.92172413327848801 ) ) ;
#10699 = VECTOR ( 'NONE', #51437, 1000.000000000000000 ) ;
#10700 = ORIENTED_EDGE ( 'NONE', *, *, #48169, .T. ) ;
#10701 = VECTOR ( 'NONE', #37010, 1000.000000000000000 ) ;
#10702 = CARTESIAN_POINT ( 'NONE',  ( -173.2765435274470178, -193.5000000000000000, -7.113702696401505321 ) ) ;
#10703 = CARTESIAN_POINT ( 'NONE',  ( 66.11593792271145276, -193.5000000000000000, -47.37063079638321739 ) ) ;
#10704 = AXIS2_PLACEMENT_3D ( 'NONE', #25995, #26240, #42018 ) ;
#10705 = CARTESIAN_POINT ( 'NONE',  ( -336.3521761649654422, -91.32752733096738496, -49.48329383994654052 ) ) ;
#10706 = EDGE_CURVE ( 'NONE', #4089, #15087, #2337, .T. ) ;
#10707 = FACE_OUTER_BOUND ( 'NONE', #34604, .T. ) ;
#10708 = ORIENTED_EDGE ( 'NONE', *, *, #33374, .T. ) ;
#10709 = DIRECTION ( 'NONE',  ( -0.5085311186492094127, 0.000000000000000000, -0.8610436117673619938 ) ) ;
#10710 = EDGE_LOOP ( 'NONE', ( #15511, #38258, #9539, #44044 ) ) ;
#10711 = EDGE_LOOP ( 'NONE', ( #29105, #26734, #19944, #31314 ) ) ;
#10712 = LINE ( 'NONE', #26737, #20339 ) ;
#10713 = VECTOR ( 'NONE', #47728, 1000.000000000000227 ) ;
#10714 = EDGE_CURVE ( 'NONE', #43197, #36214, #7647, .T. ) ;
#10715 = CARTESIAN_POINT ( 'NONE',  ( -339.1964088526558498, -175.5095439275173135, 27.86139516340941213 ) ) ;
#10716 = CIRCLE ( 'NONE', #13236, 125.0000000000000000 ) ;
#10717 = CARTESIAN_POINT ( 'NONE',  ( 65.52619748798558419, -177.1207230881787780, 48.77484799213969069 ) ) ;
#10718 = ORIENTED_EDGE ( 'NONE', *, *, #971, .T. ) ;
#10719 = AXIS2_PLACEMENT_3D ( 'NONE', #16202, #11731, #51187 ) ;
#10720 = LINE ( 'NONE', #39075, #42465 ) ;
#10721 = CARTESIAN_POINT ( 'NONE',  ( -339.1964088526558498, -143.9541802141672235, -55.34326076196065003 ) ) ;
#10722 = CARTESIAN_POINT ( 'NONE',  ( -85.14888725715768203, -175.3837268820161057, 119.5003291395398577 ) ) ;
#10723 = CARTESIAN_POINT ( 'NONE',  ( -332.3517673607765914, -64.66963335249506883, 11.78931550685348206 ) ) ;
#10724 = VECTOR ( 'NONE', #42579, 1000.000000000000000 ) ;
#10725 = ORIENTED_EDGE ( 'NONE', *, *, #18542, .F. ) ;
#10726 = LINE ( 'NONE', #38829, #12035 ) ;
#10727 = DIRECTION ( 'NONE',  ( 0.000000000000000000, 0.000000000000000000, 1.000000000000000000 ) ) ;
#10728 = VECTOR ( 'NONE', #46262, 1000.000000000000227 ) ;
#10729 = DIRECTION ( 'NONE',  ( 1.000000000000000000, 3.091579882402590330E-17, -8.151826190875920009E-17 ) ) ;
#10730 = ORIENTED_EDGE ( 'NONE', *, *, #1582, .T. ) ;
#10731 = ADVANCED_FACE ( 'NONE', ( #27354 ), #39683, .F. ) ;
#10732 = CARTESIAN_POINT ( 'NONE',  ( -172.0042974347349229, -189.7472609257535510, 10.84123789944660743 ) ) ;
#10733 = CARTESIAN_POINT ( 'NONE',  ( -168.0489871616337325, -189.7472609257535510, -32.84887689123905830 ) ) ;
#10734 = VERTEX_POINT ( 'NONE', #24 ) ;
#10735 = CARTESIAN_POINT ( 'NONE',  ( -336.3521761649654422, -161.4024510877913485, 45.24454186338643780 ) ) ;
#10736 = ORIENTED_EDGE ( 'NONE', *, *, #30442, .T. ) ;
#10737 = AXIS2_PLACEMENT_3D ( 'NONE', #19806, #35841, #15890 ) ;
#10738 = CARTESIAN_POINT ( 'NONE',  ( -49.30901192927175458, -189.7472609257535510, -124.9972451320097093 ) ) ;
#10739 = CIRCLE ( 'NONE', #39284, 125.0000000000000000 ) ;
#10740 = LINE ( 'NONE', #46752, #44673 ) ;
#10741 = LINE ( 'NONE', #39096, #12809 ) ;
#10742 = VECTOR ( 'NONE', #593, 1000.000000000000114 ) ;
#10743 = CARTESIAN_POINT ( 'NONE',  ( -139.8555433305420195, -193.5000000000000000, -83.82333043185242616 ) ) ;
#10744 = LINE ( 'NONE', #11509, #18505 ) ;
#10745 = EDGE_LOOP ( 'NONE', ( #19087, #30005, #11251, #4545 ) ) ;
#10746 = DIRECTION ( 'NONE',  ( -0.000000000000000000, 1.000000000000000000, -0.000000000000000000 ) ) ;
#10747 = VERTEX_POINT ( 'NONE', #43405 ) ;
#10748 = CARTESIAN_POINT ( 'NONE',  ( -60.00000000000000000, 20.00000000000000000, 60.00000000000000711 ) ) ;
#10749 = AXIS2_PLACEMENT_3D ( 'NONE', #22058, #38077, #18123 ) ;
#10750 = ORIENTED_EDGE ( 'NONE', *, *, #42437, .F. ) ;
#10751 = DIRECTION ( 'NONE',  ( -0.000000000000000000, 1.000000000000000000, -0.000000000000000000 ) ) ;
#10752 = EDGE_CURVE ( 'NONE', #26038, #32799, #39438, .T. ) ;
#10753 = VECTOR ( 'NONE', #16320, 999.9999999999998863 ) ;
#10754 = EDGE_CURVE ( 'NONE', #41126, #35288, #8685, .T. ) ;
#10755 = DIRECTION ( 'NONE',  ( 0.000000000000000000, 1.000000000000000000, 0.000000000000000000 ) ) ;
#10756 = DIRECTION ( 'NONE',  ( 0.000000000000000000, -1.000000000000000000, 0.000000000000000000 ) ) ;
#10757 = ORIENTED_EDGE ( 'NONE', *, *, #6450, .T. ) ;
#10760 = ORIENTED_EDGE ( 'NONE', *, *, #30207, .T. ) ;
#10759 = CARTESIAN_POINT ( 'NONE',  ( -48.47912675150885065, -189.7472609257535510, 6.938893903907228378E-15 ) ) ;
#10758 = CARTESIAN_POINT ( 'NONE',  ( -145.6517069852672535, -175.3837268820161057, 78.62880929222943394 ) ) ;
#10761 = CARTESIAN_POINT ( 'NONE',  ( -170.6250538923603131, -193.5000000000000000, 26.55884942729649723 ) ) ;
#10762 = ORIENTED_EDGE ( 'NONE', *, *, #38603, .T. ) ;
#10763 = CARTESIAN_POINT ( 'NONE',  ( 42.10477485469927927, -183.6283474603465606, 86.13684908212515268 ) ) ;
#10764 = ORIENTED_EDGE ( 'NONE', *, *, #23748, .F. ) ;
#10765 = ADVANCED_FACE ( 'NONE', ( #48904 ), #49162, .F. ) ;
#10766 = DIRECTION ( 'NONE',  ( 0.000000000000000000, 0.000000000000000000, 1.000000000000000000 ) ) ;
#10769 = VERTEX_POINT ( 'NONE', #12881 ) ;
#10768 = DIRECTION ( 'NONE',  ( -0.000000000000000000, 1.000000000000000000, -0.000000000000000000 ) ) ;
#10767 = DIRECTION ( 'NONE',  ( 0.000000000000000000, -1.000000000000000000, 0.000000000000000000 ) ) ;
#10770 = ORIENTED_EDGE ( 'NONE', *, *, #17882, .F. ) ;
#10771 = ADVANCED_FACE ( 'NONE', ( #20778 ), #45734, .T. ) ;
#10772 = EDGE_CURVE ( 'NONE', #39548, #22041, #41253, .T. ) ;
#10773 = DIRECTION ( 'NONE',  ( -0.000000000000000000, 1.000000000000000000, -0.000000000000000000 ) ) ;
#10774 = VERTEX_POINT ( 'NONE', #41512 ) ;
#10775 = FACE_OUTER_BOUND ( 'NONE', #40569, .T. ) ;
#10776 = CIRCLE ( 'NONE', #49397, 15.24495751795539000 ) ;
#10777 = EDGE_CURVE ( 'NONE', #30392, #42165, #26671, .T. ) ;
#10778 = FACE_OUTER_BOUND ( 'NONE', #35710, .T. ) ;
#10779 = VERTEX_POINT ( 'NONE', #25494 ) ;
#10780 = AXIS2_PLACEMENT_3D ( 'NONE', #37315, #12879, #17871 ) ;
#10781 = DIRECTION ( 'NONE',  ( -0.000000000000000000, 1.000000000000000000, -0.000000000000000000 ) ) ;
#10782 = DIRECTION ( 'NONE',  ( 0.9842305779475954974, 0.000000000000000000, 0.1768902751225803205 ) ) ;
#10783 = CARTESIAN_POINT ( 'NONE',  ( -339.1964088526558498, -181.8741440471346493, 13.87297036558423002 ) ) ;
#10784 = CARTESIAN_POINT ( 'NONE',  ( -48.47912675150885065, -183.6283474603465606, 6.938893903907228378E-15 ) ) ;
#10785 = VECTOR ( 'NONE', #31032, 999.9999999999998863 ) ;
#10786 = DIRECTION ( 'NONE',  ( -0.000000000000000000, 1.000000000000000000, 0.000000000000000000 ) ) ;
#10787 = EDGE_LOOP ( 'NONE', ( #30153, #13187, #43641, #23638 ) ) ;
#10788 = CARTESIAN_POINT ( 'NONE',  ( -336.3521761649654422, -65.58448481710581746, 11.56382487286456140 ) ) ;
#10789 = CARTESIAN_POINT ( 'NONE',  ( -336.3521761649654422, -136.0347666902908372, 57.67619951860663718 ) ) ;
#10790 = PLANE ( 'NONE',  #1950 ) ;
#10791 = VERTEX_POINT ( 'NONE', #13669 ) ;
#10792 = CIRCLE ( 'NONE', #51106, 60.00000000000000000 ) ;
#10793 = FACE_OUTER_BOUND ( 'NONE', #22905, .T. ) ;
#10794 = DIRECTION ( 'NONE',  ( -1.000000000000000000, 5.928974370888818045E-15, -8.589602288500893078E-15 ) ) ;
#10795 = PLANE ( 'NONE',  #3081 ) ;
#10796 = DIRECTION ( 'NONE',  ( -0.000000000000000000, 1.000000000000000000, -0.000000000000000000 ) ) ;
#10797 = CARTESIAN_POINT ( 'NONE',  ( 46.00000000000000711, -43.50000000000000000, -41.99999999999999289 ) ) ;
#10798 = CIRCLE ( 'NONE', #9120, 124.9999999999999858 ) ;
#10799 = DIRECTION ( 'NONE',  ( 0.000000000000000000, 0.000000000000000000, 1.000000000000000000 ) ) ;
#10800 = DIRECTION ( 'NONE',  ( 0.000000000000000000, 0.9350162426854194964, 0.3546048870425235200 ) ) ;
#10801 = FACE_OUTER_BOUND ( 'NONE', #22002, .T. ) ;
#10802 = CARTESIAN_POINT ( 'NONE',  ( 7.991501969728830090, -193.5000000000000000, 110.3950557015152754 ) ) ;
#10803 = ORIENTED_EDGE ( 'NONE', *, *, #48437, .T. ) ;
#10804 = DIRECTION ( 'NONE',  ( -0.000000000000000000, 0.7485107481710999711, -0.6631226582407964143 ) ) ;
#10805 = CARTESIAN_POINT ( 'NONE',  ( -330.4913330509368166, -71.49045607248213230, 27.86139516340826461 ) ) ;
#10806 = ORIENTED_EDGE ( 'NONE', *, *, #26030, .F. ) ;
#10807 = VECTOR ( 'NONE', #17036, 1000.000000000000227 ) ;
#10808 = VECTOR ( 'NONE', #8195, 1000.000000000000000 ) ;
#10809 = ORIENTED_EDGE ( 'NONE', *, *, #27902, .T. ) ;
#10810 = AXIS2_PLACEMENT_3D ( 'NONE', #24645, #29363, #37256 ) ;
#10811 = ORIENTED_EDGE ( 'NONE', *, *, #7054, .T. ) ;
#10812 = CARTESIAN_POINT ( 'NONE',  ( -172.4792251663439231, -183.6283474603465606, 0.3215015308248941328 ) ) ;
#10813 = VECTOR ( 'NONE', #8872, 1000.000000000000000 ) ;
#10814 = ADVANCED_FACE ( 'NONE', ( #5539 ), #29177, .T. ) ;
#10815 = EDGE_CURVE ( 'NONE', #5724, #7178, #45230, .T. ) ;
#10816 = EDGE_CURVE ( 'NONE', #3747, #1163, #804, .T. ) ;
#10817 = LINE ( 'NONE', #30519, #51331 ) ;
#10818 = CARTESIAN_POINT ( 'NONE',  ( -48.47912675150885065, -177.1207230881787780, 6.938893903907228378E-15 ) ) ;
#10819 = EDGE_LOOP ( 'NONE', ( #36049, #22204 ) ) ;
#10820 = PLANE ( 'NONE',  #11708 ) ;
#10821 = DIRECTION ( 'NONE',  ( 0.000000000000000000, -0.000000000000000000, 1.000000000000000000 ) ) ;
#10822 = CIRCLE ( 'NONE', #4119, 60.00000000000000000 ) ;
#10825 = ORIENTED_EDGE ( 'NONE', *, *, #7398, .F. ) ;
#10824 = LINE ( 'NONE', #3201, #49294 ) ;
#10823 = LINE ( 'NONE', #51290, #23305 ) ;
#10826 = EDGE_CURVE ( 'NONE', #24446, #27872, #5811, .T. ) ;
#10827 = LINE ( 'NONE', #49742, #28940 ) ;
#10828 = VERTEX_POINT ( 'NONE', #1833 ) ;
#10829 = CARTESIAN_POINT ( 'NONE',  ( -93.85419746441394295, -183.6283474603465606, 115.4006183233324805 ) ) ;
#10830 = ORIENTED_EDGE ( 'NONE', *, *, #1326, .F. ) ;
#10831 = CARTESIAN_POINT ( 'NONE',  ( -305.0000000000000568, -179.0013928959018301, 22.79463504017430253 ) ) ;
#10832 = EDGE_CURVE ( 'NONE', #6145, #23787, #1316, .T. ) ;
#10833 = DIRECTION ( 'NONE',  ( -0.9890401873221623674, 0.000000000000000000, -0.1476465640024917925 ) ) ;
#10834 = CARTESIAN_POINT ( 'NONE',  ( -170.0000000000000284, -115.7896721143442278, -60.00000000000000711 ) ) ;
#10835 = ORIENTED_EDGE ( 'NONE', *, *, #10136, .F. ) ;
#10836 = ADVANCED_FACE ( 'NONE', ( #17376 ), #33397, .T. ) ;
#10837 = AXIS2_PLACEMENT_3D ( 'NONE', #33267, #34302, #2251 ) ;
#10838 = VERTEX_POINT ( 'NONE', #1590 ) ;
#10839 = CARTESIAN_POINT ( 'NONE',  ( -26.53529504715431031, -193.5000000000000000, 123.0587999703026725 ) ) ;
#10840 = EDGE_CURVE ( 'NONE', #18322, #40221, #44311, .T. ) ;
#10841 = DIRECTION ( 'NONE',  ( -0.000000000000000000, -1.000000000000000000, -0.000000000000000000 ) ) ;
#10842 = EDGE_LOOP ( 'NONE', ( #14085, #39103, #43697, #21541 ) ) ;
#10843 = DIRECTION ( 'NONE',  ( -0.5085311186492094127, 0.000000000000000000, -0.8610436117673619938 ) ) ;
#10844 = PLANE ( 'NONE',  #50033 ) ;
#10845 = EDGE_CURVE ( 'NONE', #43984, #41178, #21824, .T. ) ;
#10846 = ORIENTED_EDGE ( 'NONE', *, *, #26231, .F. ) ;
#10847 = FACE_OUTER_BOUND ( 'NONE', #4061, .T. ) ;
#10848 = CARTESIAN_POINT ( 'NONE',  ( -159.5526844214375615, -193.5000000000000000, 57.33816169485226055 ) ) ;
#10849 = ORIENTED_EDGE ( 'NONE', *, *, #45256, .T. ) ;
#10850 = FACE_OUTER_BOUND ( 'NONE', #3445, .T. ) ;
#10851 = VERTEX_POINT ( 'NONE', #29689 ) ;
#10852 = CIRCLE ( 'NONE', #8342, 4.999999999999997335 ) ;
#10853 = CARTESIAN_POINT ( 'NONE',  ( -47.53180039765466347, -193.5000000000000000, 0.3202698538628485636 ) ) ;
#10854 = PLANE ( 'NONE',  #21141 ) ;
#10855 = ORIENTED_EDGE ( 'NONE', *, *, #40831, .F. ) ;
#10856 = AXIS2_PLACEMENT_3D ( 'NONE', #26446, #42754, #1765 ) ;
#10857 = DIRECTION ( 'NONE',  ( 0.000000000000000000, 0.4647231720437664526, -0.8854560256532110207 ) ) ;
#10858 = DIRECTION ( 'NONE',  ( -1.000000000000000000, 0.000000000000000000, 0.000000000000000000 ) ) ;
#10859 = FACE_OUTER_BOUND ( 'NONE', #23330, .T. ) ;
#10860 = ORIENTED_EDGE ( 'NONE', *, *, #4659, .T. ) ;
#10861 = CARTESIAN_POINT ( 'NONE',  ( 0.000000000000000000, -137.6196241929661710, -57.28556722813703317 ) ) ;
#10862 = CARTESIAN_POINT ( 'NONE',  ( -330.4913330509368166, -123.5000000000000284, 0.000000000000000000 ) ) ;
#10863 = CARTESIAN_POINT ( 'NONE',  ( -33.86391487983341619, -175.3837268820161057, 124.1426420773540542 ) ) ;
#10865 = VERTEX_POINT ( 'NONE', #1052 ) ;
#10864 = DIRECTION ( 'NONE',  ( 0.000000000000000000, 0.000000000000000000, 1.000000000000000000 ) ) ;
#10866 = EDGE_LOOP ( 'NONE', ( #3272, #3394, #10981, #21368 ) ) ;
#10867 = DIRECTION ( 'NONE',  ( 0.000000000000000000, -0.7485107481710953081, 0.6631226582408016323 ) ) ;
#10868 = EDGE_CURVE ( 'NONE', #41267, #34577, #51850, .T. ) ;
#10869 = CARTESIAN_POINT ( 'NONE',  ( -305.0000000000000568, -182.8437365148560616, 8.849911663702917153 ) ) ;
#10870 =( REPRESENTATION_RELATIONSHIP ('NONE','NONE', #4578, #2890 ) REPRESENTATION_RELATIONSHIP_WITH_TRANSFORMATION ( #28608 )SHAPE_REPRESENTATION_RELATIONSHIP( ) );
#10871 = ORIENTED_EDGE ( 'NONE', *, *, #17325, .T. ) ;
#10872 = FACE_OUTER_BOUND ( 'NONE', #39425, .T. ) ;
#10873 = VERTEX_POINT ( 'NONE', #46768 ) ;
#10874 = CARTESIAN_POINT ( 'NONE',  ( 43.18784210722336780, -193.5000000000000000, -84.98333260264752198 ) ) ;
#10875 = FACE_OUTER_BOUND ( 'NONE', #11864, .T. ) ;
#10876 = EDGE_CURVE ( 'NONE', #8246, #31707, #42810, .T. ) ;
#10877 = EDGE_CURVE ( 'NONE', #3069, #2708, #29953, .T. ) ;
#10878 = EDGE_CURVE ( 'NONE', #15404, #47058, #15805, .T. ) ;
#10879 = EDGE_CURVE ( 'NONE', #42079, #45025, #14975, .T. ) ;
#10880 = LINE ( 'NONE', #3497, #33692 ) ;
#10881 = CARTESIAN_POINT ( 'NONE',  ( -490.0000000000001137, -168.5000000000000284, -14.36509618646847386 ) ) ;
#10882 = ORIENTED_EDGE ( 'NONE', *, *, #24362, .F. ) ;
#10883 = ADVANCED_FACE ( 'NONE', ( #30981 ), #18131, .T. ) ;
#10884 = EDGE_LOOP ( 'NONE', ( #26515, #1004, #34062, #25576 ) ) ;
#10885 = CARTESIAN_POINT ( 'NONE',  ( -339.1964088526558498, -175.5095439275173135, 27.86139516340941213 ) ) ;
#10886 = DIRECTION ( 'NONE',  ( 0.000000000000000000, -0.5680647467311485954, 0.8229838658936613482 ) ) ;
#10887 = CARTESIAN_POINT ( 'NONE',  ( 55.91309001144629320, -177.1207230881787780, 68.75510947788671956 ) ) ;
#10888 = VECTOR ( 'NONE', #44361, 1000.000000000000000 ) ;
#10889 = EDGE_CURVE ( 'NONE', #7181, #34020, #23107, .T. ) ;
#10890 = DIRECTION ( 'NONE',  ( 0.000000000000000000, 0.000000000000000000, 1.000000000000000000 ) ) ;
#10891 = DIRECTION ( 'NONE',  ( 0.3482016354343995812, 0.000000000000000000, -0.9374196611341205632 ) ) ;
#10892 = ORIENTED_EDGE ( 'NONE', *, *, #4906, .F. ) ;
#10893 = EDGE_CURVE ( 'NONE', #51589, #16369, #51037, .T. ) ;
#10894 = LINE ( 'NONE', #30590, #44993 ) ;
#10895 = EDGE_CURVE ( 'NONE', #50975, #39853, #2086, .T. ) ;
#10896 = ORIENTED_EDGE ( 'NONE', *, *, #9188, .F. ) ;
#10897 = ORIENTED_EDGE ( 'NONE', *, *, #1191, .T. ) ;
#10898 = DIRECTION ( 'NONE',  ( -0.000000000000000000, 0.7485107481710999711, -0.6631226582407964143 ) ) ;
#10899 = DIRECTION ( 'NONE',  ( 0.000000000000000000, 0.000000000000000000, -1.000000000000000000 ) ) ;
#10900 = EDGE_CURVE ( 'NONE', #50209, #28776, #10489, .T. ) ;
#10901 = CARTESIAN_POINT ( 'NONE',  ( 0.000000000000000000, 101.9200652401092384, -101.2342171097734536 ) ) ;
#10902 = CARTESIAN_POINT ( 'NONE',  ( -330.4913330509368166, -84.75001853787871653, -44.49369547121542467 ) ) ;
#10903 = ADVANCED_FACE ( 'NONE', ( #26259 ), #42285, .T. ) ;
#10904 = DIRECTION ( 'NONE',  ( 0.7175072570443249420, 0.000000000000000000, 0.6965510290630033685 ) ) ;
#10905 = FACE_OUTER_BOUND ( 'NONE', #24574, .T. ) ;
#10906 = ORIENTED_EDGE ( 'NONE', *, *, #44901, .T. ) ;
#10907 = CARTESIAN_POINT ( 'NONE',  ( 43.86477233319989466, -175.3837268820161057, -84.24728067915975771 ) ) ;
#10908 = EDGE_CURVE ( 'NONE', #11338, #5960, #46509, .T. ) ;
#10909 = VECTOR ( 'NONE', #36735, 1000.000000000000000 ) ;
#10910 = VECTOR ( 'NONE', #38254, 1000.000000000000000 ) ;
#10911 = EDGE_LOOP ( 'NONE', ( #28213, #43926, #28689, #14123 ) ) ;
#10912 = CYLINDRICAL_SURFACE ( 'NONE', #11147, 125.0000000000000000 ) ;
#10913 = LINE ( 'NONE', #20600, #15188 ) ;
#10914 = ORIENTED_EDGE ( 'NONE', *, *, #19617, .T. ) ;
#10915 = CARTESIAN_POINT ( 'NONE',  ( -158.0280232639029236, -175.3837268820161057, 60.19999396110247147 ) ) ;
#10916 = CARTESIAN_POINT ( 'NONE',  ( 39.18328161278951427, -193.5000000000000000, 89.10837311819236106 ) ) ;
#10917 = CARTESIAN_POINT ( 'NONE',  ( -339.1964088526558498, -167.3305728129742249, 39.49849221029288060 ) ) ;
#10918 = DIRECTION ( 'NONE',  ( 0.000000000000000000, 0.000000000000000000, 1.000000000000000000 ) ) ;
#10919 = ADVANCED_FACE ( 'NONE', ( #28058 ), #47289, .F. ) ;
#10920 = ADVANCED_FACE ( 'NONE', ( #4173 ), #39375, .F. ) ;
#10921 = CARTESIAN_POINT ( 'NONE',  ( -336.3521761649654422, -97.52665284734005979, -53.00046796564681983 ) ) ;
#10922 = ORIENTED_EDGE ( 'NONE', *, *, #9872, .T. ) ;
#10923 = VECTOR ( 'NONE', #39426, 1000.000000000000000 ) ;
#10924 = DIRECTION ( 'NONE',  ( 1.000000000000000000, 0.000000000000000000, 0.000000000000000000 ) ) ;
#10926 = ORIENTED_EDGE ( 'NONE', *, *, #7616, .T. ) ;
#10925 = CARTESIAN_POINT ( 'NONE',  ( 69.99104047056317768, -175.3837268820161057, -39.87254040532513244 ) ) ;
#10927 = EDGE_LOOP ( 'NONE', ( #26727, #7618, #15170, #28659 ) ) ;
#10928 = DIRECTION ( 'NONE',  ( 0.000000000000000000, 0.000000000000000000, 1.000000000000000000 ) ) ;
#10929 = VERTEX_POINT ( 'NONE', #11776 ) ;
#10930 = DIRECTION ( 'NONE',  ( 0.000000000000000000, 0.000000000000000000, -1.000000000000000000 ) ) ;
#10931 = ORIENTED_EDGE ( 'NONE', *, *, #38993, .T. ) ;
#10932 = LINE ( 'NONE', #31678, #50307 ) ;
#10933 = CARTESIAN_POINT ( 'NONE',  ( -339.1964088526558498, -108.8949048983213004, -57.16590939599337418 ) ) ;
#10934 = ORIENTED_EDGE ( 'NONE', *, *, #47198, .T. ) ;
#10935 = CARTESIAN_POINT ( 'NONE',  ( 71.87891646118019651, -189.7472609257535510, -33.74820638215424395 ) ) ;
#10936 = EDGE_CURVE ( 'NONE', #38286, #46129, #31768, .T. ) ;
#10937 = EDGE_CURVE ( 'NONE', #11500, #21582, #35697, .T. ) ;
#10938 = CARTESIAN_POINT ( 'NONE',  ( -97.70585564814139445, -175.3837268820161057, 113.8100815915419162 ) ) ;
#10939 = DIRECTION ( 'NONE',  ( -0.000000000000000000, 1.000000000000000000, -0.000000000000000000 ) ) ;
#10940 = EDGE_LOOP ( 'NONE', ( #31120, #51875, #6789, #23015 ) ) ;
#10941 = ORIENTED_EDGE ( 'NONE', *, *, #33375, .F. ) ;
#10943 = VERTEX_POINT ( 'NONE', #19410 ) ;
#10942 = VECTOR ( 'NONE', #12649, 1000.000000000000000 ) ;
#10944 = EDGE_CURVE ( 'NONE', #16640, #8493, #16253, .T. ) ;
#10945 = DIRECTION ( 'NONE',  ( 0.2348860457809775482, 0.000000000000000000, 0.9720229140804121926 ) ) ;
#10946 = DIRECTION ( 'NONE',  ( 0.000000000000000000, -1.000000000000000000, 0.000000000000000000 ) ) ;
#10947 = CARTESIAN_POINT ( 'NONE',  ( 74.00867759460086859, -193.5000000000000000, 24.93467037017222410 ) ) ;
#10948 = CARTESIAN_POINT ( 'NONE',  ( -19.92568551777507224, -189.7472609257535510, -121.6951149130962904 ) ) ;
#10949 = CYLINDRICAL_SURFACE ( 'NONE', #50723, 125.0000000000000000 ) ;
#10950 = ORIENTED_EDGE ( 'NONE', *, *, #42906, .T. ) ;
#10951 = CARTESIAN_POINT ( 'NONE',  ( -163.3245969606054473, -189.7472609257535510, -46.76022031560624725 ) ) ;
#10952 = VERTEX_POINT ( 'NONE', #16003 ) ;
#10954 = EDGE_LOOP ( 'NONE', ( #34539, #5241, #44350, #22231 ) ) ;
#10953 = DIRECTION ( 'NONE',  ( -0.000000000000000000, 1.000000000000000000, -0.000000000000000000 ) ) ;
#10955 = ORIENTED_EDGE ( 'NONE', *, *, #15773, .F. ) ;
#10956 = AXIS2_PLACEMENT_3D ( 'NONE', #22831, #47531, #27017 ) ;
#10957 = PLANE ( 'NONE',  #1434 ) ;
#10958 = PRODUCT_RELATED_PRODUCT_CATEGORY ( 'part', '', ( #26430 ) ) ;
#10959 = CARTESIAN_POINT ( 'NONE',  ( -101.0675409952199999, -183.6283474603465606, 113.3995532942341100 ) ) ;
#10960 = DIRECTION ( 'NONE',  ( 0.05924062789371441901, 0.000000000000000000, -0.9982437317643214625 ) ) ;
#10961 = CARTESIAN_POINT ( 'NONE',  ( -41.24387117724851493, -193.5000000000000000, 124.7904286264581231 ) ) ;
#10962 = ORIENTED_EDGE ( 'NONE', *, *, #42456, .F. ) ;
#10963 = FACE_OUTER_BOUND ( 'NONE', #42153, .T. ) ;
#10964 = VERTEX_POINT ( 'NONE', #35432 ) ;
#10965 = EDGE_CURVE ( 'NONE', #36158, #38434, #11526, .T. ) ;
#10966 = EDGE_LOOP ( 'NONE', ( #24045, #7069, #19342, #44588 ) ) ;
#10967 = LINE ( 'NONE', #42239, #41307 ) ;
#10968 = DIRECTION ( 'NONE',  ( 0.000000000000000000, 0.000000000000000000, 1.000000000000000000 ) ) ;
#10969 = DIRECTION ( 'NONE',  ( -0.000000000000000000, 1.000000000000000000, -0.000000000000000000 ) ) ;
#10970 = VERTEX_POINT ( 'NONE', #47805 ) ;
#10971 = LINE ( 'NONE', #23334, #2185 ) ;
#10972 = CARTESIAN_POINT ( 'NONE',  ( 1.959434878635765131E-15, -53.50000000000000000, 16.00000000000000000 ) ) ;
#10973 = VECTOR ( 'NONE', #46101, 1000.000000000000000 ) ;
#10974 = LINE ( 'NONE', #50940, #41429 ) ;
#10975 = CARTESIAN_POINT ( 'NONE',  ( 40.30419662299490824, -177.1207230881787780, -87.99159897727903967 ) ) ;
#10976 = EDGE_LOOP ( 'NONE', ( #15088, #29291, #1790, #48475 ) ) ;
#10977 = CARTESIAN_POINT ( 'NONE',  ( -48.47912675150885065, -177.1207230881787780, 6.938893903907228378E-15 ) ) ;
#10978 = CARTESIAN_POINT ( 'NONE',  ( -170.0000000000000284, -113.5000000000000000, 60.00000000000000711 ) ) ;
#10979 = AXIS2_PLACEMENT_3D ( 'NONE', #13640, #6017, #10209 ) ;
#10980 = CARTESIAN_POINT ( 'NONE',  ( -49.03777351731249468, -177.1207230881787780, -0.8294056854502022125 ) ) ;
#10981 = ORIENTED_EDGE ( 'NONE', *, *, #32750, .T. ) ;
#10982 = CARTESIAN_POINT ( 'NONE',  ( -305.0000000000000568, -183.4979166304964622, -0.4999999999999573119 ) ) ;
#10983 = DIRECTION ( 'NONE',  ( -0.000000000000000000, 1.000000000000000000, -0.000000000000000000 ) ) ;
#10984 = ORIENTED_EDGE ( 'NONE', *, *, #36263, .T. ) ;
#10985 = CARTESIAN_POINT ( 'NONE',  ( -305.0000000000000568, -158.9146170832377720, -48.43351006119259949 ) ) ;
#10986 = VERTEX_POINT ( 'NONE', #11258 ) ;
#10987 = DIRECTION ( 'NONE',  ( 1.000000000000000000, -0.000000000000000000, 0.000000000000000000 ) ) ;
#10988 = VECTOR ( 'NONE', #2987, 1000.000000000000114 ) ;
#10989 = FACE_BOUND ( 'NONE', #23552, .T. ) ;
#10990 = DIRECTION ( 'NONE',  ( 1.000000000000000000, -0.000000000000000000, -0.000000000000000000 ) ) ;
#10991 = EDGE_CURVE ( 'NONE', #1773, #38174, #12296, .T. ) ;
#10992 = CARTESIAN_POINT ( 'NONE',  ( -48.47912675150885065, -189.7472609257535510, 6.938893903907228378E-15 ) ) ;
#10993 = ORIENTED_EDGE ( 'NONE', *, *, #30751, .T. ) ;
#10994 = ORIENTED_EDGE ( 'NONE', *, *, #48690, .F. ) ;
#10995 = CARTESIAN_POINT ( 'NONE',  ( -118.4380981977755880, -175.3837268820161057, -102.3804074221059892 ) ) ;
#10996 = VERTEX_POINT ( 'NONE', #27802 ) ;
#10997 = DIRECTION ( 'NONE',  ( -0.000000000000000000, 1.000000000000000000, -0.000000000000000000 ) ) ;
#10998 = DIRECTION ( 'NONE',  ( -0.000000000000000000, 1.000000000000000000, 0.000000000000000000 ) ) ;
#10999 = DIRECTION ( 'NONE',  ( -0.000000000000000000, -0.5680647467311485954, 0.8229838658936613482 ) ) ;
#11000 = ORIENTED_EDGE ( 'NONE', *, *, #28955, .T. ) ;
#11003 = ORIENTED_EDGE ( 'NONE', *, *, #11052, .F. ) ;
#11002 = CARTESIAN_POINT ( 'NONE',  ( 33.25242634436025924, -189.7472609257535510, -94.57776286494160445 ) ) ;
#11001 = DIRECTION ( 'NONE',  ( 0.000000000000000000, 1.000000000000000000, 0.000000000000000000 ) ) ;
#11004 = VECTOR ( 'NONE', #9064, 1000.000000000000114 ) ;
#11005 = EDGE_CURVE ( 'NONE', #46482, #50353, #43836, .T. ) ;
#11006 = CARTESIAN_POINT ( 'NONE',  ( -120.2975302769383177, -177.1207230881787780, 102.3089288139533863 ) ) ;
#11007 = ORIENTED_EDGE ( 'NONE', *, *, #2045, .F. ) ;
#11008 = DIRECTION ( 'NONE',  ( -1.000000000000000000, 0.000000000000000000, 0.000000000000000000 ) ) ;
#11009 = ORIENTED_EDGE ( 'NONE', *, *, #22749, .T. ) ;
#11010 = LINE ( 'NONE', #28067, #5758 ) ;
#11011 = ORIENTED_EDGE ( 'NONE', *, *, #34614, .T. ) ;
#11014 = ORIENTED_EDGE ( 'NONE', *, *, #24124, .F. ) ;
#11013 = FACE_OUTER_BOUND ( 'NONE', #3338, .T. ) ;
#11012 = DIRECTION ( 'NONE',  ( 0.000000000000000000, 0.000000000000000000, -1.000000000000000000 ) ) ;
#11015 = ORIENTED_EDGE ( 'NONE', *, *, #16877, .F. ) ;
#11016 = FACE_OUTER_BOUND ( 'NONE', #32664, .T. ) ;
#11017 = ORIENTED_EDGE ( 'NONE', *, *, #28579, .F. ) ;
#11018 = DIRECTION ( 'NONE',  ( 0.000000000000000000, 0.000000000000000000, 1.000000000000000000 ) ) ;
#11020 = AXIS2_PLACEMENT_3D ( 'NONE', #15868, #31878, #28180 ) ;
#11019 = DIRECTION ( 'NONE',  ( 0.000000000000000000, 0.000000000000000000, 1.000000000000000000 ) ) ;
#11021 = ORIENTED_EDGE ( 'NONE', *, *, #36288, .F. ) ;
#11022 = DIRECTION ( 'NONE',  ( -0.000000000000000000, 1.000000000000000000, -0.000000000000000000 ) ) ;
#11023 = DIRECTION ( 'NONE',  ( 0.000000000000000000, 0.000000000000000000, 1.000000000000000000 ) ) ;
#11024 = FACE_OUTER_BOUND ( 'NONE', #27096, .T. ) ;
#11025 = LINE ( 'NONE', #27053, #13976 ) ;
#11026 = ORIENTED_EDGE ( 'NONE', *, *, #6342, .F. ) ;
#11027 = CARTESIAN_POINT ( 'NONE',  ( 0.000000000000000000, 0.000000000000000000, 0.000000000000000000 ) ) ;
#11028 = ADVANCED_FACE ( 'NONE', ( #31494 ), #15222, .T. ) ;
#11029 = CARTESIAN_POINT ( 'NONE',  ( -305.0000000000000568, -72.67320051506121104, 31.88473700876054551 ) ) ;
#11030 = DIRECTION ( 'NONE',  ( -0.000000000000000000, 0.2393156642875652051, 0.9709418174260502354 ) ) ;
#11031 = DIRECTION ( 'NONE',  ( -0.000000000000000000, 1.000000000000000000, 0.000000000000000000 ) ) ;
#11032 = ORIENTED_EDGE ( 'NONE', *, *, #47437, .T. ) ;
#11033 = EDGE_CURVE ( 'NONE', #28863, #10734, #51483, .T. ) ;
#11034 = CARTESIAN_POINT ( 'NONE',  ( -173.1763543514842070, -183.6283474603465606, 8.694908215728872847 ) ) ;
#11035 = DIRECTION ( 'NONE',  ( 0.000000000000000000, 0.000000000000000000, -1.000000000000000000 ) ) ;
#11036 = VECTOR ( 'NONE', #46670, 1000.000000000000000 ) ;
#11037 = DIRECTION ( 'NONE',  ( -1.000000000000000000, -0.000000000000000000, -0.000000000000000000 ) ) ;
#11038 = LINE ( 'NONE', #15015, #38654 ) ;
#11039 = LINE ( 'NONE', #35465, #37524 ) ;
#11040 = ORIENTED_EDGE ( 'NONE', *, *, #22414, .T. ) ;
#11041 = AXIS2_PLACEMENT_3D ( 'NONE', #17527, #29059, #32755 ) ;
#11042 = EDGE_CURVE ( 'NONE', #44752, #23503, #27559, .T. ) ;
#11043 = DIRECTION ( 'NONE',  ( -0.000000000000000000, 0.000000000000000000, -1.000000000000000000 ) ) ;
#11044 = LINE ( 'NONE', #39167, #24014 ) ;
#11045 = CARTESIAN_POINT ( 'NONE',  ( -103.4012653778457462, -177.1207230881787780, -112.2878385610366649 ) ) ;
#11046 = LINE ( 'NONE', #38397, #10303 ) ;
#11047 = CARTESIAN_POINT ( 'NONE',  ( -339.1964088526558498, -75.22798428563991990, -33.92731199008514409 ) ) ;
#11048 = ORIENTED_EDGE ( 'NONE', *, *, #15998, .T. ) ;
#11049 = ADVANCED_FACE ( 'NONE', ( #48315 ), #23866, .F. ) ;
#11050 = PLANE ( 'NONE',  #38601 ) ;
#11051 = VECTOR ( 'NONE', #33995, 1000.000000000000000 ) ;
#11052 = EDGE_CURVE ( 'NONE', #47414, #6751, #3910, .T. ) ;
#11053 = FACE_OUTER_BOUND ( 'NONE', #22633, .T. ) ;
#11054 = EDGE_LOOP ( 'NONE', ( #12678, #5379, #22373, #34080 ) ) ;
#11055 = ORIENTED_EDGE ( 'NONE', *, *, #36982, .T. ) ;
#11056 = ADVANCED_FACE ( 'NONE', ( #48050 ), #44103, .F. ) ;
#11057 = CIRCLE ( 'NONE', #20286, 125.0000000000000000 ) ;
#11058 = VERTEX_POINT ( 'NONE', #40160 ) ;
#11059 = CARTESIAN_POINT ( 'NONE',  ( 58.48829670243887335, -183.6283474603465606, -64.67588669375807342 ) ) ;
#11060 = DIRECTION ( 'NONE',  ( -1.000000000000000000, 0.000000000000000000, 0.000000000000000000 ) ) ;
#11061 = ORIENTED_EDGE ( 'NONE', *, *, #44942, .T. ) ;
#11062 = DIRECTION ( 'NONE',  ( 0.000000000000000000, -0.000000000000000000, 1.000000000000000000 ) ) ;
#11063 = LINE ( 'NONE', #32074, #19351 ) ;
#11066 = ORIENTED_EDGE ( 'NONE', *, *, #19737, .T. ) ;
#11065 = CARTESIAN_POINT ( 'NONE',  ( -129.4514457347087557, -175.3837268820161057, 95.22858582633116953 ) ) ;
#11064 = CARTESIAN_POINT ( 'NONE',  ( -336.3521761649654422, -145.9479049231020440, -54.58714071513102795 ) ) ;
#11067 = ADVANCED_FACE ( 'NONE', ( #8369 ), #24392, .T. ) ;
#11068 = CARTESIAN_POINT ( 'NONE',  ( -332.3517673607765914, -126.1322888500942554, -59.94223098458773080 ) ) ;
#11069 = ORIENTED_EDGE ( 'NONE', *, *, #12757, .F. ) ;
#11070 = CARTESIAN_POINT ( 'NONE',  ( 2.347046875550483230E-15, 20.00000000000000000, 51.00000000000000711 ) ) ;
#11071 = AXIS2_PLACEMENT_3D ( 'NONE', #26276, #15237, #38625 ) ;
#11072 = ORIENTED_EDGE ( 'NONE', *, *, #37619, .T. ) ;
#11073 = LINE ( 'NONE', #43660, #36677 ) ;
#11074 = FACE_OUTER_BOUND ( 'NONE', #13223, .T. ) ;
#11075 = VECTOR ( 'NONE', #27655, 1000.000000000000114 ) ;
#11077 = FACE_OUTER_BOUND ( 'NONE', #25365, .T. ) ;
#11076 = CARTESIAN_POINT ( 'NONE',  ( -78.00521078983982193, -189.7472609257535510, 121.4627941443857111 ) ) ;
#11078 = ORIENTED_EDGE ( 'NONE', *, *, #28090, .F. ) ;
#11079 = CIRCLE ( 'NONE', #47188, 125.0000000000000000 ) ;
#11080 = CARTESIAN_POINT ( 'NONE',  ( -336.3521761649653854, -156.2279223070262049, 50.28800156563451651 ) ) ;
#11081 = VERTEX_POINT ( 'NONE', #45240 ) ;
#11082 = CARTESIAN_POINT ( 'NONE',  ( -336.3521761649654422, -113.7752393642576720, 58.25253621232167944 ) ) ;
#11083 = DIRECTION ( 'NONE',  ( -0.000000000000000000, 0.000000000000000000, 1.000000000000000000 ) ) ;
#11084 = ORIENTED_EDGE ( 'NONE', *, *, #34397, .T. ) ;
#11085 = DIRECTION ( 'NONE',  ( 0.000000000000000000, 0.000000000000000000, -1.000000000000000000 ) ) ;
#11086 = CARTESIAN_POINT ( 'NONE',  ( -158.0280232639029236, -193.5000000000000000, 60.19999396110247147 ) ) ;
#11087 = ORIENTED_EDGE ( 'NONE', *, *, #30585, .T. ) ;
#11088 = DIRECTION ( 'NONE',  ( 1.000000000000000000, -0.000000000000000000, -0.000000000000000000 ) ) ;
#11089 = VECTOR ( 'NONE', #22117, 1000.000000000000000 ) ;
#11091 = AXIS2_PLACEMENT_3D ( 'NONE', #26730, #30407, #5751 ) ;
#11090 = CARTESIAN_POINT ( 'NONE',  ( -339.1964088526558498, -71.49045607248213230, 27.86139516340826106 ) ) ;
#11092 = ORIENTED_EDGE ( 'NONE', *, *, #42403, .T. ) ;
#11093 = CARTESIAN_POINT ( 'NONE',  ( -168.1141659785444915, -193.5000000000000000, -36.22785377503943494 ) ) ;
#11094 = ORIENTED_EDGE ( 'NONE', *, *, #26470, .T. ) ;
#11095 = VECTOR ( 'NONE', #33857, 1000.000000000000000 ) ;
#11096 = AXIS2_PLACEMENT_3D ( 'NONE', #678, #16727, #8808 ) ;
#11097 = CARTESIAN_POINT ( 'NONE',  ( 69.14211578623219623, -177.1207230881787780, 42.31126686685117733 ) ) ;
#11098 = CARTESIAN_POINT ( 'NONE',  ( 24.63024857337165585, -177.1207230881787780, 101.3904297239426455 ) ) ;
#11099 = EDGE_LOOP ( 'NONE', ( #37563, #25571, #47638, #32327 ) ) ;
#11100 = CARTESIAN_POINT ( 'NONE',  ( -60.00000000000000000, 0.000000000000000000, 60.00000000000000711 ) ) ;
#11101 = ADVANCED_FACE ( 'NONE', ( #4501 ), #28398, .T. ) ;
#11102 = CARTESIAN_POINT ( 'NONE',  ( -48.47912675150885065, -189.7472609257535510, 6.938893903907228378E-15 ) ) ;
#11103 = CARTESIAN_POINT ( 'NONE',  ( 75.51463005422469621, -193.5000000000000000, -1.322128892811228251 ) ) ;
#11104 = ADVANCED_FACE ( 'NONE', ( #20515 ), #542, .T. ) ;
#11105 = CARTESIAN_POINT ( 'NONE',  ( -336.3521761649654422, -113.7752393642576720, 58.25253621232167944 ) ) ;
#11106 = DIRECTION ( 'NONE',  ( 0.000000000000000000, 0.000000000000000000, -1.000000000000000000 ) ) ;
#11107 = PLANE ( 'NONE',  #19321 ) ;
#11109 = ORIENTED_EDGE ( 'NONE', *, *, #4283, .F. ) ;
#11108 = LINE ( 'NONE', #27395, #16967 ) ;
#11110 = AXIS2_PLACEMENT_3D ( 'NONE', #39641, #44396, #35711 ) ;
#11111 = VERTEX_POINT ( 'NONE', #813 ) ;
#11112 = LINE ( 'NONE', #6926, #9811 ) ;
#11113 = EDGE_CURVE ( 'NONE', #11286, #13263, #25844, .T. ) ;
#11114 = EDGE_CURVE ( 'NONE', #50694, #4146, #32860, .T. ) ;
#11115 = VECTOR ( 'NONE', #15801, 1000.000000000000000 ) ;
#11116 = DIRECTION ( 'NONE',  ( -0.7378332790417333475, 0.000000000000000000, 0.6749830015182038956 ) ) ;
#11117 = EDGE_LOOP ( 'NONE', ( #38271, #26151, #45224, #51145 ) ) ;
#11118 = ORIENTED_EDGE ( 'NONE', *, *, #38741, .T. ) ;
#11119 = EDGE_CURVE ( 'NONE', #44193, #32445, #21578, .T. ) ;
#11120 = CARTESIAN_POINT ( 'NONE',  ( -332.3517673607765914, -155.6724726690323450, 49.48329383994676078 ) ) ;
#11121 = EDGE_LOOP ( 'NONE', ( #45948, #12104, #49961, #47617 ) ) ;
#11122 = CARTESIAN_POINT ( 'NONE',  ( 24.63024857337166296, -183.6283474603465606, 101.3904297239426597 ) ) ;
#11123 = CARTESIAN_POINT ( 'NONE',  ( -48.36085358058748085, -177.1207230881787780, -0.9929810960135100339 ) ) ;
#11124 = EDGE_CURVE ( 'NONE', #32868, #1251, #41011, .T. ) ;
#11125 = LINE ( 'NONE', #35054, #4275 ) ;
#11126 = CARTESIAN_POINT ( 'NONE',  ( -305.0000000000000568, -78.92247586332004516, -40.16023333900979964 ) ) ;
#11127 = ORIENTED_EDGE ( 'NONE', *, *, #36574, .F. ) ;
#11128 = ORIENTED_EDGE ( 'NONE', *, *, #11873, .F. ) ;
#11129 = AXIS2_PLACEMENT_3D ( 'NONE', #32219, #48262, #9103 ) ;
#11130 = VERTEX_POINT ( 'NONE', #12628 ) ;
#11131 = LINE ( 'NONE', #6441, #38354 ) ;
#11132 = VECTOR ( 'NONE', #43293, 1000.000000000000000 ) ;
#11133 = DIRECTION ( 'NONE',  ( 0.2920567706369833760, 0.000000000000000000, -0.9564009842765202052 ) ) ;
#11134 = VECTOR ( 'NONE', #1677, 1000.000000000000000 ) ;
#11135 = CARTESIAN_POINT ( 'NONE',  ( 74.00867759460086859, -189.7472609257535510, 24.93467037017222410 ) ) ;
#11136 = CARTESIAN_POINT ( 'NONE',  ( -365.0000000000001137, -78.50000000000002842, 0.000000000000000000 ) ) ;
#11137 = EDGE_LOOP ( 'NONE', ( #31718, #5986, #16957, #21885 ) ) ;
#11138 = PRODUCT_DEFINITION_CONTEXT ( 'detailed design', #21625, 'design' ) ;
#11139 = CLOSED_SHELL ( 'NONE', ( #20890, #28797, #37961, #17608, #41968, #18010, #12995, #21531, #12824, #43779, #19886, #20350, #21982, #10731, #10765, #4483, #34353, #26007, #4785, #31352, #26245, #25529, #15629, #38744 ) ) ;
#11140 = DIRECTION ( 'NONE',  ( 0.000000000000000000, 0.000000000000000000, 1.000000000000000000 ) ) ;
#11141 = PLANE ( 'NONE',  #27369 ) ;
#11142 = VERTEX_POINT ( 'NONE', #40479 ) ;
#11143 = VERTEX_POINT ( 'NONE', #37065 ) ;
#11144 = LINE ( 'NONE', #22987, #26447 ) ;
#11145 = CARTESIAN_POINT ( 'NONE',  ( -118.4510020108455137, -193.5000000000000000, 103.5805805771131674 ) ) ;
#11146 = DIRECTION ( 'NONE',  ( -1.000000000000000000, 0.000000000000000000, -0.000000000000000000 ) ) ;
#11147 = AXIS2_PLACEMENT_3D ( 'NONE', #21714, #6470, #29839 ) ;
#11148 = DIRECTION ( 'NONE',  ( -0.000000000000000000, -1.000000000000000000, -0.000000000000000000 ) ) ;
#11149 = CARTESIAN_POINT ( 'NONE',  ( -171.4462109067799247, -193.5000000000000000, 15.97798378892250071 ) ) ;
#11150 = VERTEX_POINT ( 'NONE', #28651 ) ;
#11151 = DIRECTION ( 'NONE',  ( -0.000000000000000000, 1.000000000000000000, 0.000000000000000000 ) ) ;
#11152 = AXIS2_PLACEMENT_3D ( 'NONE', #47136, #51104, #43176 ) ;
#11153 = EDGE_LOOP ( 'NONE', ( #29674, #39881, #14988, #1193 ) ) ;
#11154 = DIRECTION ( 'NONE',  ( 1.000000000000000000, 0.000000000000000000, 0.000000000000000000 ) ) ;
#11155 = DIRECTION ( 'NONE',  ( 0.7575112421616236880, 0.000000000000000000, -0.6528221181905174975 ) ) ;
#11156 = ORIENTED_EDGE ( 'NONE', *, *, #28500, .T. ) ;
#11157 = ADVANCED_FACE ( 'NONE', ( #12371 ), #44447, .T. ) ;
#11158 = DIRECTION ( 'NONE',  ( 1.043714542225393381E-14, -0.7485107481711024136, -0.6631226582407937498 ) ) ;
#11159 = ADVANCED_FACE ( 'NONE', ( #40740 ), #29185, .F. ) ;
#11160 = DIRECTION ( 'NONE',  ( -1.000000000000000000, -0.000000000000000000, -0.000000000000000000 ) ) ;
#11161 = CARTESIAN_POINT ( 'NONE',  ( 55.35935253854128746, -193.5000000000000000, 69.58857822035042773 ) ) ;
#11162 = EDGE_CURVE ( 'NONE', #18433, #42344, #44974, .T. ) ;
#11163 = VECTOR ( 'NONE', #300, 1000.000000000000000 ) ;
#11164 = PLANE ( 'NONE',  #24057 ) ;
#11165 = AXIS2_PLACEMENT_3D ( 'NONE', #26173, #18563, #22239 ) ;
#11166 = EDGE_CURVE ( 'NONE', #2008, #8829, #36820, .T. ) ;
#11167 = LINE ( 'NONE', #27190, #41234 ) ;
#11168 = ORIENTED_EDGE ( 'NONE', *, *, #37505, .T. ) ;
#11169 = AXIS2_PLACEMENT_3D ( 'NONE', #48682, #41290, #28941 ) ;
#11170 = ADVANCED_FACE ( 'NONE', ( #12891 ), #29437, .T. ) ;
#11171 = FACE_OUTER_BOUND ( 'NONE', #5708, .T. ) ;
#11173 = ORIENTED_EDGE ( 'NONE', *, *, #23536, .F. ) ;
#11172 = CARTESIAN_POINT ( 'NONE',  ( 23.33927677392130917, -177.1207230881787780, -102.3089288139528747 ) ) ;
#11174 = VERTEX_POINT ( 'NONE', #5029 ) ;
#11175 = CARTESIAN_POINT ( 'NONE',  ( 0.000000000000000000, 101.5275612430648380, -100.5543802447186579 ) ) ;
#11176 = VECTOR ( 'NONE', #30621, 1000.000000000000114 ) ;
#11177 = EDGE_CURVE ( 'NONE', #31178, #28257, #21046, .T. ) ;
#11178 = ORIENTED_EDGE ( 'NONE', *, *, #13550, .F. ) ;
#11179 = EDGE_CURVE ( 'NONE', #19179, #46206, #34245, .T. ) ;
#11180 = FACE_OUTER_BOUND ( 'NONE', #21346, .T. ) ;
#11181 = ORIENTED_EDGE ( 'NONE', *, *, #23771, .F. ) ;
#11182 = EDGE_CURVE ( 'NONE', #15096, #5889, #41263, .T. ) ;
#11183 = DIRECTION ( 'NONE',  ( -0.000000000000000000, 1.000000000000000000, -0.000000000000000000 ) ) ;
#11184 = CARTESIAN_POINT ( 'NONE',  ( -339.1964088526558498, -102.1108035431478811, -54.98865587491830809 ) ) ;
#11185 = ORIENTED_EDGE ( 'NONE', *, *, #37515, .F. ) ;
#11186 = DIRECTION ( 'NONE',  ( -0.02963332782255633305, 0.000000000000000000, -0.9995608365087944591 ) ) ;
#11187 = AXIS2_PLACEMENT_3D ( 'NONE', #34691, #47315, #11283 ) ;
#11188 = EDGE_CURVE ( 'NONE', #41176, #24784, #21651, .T. ) ;
#11189 = CARTESIAN_POINT ( 'NONE',  ( 60.90550954139437323, -189.7472609257535510, 60.49794494914088006 ) ) ;
#11190 = DIRECTION ( 'NONE',  ( -0.000000000000000000, 1.000000000000000000, -0.000000000000000000 ) ) ;
#11191 = ORIENTED_EDGE ( 'NONE', *, *, #4318, .F. ) ;
#11192 = VERTEX_POINT ( 'NONE', #29697 ) ;
#11193 = EDGE_CURVE ( 'NONE', #41557, #14780, #33645, .T. ) ;
#11194 = AXIS2_PLACEMENT_3D ( 'NONE', #41836, #1887, #17924 ) ;
#11195 = EDGE_LOOP ( 'NONE', ( #48481, #43948, #44928, #5191 ) ) ;
#11196 = DIRECTION ( 'NONE',  ( -0.000000000000000000, 1.000000000000000000, -0.000000000000000000 ) ) ;
#11197 = CARTESIAN_POINT ( 'NONE',  ( -146.0653709326077490, -193.5000000000000000, -78.11481899503411341 ) ) ;
#11198 = CARTESIAN_POINT ( 'NONE',  ( -139.0630283577175987, -193.5000000000000000, -86.13684908212448477 ) ) ;
#11199 = CARTESIAN_POINT ( 'NONE',  ( -280.0000000000000000, -63.50000000000000000, -60.00000000000000711 ) ) ;
#11200 = DIRECTION ( 'NONE',  ( 0.000000000000000000, 0.000000000000000000, 1.000000000000000000 ) ) ;
#11201 = ORIENTED_EDGE ( 'NONE', *, *, #17617, .F. ) ;
#11202 = EDGE_CURVE ( 'NONE', #29300, #11668, #6581, .T. ) ;
#11203 = DIRECTION ( 'NONE',  ( -0.000000000000000000, 1.000000000000000000, -0.000000000000000000 ) ) ;
#11204 = ORIENTED_EDGE ( 'NONE', *, *, #38553, .F. ) ;
#11206 = EDGE_LOOP ( 'NONE', ( #8910, #13090, #30888, #38558 ) ) ;
#11205 = CARTESIAN_POINT ( 'NONE',  ( -1.578537454945990293, -177.1207230881787780, 114.7887733785766926 ) ) ;
#11207 = VECTOR ( 'NONE', #51694, 1000.000000000000000 ) ;
#11208 = ORIENTED_EDGE ( 'NONE', *, *, #26181, .F. ) ;
#11209 = CARTESIAN_POINT ( 'NONE',  ( -46.00000000000000711, 0.000000000000000000, 41.00000000000000000 ) ) ;
#11210 = CARTESIAN_POINT ( 'NONE',  ( -47.82630463331832971, -193.5000000000000000, -0.7575112421616121416 ) ) ;
#11211 = DIRECTION ( 'NONE',  ( -0.000000000000000000, 1.000000000000000000, -0.000000000000000000 ) ) ;
#11212 = DIRECTION ( 'NONE',  ( 0.000000000000000000, -1.892005071132037688E-13, 1.000000000000000000 ) ) ;
#11213 = ORIENTED_EDGE ( 'NONE', *, *, #21509, .F. ) ;
#11214 = PLANE ( 'NONE',  #37607 ) ;
#11215 = ORIENTED_EDGE ( 'NONE', *, *, #39035, .T. ) ;
#11216 = EDGE_CURVE ( 'NONE', #33918, #21157, #41788, .T. ) ;
#11217 = ORIENTED_EDGE ( 'NONE', *, *, #51911, .F. ) ;
#11218 = DIRECTION ( 'NONE',  ( 0.000000000000000000, 0.000000000000000000, -1.000000000000000000 ) ) ;
#11219 = DIRECTION ( 'NONE',  ( 0.000000000000000000, -1.000000000000000000, 0.000000000000000000 ) ) ;
#11220 = LINE ( 'NONE', #35394, #36620 ) ;
#11221 = AXIS2_PLACEMENT_3D ( 'NONE', #38316, #50674, #42784 ) ;
#11222 = FACE_OUTER_BOUND ( 'NONE', #20239, .T. ) ;
#11223 = EDGE_CURVE ( 'NONE', #33816, #30271, #34168, .T. ) ;
#11224 = EDGE_CURVE ( 'NONE', #50838, #3877, #22075, .T. ) ;
#11225 = FACE_OUTER_BOUND ( 'NONE', #30341, .T. ) ;
#11226 = LINE ( 'NONE', #35928, #10282 ) ;
#11227 = ORIENTED_EDGE ( 'NONE', *, *, #6087, .F. ) ;
#11228 = CARTESIAN_POINT ( 'NONE',  ( -336.3521761649654422, -142.8954717479169574, 55.74477592174805096 ) ) ;
#11229 = FACE_OUTER_BOUND ( 'NONE', #7943, .T. ) ;
#11230 = CIRCLE ( 'NONE', #26353, 125.0000000000000000 ) ;
#11231 = EDGE_CURVE ( 'NONE', #24601, #38717, #6827, .T. ) ;
#11232 = EDGE_CURVE ( 'NONE', #29743, #37750, #34671, .T. ) ;
#11233 = DIRECTION ( 'NONE',  ( 0.000000000000000000, 1.000000000000000000, -0.000000000000000000 ) ) ;
#11234 = EDGE_LOOP ( 'NONE', ( #1218, #40669, #18444, #47972 ) ) ;
#11235 = DIRECTION ( 'NONE',  ( 0.9995608365087942371, 0.000000000000000000, 0.02963332782256331357 ) ) ;
#11236 = CARTESIAN_POINT ( 'NONE',  ( 57.12946453413545100, -193.5000000000000000, 66.87170886602000053 ) ) ;
#11237 = ORIENTED_EDGE ( 'NONE', *, *, #11456, .T. ) ;
#11238 = LINE ( 'NONE', #10985, #26255 ) ;
#11239 = CIRCLE ( 'NONE', #10414, 125.0000000000000000 ) ;
#11240 = ORIENTED_EDGE ( 'NONE', *, *, #44319, .T. ) ;
#11241 = DIRECTION ( 'NONE',  ( 0.3482016354344059095, 0.000000000000000000, -0.9374196611341183427 ) ) ;
#11242 = EDGE_CURVE ( 'NONE', #43197, #16239, #26735, .T. ) ;
#11243 = FACE_BOUND ( 'NONE', #50206, .T. ) ;
#11244 = CARTESIAN_POINT ( 'NONE',  ( -160.0000000000000284, -123.5000000000000284, -45.63467731922664683 ) ) ;
#11245 = EDGE_CURVE ( 'NONE', #12900, #34513, #25768, .T. ) ;
#11246 = DIRECTION ( 'NONE',  ( 0.5829794791144650157, 0.000000000000000000, 0.8124868780056864193 ) ) ;
#11247 = ORIENTED_EDGE ( 'NONE', *, *, #23092, .F. ) ;
#11248 = EDGE_CURVE ( 'NONE', #41150, #10561, #26019, .T. ) ;
#11249 = ORIENTED_EDGE ( 'NONE', *, *, #40496, .F. ) ;
#11250 = CARTESIAN_POINT ( 'NONE',  ( -169.0136227435421006, -193.5000000000000000, -33.11246405730811659 ) ) ;
#11251 = ORIENTED_EDGE ( 'NONE', *, *, #22048, .F. ) ;
#11252 = DIRECTION ( 'NONE',  ( -0.000000000000000000, 0.9927088740980556381, 0.1205366802553095307 ) ) ;
#11253 = AXIS2_PLACEMENT_3D ( 'NONE', #39902, #35989, #23627 ) ;
#11254 = VECTOR ( 'NONE', #31076, 1000.000000000000000 ) ;
#11255 =( NAMED_UNIT ( * ) PLANE_ANGLE_UNIT ( ) SI_UNIT ( $, .RADIAN. ) );
#11256 = CARTESIAN_POINT ( 'NONE',  ( 75.12566530717464275, -193.5000000000000000, 18.62405380494841367 ) ) ;
#11257 = EDGE_LOOP ( 'NONE', ( #49481, #40031, #39786, #26060 ) ) ;
#11260 = ORIENTED_EDGE ( 'NONE', *, *, #27907, .T. ) ;
#11259 = CARTESIAN_POINT ( 'NONE',  ( -147.0463339291296165, -183.6283474603465606, 76.87330921200147316 ) ) ;
#11258 = CARTESIAN_POINT ( 'NONE',  ( -19.92568551777506869, -175.3837268820161057, -121.6951149130962904 ) ) ;
#11261 = CARTESIAN_POINT ( 'NONE',  ( -330.4913330509368166, -162.9984922102920848, 43.83057281297495678 ) ) ;
#11262 = ORIENTED_EDGE ( 'NONE', *, *, #25374, .F. ) ;
#11263 = CARTESIAN_POINT ( 'NONE',  ( -339.1964088526558498, -130.1153096980153236, -58.63009191191284941 ) ) ;
#11264 = ORIENTED_EDGE ( 'NONE', *, *, #47091, .F. ) ;
#11265 = FACE_OUTER_BOUND ( 'NONE', #2520, .T. ) ;
#11266 = ORIENTED_EDGE ( 'NONE', *, *, #14751, .T. ) ;
#11268 = CARTESIAN_POINT ( 'NONE',  ( -330.4913330509368166, -79.66942718702547666, -39.49849221029252533 ) ) ;
#11267 = CARTESIAN_POINT ( 'NONE',  ( -123.4791267515088435, -173.5000000000000284, 60.00000000000001421 ) ) ;
#11269 = ORIENTED_EDGE ( 'NONE', *, *, #39480, .T. ) ;
#11270 = DIRECTION ( 'NONE',  ( -0.9785564922995060311, 0.000000000000000000, 0.2059786187410889424 ) ) ;
#11271 = ORIENTED_EDGE ( 'NONE', *, *, #18657, .T. ) ;
#11272 = LINE ( 'NONE', #42300, #40439 ) ;
#11273 = DIRECTION ( 'NONE',  ( 0.000000000000000000, -0.000000000000000000, 1.000000000000000000 ) ) ;
#11274 = VERTEX_POINT ( 'NONE', #41800 ) ;
#11275 = CARTESIAN_POINT ( 'NONE',  ( -168.4003408533108086, -193.5000000000000000, -35.26900067126609173 ) ) ;
#11276 = LINE ( 'NONE', #42832, #40911 ) ;
#11277 = DIRECTION ( 'NONE',  ( 0.000000000000000000, -0.000000000000000000, 1.000000000000000000 ) ) ;
#11278 = CARTESIAN_POINT ( 'NONE',  ( -339.1964088526558498, -144.8891964568517778, 54.98865587491845730 ) ) ;
#11279 = ORIENTED_EDGE ( 'NONE', *, *, #23363, .F. ) ;
#11280 = EDGE_CURVE ( 'NONE', #6134, #39742, #13678, .T. ) ;
#11281 = EDGE_CURVE ( 'NONE', #4514, #5217, #17501, .T. ) ;
#11282 = DIRECTION ( 'NONE',  ( 0.000000000000000000, 0.000000000000000000, 1.000000000000000000 ) ) ;
#11283 = DIRECTION ( 'NONE',  ( 0.000000000000000000, 0.000000000000000000, -1.000000000000000000 ) ) ;
#11284 = DIRECTION ( 'NONE',  ( -0.9473263538541876194, 0.000000000000000000, -0.3202698538628486746 ) ) ;
#11285 = DIRECTION ( 'NONE',  ( 0.000000000000000000, 0.000000000000000000, -1.000000000000000000 ) ) ;
#11286 = VERTEX_POINT ( 'NONE', #42292 ) ;
#11287 = CARTESIAN_POINT ( 'NONE',  ( -332.3517673607765914, -128.9912765084839066, 58.76657425099337928 ) ) ;
#11288 = DIRECTION ( 'NONE',  ( 1.000000000000000000, 0.000000000000000000, 0.000000000000000000 ) ) ;
#11289 = AXIS2_PLACEMENT_3D ( 'NONE', #30722, #6056, #46267 ) ;
#11290 = CIRCLE ( 'NONE', #42361, 125.0000000000000000 ) ;
#11291 = PLANE ( 'NONE',  #22725 ) ;
#11293 = ORIENTED_EDGE ( 'NONE', *, *, #39099, .F. ) ;
#11292 = DIRECTION ( 'NONE',  ( -0.000000000000000000, 1.000000000000000000, 0.000000000000000000 ) ) ;
#11294 = VERTEX_POINT ( 'NONE', #34421 ) ;
#11295 = ORIENTED_EDGE ( 'NONE', *, *, #43639, .F. ) ;
#11296 = VECTOR ( 'NONE', #43045, 1000.000000000000000 ) ;
#11297 = DIRECTION ( 'NONE',  ( -0.000000000000000000, -1.000000000000000000, -0.000000000000000000 ) ) ;
#11298 = DIRECTION ( 'NONE',  ( 0.000000000000000000, 0.000000000000000000, -1.000000000000000000 ) ) ;
#11299 = DIRECTION ( 'NONE',  ( 0.000000000000000000, 0.000000000000000000, -1.000000000000000000 ) ) ;
#11301 = ADVANCED_FACE ( 'NONE', ( #6312 ), #14714, .F. ) ;
#11300 = CIRCLE ( 'NONE', #13871, 125.0000000000000000 ) ;
#11302 = FACE_OUTER_BOUND ( 'NONE', #20053, .T. ) ;
#11303 = DIRECTION ( 'NONE',  ( 0.000000000000000000, -0.000000000000000000, 1.000000000000000000 ) ) ;
#11304 = ORIENTED_EDGE ( 'NONE', *, *, #17021, .T. ) ;
#11305 = VECTOR ( 'NONE', #46323, 1000.000000000000000 ) ;
#11306 = CARTESIAN_POINT ( 'NONE',  ( 50.70030191143631271, -177.1207230881787780, -76.08180419845319875 ) ) ;
#11307 = EDGE_CURVE ( 'NONE', #42630, #12033, #46516, .T. ) ;
#11308 = EDGE_LOOP ( 'NONE', ( #36226, #35708, #36346, #8273 ) ) ;
#11309 = ORIENTED_EDGE ( 'NONE', *, *, #31059, .T. ) ;
#11310 = ORIENTED_EDGE ( 'NONE', *, *, #41674, .F. ) ;
#11311 = LINE ( 'NONE', #37051, #50231 ) ;
#11312 = EDGE_CURVE ( 'NONE', #45236, #23329, #40990, .T. ) ;
#11313 = PLANE ( 'NONE',  #22819 ) ;
#11314 = VERTEX_POINT ( 'NONE', #33897 ) ;
#11315 = DIRECTION ( 'NONE',  ( 0.000000000000000000, -1.000000000000000000, 0.000000000000000000 ) ) ;
#11316 = CARTESIAN_POINT ( 'NONE',  ( 21.47984469475713354, -193.5000000000000000, 102.3804074221065292 ) ) ;
#11319 = ORIENTED_EDGE ( 'NONE', *, *, #16543, .T. ) ;
#11318 = DIRECTION ( 'NONE',  ( -0.000000000000000000, -0.9709418174260502354, 0.2393156642875652051 ) ) ;
#11317 = CARTESIAN_POINT ( 'NONE',  ( 71.18041382641612813, -175.3837268820161057, -32.52067927015754378 ) ) ;
#11320 = AXIS2_PLACEMENT_3D ( 'NONE', #45316, #33723, #30042 ) ;
#11321 = CARTESIAN_POINT ( 'NONE',  ( 51.78320179844649118, -189.7472609257535510, -72.96212019587142095 ) ) ;
#11322 = CIRCLE ( 'NONE', #10511, 4.999999999999997335 ) ;
#11323 = ORIENTED_EDGE ( 'NONE', *, *, #42027, .T. ) ;
#11324 = CARTESIAN_POINT ( 'NONE',  ( -336.3521761649654422, -70.49953203435293858, 25.97334715265942151 ) ) ;
#11325 = VERTEX_POINT ( 'NONE', #22606 ) ;
#11326 = AXIS2_PLACEMENT_3D ( 'NONE', #6004, #2829, #18854 ) ;
#11327 = PLANE ( 'NONE',  #15725 ) ;
#11328 = CARTESIAN_POINT ( 'NONE',  ( -336.3521761649654422, -92.15051119686104641, -50.05135858667769355 ) ) ;
#11330 = DIRECTION ( 'NONE',  ( -0.000000000000000000, 1.000000000000000000, -0.000000000000000000 ) ) ;
#11329 = FACE_OUTER_BOUND ( 'NONE', #13883, .T. ) ;
#11331 = CIRCLE ( 'NONE', #50825, 125.0000000000000000 ) ;
#11332 = ORIENTED_EDGE ( 'NONE', *, *, #33687, .T. ) ;
#11333 = EDGE_CURVE ( 'NONE', #30259, #8199, #49943, .T. ) ;
#11334 = CARTESIAN_POINT ( 'NONE',  ( -43.48323084606168720, -183.6283474603465606, 124.9001241957026167 ) ) ;
#11335 = ORIENTED_EDGE ( 'NONE', *, *, #42160, .T. ) ;
#11336 = LINE ( 'NONE', #3456, #5512 ) ;
#11337 = CARTESIAN_POINT ( 'NONE',  ( 0.000000000000000000, -150.9186671505826212, -52.24190551353930090 ) ) ;
#11338 = VERTEX_POINT ( 'NONE', #29966 ) ;
#11339 = AXIS2_PLACEMENT_3D ( 'NONE', #5478, #1249, #1522 ) ;
#11340 = LINE ( 'NONE', #27112, #28263 ) ;
#11341 = AXIS2_PLACEMENT_3D ( 'NONE', #41629, #21678, #26378 ) ;
#11342 = LINE ( 'NONE', #46339, #487 ) ;
#11343 = ORIENTED_EDGE ( 'NONE', *, *, #34142, .T. ) ;
#11344 = EDGE_CURVE ( 'NONE', #31867, #39679, #2374, .T. ) ;
#11345 = LINE ( 'NONE', #27377, #24242 ) ;
#11346 = AXIS2_PLACEMENT_3D ( 'NONE', #28121, #18972, #6881 ) ;
#11347 = CARTESIAN_POINT ( 'NONE',  ( 73.80528149577284580, -175.3837268820161057, 25.91377046305969145 ) ) ;
#11348 = VECTOR ( 'NONE', #44625, 1000.000000000000000 ) ;
#11349 = EDGE_LOOP ( 'NONE', ( #9887, #15143, #18195, #36749 ) ) ;
#11350 = DIRECTION ( 'NONE',  ( 0.3482016354343928088, 0.000000000000000000, 0.9374196611341231167 ) ) ;
#11351 = ORIENTED_EDGE ( 'NONE', *, *, #8391, .F. ) ;
#11352 = ADVANCED_FACE ( 'NONE', ( #10008 ), #2619, .T. ) ;
#11353 = LINE ( 'NONE', #43435, #29831 ) ;
#11354 = DIRECTION ( 'NONE',  ( 0.000000000000000000, -1.000000000000000000, 0.000000000000000000 ) ) ;
#11355 = LINE ( 'NONE', #27388, #3396 ) ;
#11356 = DIRECTION ( 'NONE',  ( 0.8455960035018234011, 0.000000000000000000, 0.5338233779647948429 ) ) ;
#11357 = DIRECTION ( 'NONE',  ( 0.000000000000000000, -1.000000000000000000, 0.000000000000000000 ) ) ;
#11358 = CARTESIAN_POINT ( 'NONE',  ( 76.48781641346532467, -175.3837268820161057, 2.874563619424056249 ) ) ;
#11359 = CIRCLE ( 'NONE', #24807, 124.9999999999999858 ) ;
#11360 = PLANE ( 'NONE',  #32874 ) ;
#11361 = ADVANCED_FACE ( 'NONE', ( #7085 ), #31776, .F. ) ;
#11362 = CARTESIAN_POINT ( 'NONE',  ( -305.0000000000000568, -179.4217241332784454, -21.74306257088699113 ) ) ;
#11364 = ORIENTED_EDGE ( 'NONE', *, *, #2860, .F. ) ;
#11363 = DIRECTION ( 'NONE',  ( -0.000000000000000000, 1.000000000000000000, 0.000000000000000000 ) ) ;
#11365 = AXIS2_PLACEMENT_3D ( 'NONE', #6388, #26603, #47104 ) ;
#11366 = AXIS2_PLACEMENT_3D ( 'NONE', #45511, #25790, #33430 ) ;
#11367 = ORIENTED_EDGE ( 'NONE', *, *, #32725, .T. ) ;
#11368 = CARTESIAN_POINT ( 'NONE',  ( 44.58442300236217903, -183.6283474603465606, -81.94739446021065987 ) ) ;
#11369 = FACE_OUTER_BOUND ( 'NONE', #13257, .T. ) ;
#11370 = ORIENTED_EDGE ( 'NONE', *, *, #49702, .F. ) ;
#11371 = VERTEX_POINT ( 'NONE', #15230 ) ;
#11372 = PLANE ( 'NONE',  #10529 ) ;
#11373 = VECTOR ( 'NONE', #37328, 1000.000000000000000 ) ;
#11374 = ORIENTED_EDGE ( 'NONE', *, *, #2149, .T. ) ;
#11375 = DIRECTION ( 'NONE',  ( -0.000000000000000000, 0.6631226582407937498, -0.7485107481711024136 ) ) ;
#11376 = DIRECTION ( 'NONE',  ( 0.000000000000000000, 1.000000000000000000, -0.000000000000000000 ) ) ;
#11377 = AXIS2_PLACEMENT_3D ( 'NONE', #45125, #9113, #25142 ) ;
#11379 = AXIS2_PLACEMENT_3D ( 'NONE', #27106, #8184, #32090 ) ;
#11378 = PLANE ( 'NONE',  #50442 ) ;
#11380 = LINE ( 'NONE', #11126, #3967 ) ;
#11381 = ORIENTED_EDGE ( 'NONE', *, *, #23363, .T. ) ;
#11382 = ORIENTED_EDGE ( 'NONE', *, *, #32604, .T. ) ;
#11383 = ORIENTED_EDGE ( 'NONE', *, *, #36103, .F. ) ;
#11384 = VECTOR ( 'NONE', #48714, 999.9999999999998863 ) ;
#11385 = CYLINDRICAL_SURFACE ( 'NONE', #10674, 125.0000000000000000 ) ;
#11386 = CARTESIAN_POINT ( 'NONE',  ( -332.3517673607765914, -146.8829211657874794, -54.23253582808848705 ) ) ;
#11387 = CARTESIAN_POINT ( 'NONE',  ( -339.1964088526558498, -151.3613951634084742, 52.00954392751779665 ) ) ;
#11388 = DIRECTION ( 'NONE',  ( 0.000000000000000000, 0.000000000000000000, 1.000000000000000000 ) ) ;
#11389 = CARTESIAN_POINT ( 'NONE',  ( 64.01121016852529522, -189.7472609257535510, -54.50618404930953176 ) ) ;
#11390 = ORIENTED_EDGE ( 'NONE', *, *, #31050, .F. ) ;
#11391 = EDGE_CURVE ( 'NONE', #8199, #46931, #38872, .T. ) ;
#11392 = DIRECTION ( 'NONE',  ( -0.000000000000000000, 1.000000000000000000, -0.000000000000000000 ) ) ;
#11393 = CARTESIAN_POINT ( 'NONE',  ( 75.95066919219054569, -189.7472609257535510, -11.92584929509534852 ) ) ;
#11394 = ORIENTED_EDGE ( 'NONE', *, *, #22257, .T. ) ;
#11395 = VERTEX_POINT ( 'NONE', #7355 ) ;
#11396 = AXIS2_PLACEMENT_3D ( 'NONE', #27588, #7615, #39651 ) ;
#11397 = ORIENTED_EDGE ( 'NONE', *, *, #31124, .F. ) ;
#11398 = CARTESIAN_POINT ( 'NONE',  ( -339.1964088526558498, -123.5000000000000284, 0.000000000000000000 ) ) ;
#11399 = DIRECTION ( 'NONE',  ( 0.000000000000000000, 0.000000000000000000, 1.000000000000000000 ) ) ;
#11400 = ORIENTED_EDGE ( 'NONE', *, *, #44901, .F. ) ;
#11401 = LINE ( 'NONE', #35844, #9779 ) ;
#11402 = AXIS2_PLACEMENT_3D ( 'NONE', #16610, #32620, #17123 ) ;
#11403 = AXIS2_PLACEMENT_3D ( 'NONE', #34742, #50285, #2689 ) ;
#11404 = CARTESIAN_POINT ( 'NONE',  ( -330.4913330509368166, -157.4273119900852578, -48.27201571436002325 ) ) ;
#11405 = LINE ( 'NONE', #38745, #46972 ) ;
#11406 = ORIENTED_EDGE ( 'NONE', *, *, #40895, .F. ) ;
#11407 = EDGE_CURVE ( 'NONE', #32138, #29000, #11010, .T. ) ;
#11408 = DIRECTION ( 'NONE',  ( 0.000000000000000000, 0.000000000000000000, -1.000000000000000000 ) ) ;
#11409 = ADVANCED_FACE ( 'NONE', ( #18906 ), #19674, .T. ) ;
#11410 = ORIENTED_EDGE ( 'NONE', *, *, #34001, .T. ) ;
#11411 = DIRECTION ( 'NONE',  ( -0.000000000000000000, 1.000000000000000000, -0.000000000000000000 ) ) ;
#11412 = ADVANCED_FACE ( 'NONE', ( #52026 ), #23616, .T. ) ;
#11413 = VECTOR ( 'NONE', #44541, 1000.000000000000000 ) ;
#11414 = LINE ( 'NONE', #15379, #48004 ) ;
#11415 = ORIENTED_EDGE ( 'NONE', *, *, #12162, .T. ) ;
#11416 = CIRCLE ( 'NONE', #31559, 125.0000000000000000 ) ;
#11417 = CARTESIAN_POINT ( 'NONE',  ( 51.70113075622899856, 30.00000000000000355, -45.78969942005421956 ) ) ;
#11418 = FACE_OUTER_BOUND ( 'NONE', #27877, .T. ) ;
#11419 = FACE_OUTER_BOUND ( 'NONE', #33409, .T. ) ;
#11420 = VECTOR ( 'NONE', #13174, 1000.000000000000114 ) ;
#11421 = CARTESIAN_POINT ( 'NONE',  ( -305.0000000000000568, -152.8183901354257159, -52.34913561719022113 ) ) ;
#11423 = AXIS2_PLACEMENT_3D ( 'NONE', #15617, #42943, #27690 ) ;
#11422 = DIRECTION ( 'NONE',  ( 0.000000000000000000, 0.4647231720437604574, -0.8854560256532141294 ) ) ;
#11424 = ORIENTED_EDGE ( 'NONE', *, *, #22331, .F. ) ;
#11425 = VERTEX_POINT ( 'NONE', #22853 ) ;
#11426 = CARTESIAN_POINT ( 'NONE',  ( -339.1964088526558498, -182.1300919119128423, 6.615309698015510165 ) ) ;
#11428 = ORIENTED_EDGE ( 'NONE', *, *, #1188, .T. ) ;
#11427 = PLANE ( 'NONE',  #42191 ) ;
#11429 = EDGE_LOOP ( 'NONE', ( #18246, #25164, #3610, #16788 ) ) ;
#11430 = CARTESIAN_POINT ( 'NONE',  ( -172.4195137048758681, -189.7472609257535510, -3.844569333772463793 ) ) ;
#11431 = LINE ( 'NONE', #31411, #29338 ) ;
#11432 = AXIS2_PLACEMENT_3D ( 'NONE', #17264, #32763, #24612 ) ;
#11433 = AXIS2_PLACEMENT_3D ( 'NONE', #34964, #366, #16422 ) ;
#11434 = ORIENTED_EDGE ( 'NONE', *, *, #25960, .F. ) ;
#11435 = DIRECTION ( 'NONE',  ( 0.000000000000000000, -1.000000000000000000, 0.000000000000000000 ) ) ;
#11436 = DIRECTION ( 'NONE',  ( 0.000000000000000000, 0.000000000000000000, 1.000000000000000000 ) ) ;
#11437 = ORIENTED_EDGE ( 'NONE', *, *, #7030, .F. ) ;
#11438 = CARTESIAN_POINT ( 'NONE',  ( -260.0000000000000000, -123.5000000000000284, 6.938893903907228378E-15 ) ) ;
#11439 = CIRCLE ( 'NONE', #35791, 125.0000000000000000 ) ;
#11440 = CARTESIAN_POINT ( 'NONE',  ( 62.59443091842027940, -183.6283474603465606, -57.33816169485142211 ) ) ;
#11441 = CARTESIAN_POINT ( 'NONE',  ( -336.3521761649654422, -146.8829211657874794, -54.23253582808848705 ) ) ;
#11442 = ORIENTED_EDGE ( 'NONE', *, *, #40496, .T. ) ;
#11443 = ORIENTED_EDGE ( 'NONE', *, *, #7621, .F. ) ;
#11444 = VERTEX_POINT ( 'NONE', #44112 ) ;
#11445 = DIRECTION ( 'NONE',  ( 0.000000000000000000, 0.000000000000000000, -1.000000000000000000 ) ) ;
#11446 = CARTESIAN_POINT ( 'NONE',  ( 62.43652093785069468, -183.6283474603465606, 55.44293326708522329 ) ) ;
#11447 = AXIS2_PLACEMENT_3D ( 'NONE', #31378, #27440, #42951 ) ;
#11448 = AXIS2_PLACEMENT_3D ( 'NONE', #42059, #18156, #48922 ) ;
#11449 = DIRECTION ( 'NONE',  ( -0.2635871660690783380, 0.000000000000000000, 0.9646355819083558547 ) ) ;
#11450 = VECTOR ( 'NONE', #21267, 999.9999999999998863 ) ;
#11452 = AXIS2_PLACEMENT_3D ( 'NONE', #17188, #49250, #45054 ) ;
#11451 = CARTESIAN_POINT ( 'NONE',  ( -305.0000000000000568, -64.87442053112221174, 12.76876783163883111 ) ) ;
#11453 = CYLINDRICAL_SURFACE ( 'NONE', #18818, 4.000000000000003553 ) ;
#11454 = ORIENTED_EDGE ( 'NONE', *, *, #5633, .T. ) ;
#11455 = EDGE_CURVE ( 'NONE', #46710, #2495, #39384, .T. ) ;
#11456 = EDGE_CURVE ( 'NONE', #35941, #33506, #40127, .T. ) ;
#11457 = ADVANCED_FACE ( 'NONE', ( #11265 ), #34924, .T. ) ;
#11458 = VECTOR ( 'NONE', #40085, 1000.000000000000114 ) ;
#11459 = EDGE_CURVE ( 'NONE', #17674, #30731, #35704, .T. ) ;
#11460 = VECTOR ( 'NONE', #30535, 999.9999999999998863 ) ;
#11461 = CARTESIAN_POINT ( 'NONE',  ( -164.6246685127424882, -193.5000000000000000, -46.20836643930983456 ) ) ;
#11462 = EDGE_LOOP ( 'NONE', ( #28685, #24706, #15311, #17986 ) ) ;
#11464 = ORIENTED_EDGE ( 'NONE', *, *, #30117, .T. ) ;
#11463 = DIRECTION ( 'NONE',  ( 0.000000000000000000, 0.000000000000000000, 1.000000000000000000 ) ) ;
#11465 = ORIENTED_EDGE ( 'NONE', *, *, #25590, .F. ) ;
#11466 = ADVANCED_FACE ( 'NONE', ( #19418 ), #43078, .F. ) ;
#11467 = CARTESIAN_POINT ( 'NONE',  ( -12.00000000000000000, 65.00000000000000000, 2.265876312981440552E-15 ) ) ;
#11468 = EDGE_CURVE ( 'NONE', #43678, #34495, #51757, .T. ) ;
#11469 = PLANE ( 'NONE',  #14070 ) ;
#11470 = CARTESIAN_POINT ( 'NONE',  ( 72.71365293123227502, -183.6283474603465606, -30.61552143554913030 ) ) ;
#11471 = CARTESIAN_POINT ( 'NONE',  ( -339.1964088526558498, -123.5000000000000284, 0.000000000000000000 ) ) ;
#11472 = VERTEX_POINT ( 'NONE', #39633 ) ;
#11473 = EDGE_CURVE ( 'NONE', #49349, #27618, #3139, .T. ) ;
#11474 = DIRECTION ( 'NONE',  ( -0.000000000000000000, -3.491481338843133355E-15, -1.000000000000000000 ) ) ;
#11475 = ORIENTED_EDGE ( 'NONE', *, *, #18134, .T. ) ;
#11476 = EDGE_CURVE ( 'NONE', #9197, #51141, #24195, .T. ) ;
#11477 = ORIENTED_EDGE ( 'NONE', *, *, #32402, .F. ) ;
#11478 = DIRECTION ( 'NONE',  ( -0.000000000000000000, 1.000000000000000000, 0.000000000000000000 ) ) ;
#11479 = AXIS2_PLACEMENT_3D ( 'NONE', #51393, #35341, #11936 ) ;
#11480 = DIRECTION ( 'NONE',  ( -0.08879589532293158394, 0.000000000000000000, -0.9960498426152172291 ) ) ;
#11481 = VECTOR ( 'NONE', #2461, 1000.000000000000000 ) ;
#11482 = EDGE_CURVE ( 'NONE', #48404, #19489, #11539, .T. ) ;
#11483 = DIRECTION ( 'NONE',  ( 0.000000000000000000, -0.8229838658936575735, -0.5680647467311540355 ) ) ;
#11484 = DIRECTION ( 'NONE',  ( 0.000000000000000000, 0.000000000000000000, 1.000000000000000000 ) ) ;
#11485 = VECTOR ( 'NONE', #2206, 1000.000000000000341 ) ;
#11486 = ADVANCED_FACE ( 'NONE', ( #27567 ), #43599, .T. ) ;
#11487 = DIRECTION ( 'NONE',  ( -0.000000000000000000, 1.000000000000000000, 0.000000000000000000 ) ) ;
#11488 = DIRECTION ( 'NONE',  ( 0.2348860457809775482, 0.000000000000000000, 0.9720229140804121926 ) ) ;
#11489 = EDGE_LOOP ( 'NONE', ( #1173, #41014, #22017, #11897 ) ) ;
#11490 = DIRECTION ( 'NONE',  ( -0.9027978299657477557, 0.000000000000000000, 0.4300652022765115712 ) ) ;
#11491 = CARTESIAN_POINT ( 'NONE',  ( -47.78257572244586271, -189.7472609257535510, 0.7175072570443418174 ) ) ;
#11492 = FACE_BOUND ( 'NONE', #31889, .T. ) ;
#11493 = VERTEX_POINT ( 'NONE', #13362 ) ;
#11494 = AXIS2_PLACEMENT_3D ( 'NONE', #41637, #28765, #33242 ) ;
#11495 = AXIS2_PLACEMENT_3D ( 'NONE', #39748, #3765, #19794 ) ;
#11496 = CARTESIAN_POINT ( 'NONE',  ( -47.78257572244585560, -183.6283474603465606, -0.7175072570443230546 ) ) ;
#11497 = VECTOR ( 'NONE', #45679, 1000.000000000000000 ) ;
#11498 = VECTOR ( 'NONE', #12119, 1000.000000000000000 ) ;
#11499 = DIRECTION ( 'NONE',  ( -1.000000000000000000, 0.000000000000000000, 0.000000000000000000 ) ) ;
#11500 = VERTEX_POINT ( 'NONE', #48598 ) ;
#11501 = DIRECTION ( 'NONE',  ( 0.000000000000000000, -0.7485107481711069655, -0.6631226582407885317 ) ) ;
#11502 =( GEOMETRIC_REPRESENTATION_CONTEXT ( 3 ) GLOBAL_UNCERTAINTY_ASSIGNED_CONTEXT ( ( #18520 ) ) GLOBAL_UNIT_ASSIGNED_CONTEXT ( ( #27883, #43922, #7914 ) ) REPRESENTATION_CONTEXT ( 'NONE', 'WORKASPACE' ) );
#11503 = ORIENTED_EDGE ( 'NONE', *, *, #3518, .T. ) ;
#11504 = EDGE_CURVE ( 'NONE', #45084, #46184, #36222, .T. ) ;
#11505 = AXIS2_PLACEMENT_3D ( 'NONE', #18406, #18908, #6313 ) ;
#11506 = DIRECTION ( 'NONE',  ( 0.000000000000000000, 1.000000000000000000, -0.000000000000000000 ) ) ;
#11507 = FACE_BOUND ( 'NONE', #9380, .T. ) ;
#11508 = CARTESIAN_POINT ( 'NONE',  ( -156.2577088867455473, -193.5000000000000000, -63.31490529818420754 ) ) ;
#11509 = CARTESIAN_POINT ( 'NONE',  ( -162.3451783319732442, -183.6283474603465606, 51.57055649762783389 ) ) ;
#11510 = ORIENTED_EDGE ( 'NONE', *, *, #4013, .T. ) ;
#11511 = ORIENTED_EDGE ( 'NONE', *, *, #50246, .F. ) ;
#11512 = EDGE_CURVE ( 'NONE', #45026, #51761, #29376, .T. ) ;
#11513 = CARTESIAN_POINT ( 'NONE',  ( 0.000000000000000000, 20.00000000000000355, 0.000000000000000000 ) ) ;
#11514 = VECTOR ( 'NONE', #36689, 1000.000000000000000 ) ;
#11515 = AXIS2_PLACEMENT_3D ( 'NONE', #31018, #38392, #6853 ) ;
#11516 = ORIENTED_EDGE ( 'NONE', *, *, #45011, .F. ) ;
#11517 = CARTESIAN_POINT ( 'NONE',  ( -339.1964088526558498, -175.9742670995615015, -26.97593913775538965 ) ) ;
#11518 = VECTOR ( 'NONE', #42797, 1000.000000000000000 ) ;
#11519 = EDGE_CURVE ( 'NONE', #48694, #29891, #47722, .T. ) ;
#11520 = EDGE_CURVE ( 'NONE', #14560, #36987, #4091, .T. ) ;
#11521 = EDGE_CURVE ( 'NONE', #4209, #17851, #42689, .T. ) ;
#11522 = ADVANCED_FACE ( 'NONE', ( #12307 ), #8890, .T. ) ;
#11523 = ADVANCED_FACE ( 'NONE', ( #49109 ), #17314, .F. ) ;
#11524 = LINE ( 'NONE', #50974, #37356 ) ;
#11525 = ORIENTED_EDGE ( 'NONE', *, *, #22467, .F. ) ;
#11528 = ORIENTED_EDGE ( 'NONE', *, *, #34594, .F. ) ;
#11527 = DIRECTION ( 'NONE',  ( -0.000000000000000000, 0.6631226582408039638, 0.7485107481710934207 ) ) ;
#11526 = LINE ( 'NONE', #15754, #23341 ) ;
#11529 = VECTOR ( 'NONE', #49809, 1000.000000000000000 ) ;
#11530 = VECTOR ( 'NONE', #47614, 1000.000000000000000 ) ;
#11531 = EDGE_CURVE ( 'NONE', #39155, #47506, #36473, .T. ) ;
#11532 = ADVANCED_FACE ( 'NONE', ( #5228 ), #13095, .T. ) ;
#11533 = VECTOR ( 'NONE', #6520, 1000.000000000000000 ) ;
#11534 = DIRECTION ( 'NONE',  ( 0.000000000000000000, 0.000000000000000000, 1.000000000000000000 ) ) ;
#11535 = ORIENTED_EDGE ( 'NONE', *, *, #19546, .F. ) ;
#11536 = DIRECTION ( 'NONE',  ( -8.718379230999705894E-17, 0.9927088740980535286, -0.1205366802553268502 ) ) ;
#11537 = EDGE_LOOP ( 'NONE', ( #25145, #40901, #37512, #20649 ) ) ;
#11538 = AXIS2_PLACEMENT_3D ( 'NONE', #44912, #4704, #44123 ) ;
#11539 = LINE ( 'NONE', #43343, #18353 ) ;
#11540 = ORIENTED_EDGE ( 'NONE', *, *, #29236, .T. ) ;
#11541 = EDGE_CURVE ( 'NONE', #30974, #40458, #24160, .T. ) ;
#11543 = LINE ( 'NONE', #7088, #42590 ) ;
#11542 = DIRECTION ( 'NONE',  ( 0.000000000000000000, 0.000000000000000000, 1.000000000000000000 ) ) ;
#11544 = EDGE_LOOP ( 'NONE', ( #25167, #37668, #34303, #658 ) ) ;
#11545 = ADVANCED_FACE ( 'NONE', ( #40168 ), #48324, .T. ) ;
#11546 = VECTOR ( 'NONE', #40215, 1000.000000000000000 ) ;
#11547 = DIRECTION ( 'NONE',  ( 0.000000000000000000, -0.8229838658936613482, -0.5680647467311485954 ) ) ;
#11548 = ORIENTED_EDGE ( 'NONE', *, *, #36200, .F. ) ;
#11549 = PLANE ( 'NONE',  #16156 ) ;
#11550 = DIRECTION ( 'NONE',  ( 0.000000000000000000, 0.000000000000000000, 1.000000000000000000 ) ) ;
#11551 = EDGE_CURVE ( 'NONE', #1671, #37031, #48854, .T. ) ;
#11552 = DIRECTION ( 'NONE',  ( 0.000000000000000000, 1.000000000000000000, 0.000000000000000000 ) ) ;
#11553 = LINE ( 'NONE', #27580, #35889 ) ;
#11554 = CARTESIAN_POINT ( 'NONE',  ( -339.1964088526558498, -130.1153096980144426, 58.63009191191295599 ) ) ;
#11555 = DIRECTION ( 'NONE',  ( 0.9151456172430210145, 0.000000000000000000, -0.4031234292879665171 ) ) ;
#11556 = EDGE_CURVE ( 'NONE', #38180, #11142, #33336, .T. ) ;
#11557 = EDGE_LOOP ( 'NONE', ( #38833, #5985, #35412, #12380, #28614, #11443 ) ) ;
#11558 = DIRECTION ( 'NONE',  ( 1.000000000000000000, 0.000000000000000000, 0.000000000000000000 ) ) ;
#11559 = CARTESIAN_POINT ( 'NONE',  ( -170.0000000000000284, -113.5000000000000000, -40.00000000000001421 ) ) ;
#11560 = DIRECTION ( 'NONE',  ( 0.000000000000000000, 0.000000000000000000, 1.000000000000000000 ) ) ;
#11561 = EDGE_CURVE ( 'NONE', #41080, #1671, #41829, .T. ) ;
#11562 = CARTESIAN_POINT ( 'NONE',  ( -330.4913330509368166, -143.9541802141664562, 55.34326076196094135 ) ) ;
#11563 = ORIENTED_EDGE ( 'NONE', *, *, #32035, .T. ) ;
#11564 = CIRCLE ( 'NONE', #44281, 125.0000000000000000 ) ;
#11565 = VECTOR ( 'NONE', #47038, 1000.000000000000000 ) ;
#11566 = CARTESIAN_POINT ( 'NONE',  ( -339.1964088526558498, -89.57268800991514013, -48.27201571436026484 ) ) ;
#11567 = DIRECTION ( 'NONE',  ( -0.000000000000000000, -1.000000000000000000, 0.000000000000000000 ) ) ;
#11568 = CIRCLE ( 'NONE', #35086, 125.0000000000000000 ) ;
#11569 = PLANE ( 'NONE',  #32811 ) ;
#11571 = ORIENTED_EDGE ( 'NONE', *, *, #311, .F. ) ;
#11570 = LINE ( 'NONE', #8143, #19074 ) ;
#11572 = EDGE_LOOP ( 'NONE', ( #35040, #7139, #17604, #48088 ) ) ;
#11573 = ORIENTED_EDGE ( 'NONE', *, *, #20922, .F. ) ;
#11574 = EDGE_CURVE ( 'NONE', #21936, #46797, #754, .T. ) ;
#11575 = VECTOR ( 'NONE', #6172, 1000.000000000000114 ) ;
#11576 = CARTESIAN_POINT ( 'NONE',  ( -339.1964088526558498, -123.5000000000000284, 0.000000000000000000 ) ) ;
#11577 = CARTESIAN_POINT ( 'NONE',  ( 75.52097166332623601, -177.1207230881787780, -0.3215015308241039316 ) ) ;
#11578 = DIRECTION ( 'NONE',  ( 1.000000000000000000, 0.000000000000000000, 0.000000000000000000 ) ) ;
#11579 = CARTESIAN_POINT ( 'NONE',  ( -64.08700758308647494, -189.7472609257535510, -124.0217483183786840 ) ) ;
#11580 = ORIENTED_EDGE ( 'NONE', *, *, #23885, .T. ) ;
#11581 = CARTESIAN_POINT ( 'NONE',  ( 1.734723475976807094E-15, 20.00000000000000000, 46.00000000000000711 ) ) ;
#11582 = AXIS2_PLACEMENT_3D ( 'NONE', #8105, #24149, #44381 ) ;
#11583 = EDGE_LOOP ( 'NONE', ( #24303, #20601, #30929, #32213 ) ) ;
#11584 = ORIENTED_EDGE ( 'NONE', *, *, #23974, .T. ) ;
#11585 = ORIENTED_EDGE ( 'NONE', *, *, #9246, .F. ) ;
#11586 = CARTESIAN_POINT ( 'NONE',  ( -102.5006284722404502, -177.1207230881787780, -112.7238987608084386 ) ) ;
#11587 = EDGE_CURVE ( 'NONE', #50750, #4539, #10798, .T. ) ;
#11588 = EDGE_CURVE ( 'NONE', #41523, #41127, #49375, .T. ) ;
#11589 = DIRECTION ( 'NONE',  ( 0.000000000000000000, -1.000000000000000000, -0.000000000000000000 ) ) ;
#11590 = EDGE_LOOP ( 'NONE', ( #17710, #10427, #18377, #22184 ) ) ;
#11591 = DIRECTION ( 'NONE',  ( -0.000000000000000000, 0.000000000000000000, 1.000000000000000000 ) ) ;
#11592 = DIRECTION ( 'NONE',  ( 0.000000000000000000, 0.5680647467311510379, -0.8229838658936596829 ) ) ;
#11593 = VECTOR ( 'NONE', #8188, 1000.000000000000000 ) ;
#11596 = ORIENTED_EDGE ( 'NONE', *, *, #34978, .F. ) ;
#11595 = DIRECTION ( 'NONE',  ( 0.000000000000000000, -1.000000000000000000, -0.000000000000000000 ) ) ;
#11594 = FACE_OUTER_BOUND ( 'NONE', #1911, .T. ) ;
#11597 = AXIS2_PLACEMENT_3D ( 'NONE', #8321, #4909, #16470 ) ;
#11598 = AXIS2_PLACEMENT_3D ( 'NONE', #42870, #7131, #10556 ) ;
#11599 = CARTESIAN_POINT ( 'NONE',  ( -84.82349129030157542, -189.7472609257535510, -119.5996955107802364 ) ) ;
#11600 = VERTEX_POINT ( 'NONE', #45181 ) ;
#11601 = LINE ( 'NONE', #48383, #10471 ) ;
#11602 = AXIS2_PLACEMENT_3D ( 'NONE', #7642, #7890, #23425 ) ;
#11603 = EDGE_LOOP ( 'NONE', ( #5274, #37699, #12409, #36095 ) ) ;
#11604 = LINE ( 'NONE', #35502, #37497 ) ;
#11605 = CARTESIAN_POINT ( 'NONE',  ( -336.3521761649654422, -146.8829211657874794, -54.23253582808848705 ) ) ;
#11607 = DIRECTION ( 'NONE',  ( -0.000000000000000000, -0.6631226582407911962, 0.7485107481711046340 ) ) ;
#11606 = LINE ( 'NONE', #7907, #27448 ) ;
#11608 = VERTEX_POINT ( 'NONE', #37269 ) ;
#11609 = VECTOR ( 'NONE', #18640, 1000.000000000000114 ) ;
#11610 = CARTESIAN_POINT ( 'NONE',  ( -124.3803110981236273, -193.5000000000000000, -98.05618656931939370 ) ) ;
#11611 = CARTESIAN_POINT ( 'NONE',  ( -332.3517673607765914, -64.15626348514393840, -8.849911663702497933 ) ) ;
#11612 = CARTESIAN_POINT ( 'NONE',  ( 47.04848625005566731, -177.1207230881787780, 80.61932246194658092 ) ) ;
#11613 = VERTEX_POINT ( 'NONE', #1261 ) ;
#11614 = EDGE_CURVE ( 'NONE', #42344, #14242, #45222, .T. ) ;
#11615 = LINE ( 'NONE', #42642, #36674 ) ;
#11616 = DIRECTION ( 'NONE',  ( 1.000000000000000000, 0.000000000000000000, -0.000000000000000000 ) ) ;
#11617 = DIRECTION ( 'NONE',  ( 0.000000000000000000, -0.000000000000000000, 1.000000000000000000 ) ) ;
#11618 = ORIENTED_EDGE ( 'NONE', *, *, #23709, .F. ) ;
#11619 = DIRECTION ( 'NONE',  ( -0.000000000000000000, 1.000000000000000000, -0.000000000000000000 ) ) ;
#11620 = DIRECTION ( 'NONE',  ( 0.2348860457809842095, 0.000000000000000000, -0.9720229140804107493 ) ) ;
#11621 = EDGE_CURVE ( 'NONE', #23503, #31214, #29251, .T. ) ;
#11622 = VECTOR ( 'NONE', #13941, 1000.000000000000000 ) ;
#11623 = CARTESIAN_POINT ( 'NONE',  ( -137.2624501260119985, -183.6283474603465606, 87.99159897727967916 ) ) ;
#11624 = ORIENTED_EDGE ( 'NONE', *, *, #40962, .T. ) ;
#11625 = FACE_OUTER_BOUND ( 'NONE', #30638, .T. ) ;
#11626 = VERTEX_POINT ( 'NONE', #21505 ) ;
#11627 = CARTESIAN_POINT ( 'NONE',  ( -332.3517673607765914, -82.50558083279611310, 43.81161486573607533 ) ) ;
#11628 = CARTESIAN_POINT ( 'NONE',  ( 62.59443091842029361, -177.1207230881787780, -57.33816169485141501 ) ) ;
#11629 = LINE ( 'NONE', #23465, #41138 ) ;
#11630 = CARTESIAN_POINT ( 'NONE',  ( -339.1964088526558498, -89.82879061784626629, 49.66134974749640207 ) ) ;
#11631 = LINE ( 'NONE', #27659, #25750 ) ;
#11632 = CARTESIAN_POINT ( 'NONE',  ( 9.336583202542586335, -189.7472609257535510, 110.8257356506556164 ) ) ;
#11633 = AXIS2_PLACEMENT_3D ( 'NONE', #29511, #9551, #45051 ) ;
#11634 = AXIS2_PLACEMENT_3D ( 'NONE', #44888, #742, #5739 ) ;
#11635 = DIRECTION ( 'NONE',  ( 0.000000000000000000, -0.9350162426854169428, -0.3546048870425300148 ) ) ;
#11636 = DIRECTION ( 'NONE',  ( 0.000000000000000000, 0.000000000000000000, 1.000000000000000000 ) ) ;
#11638 = EDGE_LOOP ( 'NONE', ( #27597, #630 ) ) ;
#11637 = DIRECTION ( 'NONE',  ( -0.000000000000000000, 1.000000000000000000, -0.000000000000000000 ) ) ;
#11639 = SHAPE_REPRESENTATION ( 'Tool Retaining Set Screws', ( #31742 ), #22569 ) ;
#11640 = AXIS2_PLACEMENT_3D ( 'NONE', #39874, #47284, #15748 ) ;
#11641 = VERTEX_POINT ( 'NONE', #14652 ) ;
#11642 = CARTESIAN_POINT ( 'NONE',  ( 73.09196206113300320, -177.1207230881787780, 29.07697310430963356 ) ) ;
#11643 = LINE ( 'NONE', #4272, #35490 ) ;
#11644 = ORIENTED_EDGE ( 'NONE', *, *, #28632, .T. ) ;
#11645 = AXIS2_PLACEMENT_3D ( 'NONE', #51424, #18325, #34584 ) ;
#11646 = VERTEX_POINT ( 'NONE', #13612 ) ;
#11647 = DIRECTION ( 'NONE',  ( -0.000000000000000000, 1.000000000000000000, -0.000000000000000000 ) ) ;
#11648 = ORIENTED_EDGE ( 'NONE', *, *, #41508, .F. ) ;
#11649 = CARTESIAN_POINT ( 'NONE',  ( 52.16997862029128186, -175.3837268820161057, 72.42760398749086903 ) ) ;
#11650 = PLANE ( 'NONE',  #17484 ) ;
#11651 = EDGE_CURVE ( 'NONE', #12334, #38856, #41461, .T. ) ;
#11652 = LINE ( 'NONE', #41569, #18574 ) ;
#11653 = FACE_OUTER_BOUND ( 'NONE', #9632, .T. ) ;
#11654 = VERTEX_POINT ( 'NONE', #45428 ) ;
#11655 = ORIENTED_EDGE ( 'NONE', *, *, #28834, .T. ) ;
#11656 = ORIENTED_EDGE ( 'NONE', *, *, #4819, .T. ) ;
#11657 = CIRCLE ( 'NONE', #41029, 10.00000000000000711 ) ;
#11658 = PLANE ( 'NONE',  #24980 ) ;
#11659 = DIRECTION ( 'NONE',  ( -0.000000000000000000, 1.000000000000000000, -0.000000000000000000 ) ) ;
#11660 = PLANE ( 'NONE',  #19502 ) ;
#11661 = CARTESIAN_POINT ( 'NONE',  ( -172.0602536473422504, -189.7472609257535510, -10.18383939837523222 ) ) ;
#11662 = EDGE_LOOP ( 'NONE', ( #13520, #33773, #42104, #12040 ) ) ;
#11663 = DIRECTION ( 'NONE',  ( -0.000000000000000000, -0.9709418174260511236, 0.2393156642875615969 ) ) ;
#11664 = LINE ( 'NONE', #343, #1308 ) ;
#11665 = CARTESIAN_POINT ( 'NONE',  ( -305.0000000000000568, -166.6218737817864621, 41.71934804797023588 ) ) ;
#11666 = ORIENTED_EDGE ( 'NONE', *, *, #38071, .T. ) ;
#11667 = ORIENTED_EDGE ( 'NONE', *, *, #24509, .F. ) ;
#11668 = VERTEX_POINT ( 'NONE', #45956 ) ;
#11669 = DIRECTION ( 'NONE',  ( -0.000000000000000000, 1.000000000000000000, -0.000000000000000000 ) ) ;
#11671 = CIRCLE ( 'NONE', #49477, 4.999999999999997335 ) ;
#11670 = LINE ( 'NONE', #48200, #16606 ) ;
#11672 = VERTEX_POINT ( 'NONE', #5992 ) ;
#11673 = ADVANCED_FACE ( 'NONE', ( #2564 ), #25447, .T. ) ;
#11674 = CARTESIAN_POINT ( 'NONE',  ( -332.3517673607765914, -121.8677111499054320, 59.97779283292990016 ) ) ;
#11675 = AXIS2_PLACEMENT_3D ( 'NONE', #14132, #18825, #14638 ) ;
#11676 = LINE ( 'NONE', #51623, #10280 ) ;
#11677 = DIRECTION ( 'NONE',  ( 0.000000000000000000, 0.000000000000000000, 1.000000000000000000 ) ) ;
#11678 = EDGE_LOOP ( 'NONE', ( #4255, #31241, #37597, #826 ) ) ;
#11679 = PLANE ( 'NONE',  #25892 ) ;
#11680 = EDGE_LOOP ( 'NONE', ( #29426, #10637, #40109, #33762 ) ) ;
#11681 = CARTESIAN_POINT ( 'NONE',  ( -48.98765787015805984, -183.6283474603465606, -0.8610436117673551104 ) ) ;
#11682 = AXIS2_PLACEMENT_3D ( 'NONE', #28311, #8352, #45399 ) ;
#11683 = LINE ( 'NONE', #51387, #40444 ) ;
#11684 = ORIENTED_EDGE ( 'NONE', *, *, #28090, .T. ) ;
#11685 = DIRECTION ( 'NONE',  ( 0.5586467658036476935, 0.000000000000000000, 0.8294056854502049880 ) ) ;
#11686 = CARTESIAN_POINT ( 'NONE',  ( -332.3517673607765914, -176.9651911376907094, -25.08789112700655721 ) ) ;
#11687 = PLANE ( 'NONE',  #44144 ) ;
#11688 = FACE_OUTER_BOUND ( 'NONE', #32652, .T. ) ;
#11689 = VECTOR ( 'NONE', #47423, 1000.000000000000000 ) ;
#11690 = ORIENTED_EDGE ( 'NONE', *, *, #49794, .T. ) ;
#11691 = PLANE ( 'NONE',  #4331 ) ;
#11692 = ORIENTED_EDGE ( 'NONE', *, *, #10578, .T. ) ;
#11693 = ORIENTED_EDGE ( 'NONE', *, *, #42798, .F. ) ;
#11695 = EDGE_LOOP ( 'NONE', ( #20421, #35302, #32408, #15975 ) ) ;
#11694 = LINE ( 'NONE', #43751, #34537 ) ;
#11696 = EDGE_CURVE ( 'NONE', #47995, #20677, #33842, .T. ) ;
#11697 = ORIENTED_EDGE ( 'NONE', *, *, #1794, .T. ) ;
#11698 = FACE_OUTER_BOUND ( 'NONE', #18303, .T. ) ;
#11699 = ADVANCED_FACE ( 'NONE', ( #9943 ), #22014, .T. ) ;
#11700 = DIRECTION ( 'NONE',  ( -1.000000000000000000, 0.000000000000000000, -0.000000000000000000 ) ) ;
#11701 = ORIENTED_EDGE ( 'NONE', *, *, #43053, .F. ) ;
#11702 = AXIS2_PLACEMENT_3D ( 'NONE', #20624, #36658, #28751 ) ;
#11703 = DIRECTION ( 'NONE',  ( 0.000000000000000000, 0.000000000000000000, 1.000000000000000000 ) ) ;
#11704 = LINE ( 'NONE', #29226, #23658 ) ;
#11705 = EDGE_LOOP ( 'NONE', ( #33753, #1597, #24908, #37722 ) ) ;
#11706 = CARTESIAN_POINT ( 'NONE',  ( 72.71365293123227502, -193.5000000000000000, -30.61552143554913030 ) ) ;
#11707 = CARTESIAN_POINT ( 'NONE',  ( -63.09433862318514485, -189.7472609257535510, -124.1426420773539547 ) ) ;
#11708 = AXIS2_PLACEMENT_3D ( 'NONE', #39189, #47343, #18453 ) ;
#11709 = EDGE_CURVE ( 'NONE', #12667, #15472, #50658, .T. ) ;
#11710 = CARTESIAN_POINT ( 'NONE',  ( 48.69345348225014902, -193.5000000000000000, -78.62880929222872339 ) ) ;
#11711 = DIRECTION ( 'NONE',  ( 0.7765238627180482966, 0.000000000000000000, -0.6300878435817038881 ) ) ;
#11712 = EDGE_LOOP ( 'NONE', ( #40945, #3463, #35648, #26863 ) ) ;
#11713 = VERTEX_POINT ( 'NONE', #2315 ) ;
#11714 = EDGE_CURVE ( 'NONE', #41052, #28664, #38519, .T. ) ;
#11715 = ORIENTED_EDGE ( 'NONE', *, *, #14572, .F. ) ;
#11716 = DIRECTION ( 'NONE',  ( 0.000000000000000000, -1.000000000000000000, 0.000000000000000000 ) ) ;
#11717 = CARTESIAN_POINT ( 'NONE',  ( 14.37129481273059106, -189.7472609257535510, -108.0501018472328241 ) ) ;
#11718 = EDGE_CURVE ( 'NONE', #23787, #39696, #18349, .T. ) ;
#11719 = CARTESIAN_POINT ( 'NONE',  ( 73.09196206113300320, -193.5000000000000000, 29.07697310430963356 ) ) ;
#11720 = CYLINDRICAL_SURFACE ( 'NONE', #2660, 125.0000000000000000 ) ;
#11721 = DIRECTION ( 'NONE',  ( 0.000000000000000000, -0.000000000000000000, 1.000000000000000000 ) ) ;
#11722 = EDGE_LOOP ( 'NONE', ( #26985, #30872, #14721, #4242 ) ) ;
#11723 = AXIS2_PLACEMENT_3D ( 'NONE', #21482, #13068, #29095 ) ;
#11724 = CARTESIAN_POINT ( 'NONE',  ( 10.22625775207003507, -183.6283474603465606, -109.2239789693433352 ) ) ;
#11725 = ORIENTED_EDGE ( 'NONE', *, *, #5972, .F. ) ;
#11727 = EDGE_LOOP ( 'NONE', ( #48651, #27922, #28704, #10580 ) ) ;
#11726 = PLANE ( 'NONE',  #38203 ) ;
#11728 = ORIENTED_EDGE ( 'NONE', *, *, #19726, .T. ) ;
#11729 = CARTESIAN_POINT ( 'NONE',  ( -46.00000000000000711, 20.00000000000000000, 46.00000000000000000 ) ) ;
#11730 = EDGE_CURVE ( 'NONE', #51354, #10952, #38036, .T. ) ;
#11731 = DIRECTION ( 'NONE',  ( -8.718379230999705894E-17, 0.2393156642875582940, 0.9709418174260519008 ) ) ;
#11732 = CARTESIAN_POINT ( 'NONE',  ( -140.8230258362169707, -189.7472609257535510, 84.24728067916045404 ) ) ;
#11733 = DIRECTION ( 'NONE',  ( -0.000000000000000000, 1.000000000000000000, -0.000000000000000000 ) ) ;
#11734 = VERTEX_POINT ( 'NONE', #18594 ) ;
#11735 = DIRECTION ( 'NONE',  ( 0.000000000000000000, -1.000000000000000000, -0.000000000000000000 ) ) ;
#11736 = VERTEX_POINT ( 'NONE', #50156 ) ;
#11737 = ORIENTED_EDGE ( 'NONE', *, *, #17724, .F. ) ;
#11738 = LINE ( 'NONE', #44058, #41347 ) ;
#11739 = AXIS2_PLACEMENT_3D ( 'NONE', #18442, #34457, #50505 ) ;
#11740 = PLANE ( 'NONE',  #24884 ) ;
#11741 = DIRECTION ( 'NONE',  ( -1.000000000000000000, 0.000000000000000000, 0.000000000000000000 ) ) ;
#11742 = CARTESIAN_POINT ( 'NONE',  ( 46.00000000000000711, 20.00000000000000000, 46.00000000000000000 ) ) ;
#11743 = CARTESIAN_POINT ( 'NONE',  ( -336.3521761649654422, -146.8829211657874794, -54.23253582808848705 ) ) ;
#11744 = EDGE_LOOP ( 'NONE', ( #12567, #9037, #979, #2371 ) ) ;
#11745 = CARTESIAN_POINT ( 'NONE',  ( -87.88805327685028601, -177.1207230881787780, 117.5715283571807106 ) ) ;
#11746 = DIRECTION ( 'NONE',  ( 0.000000000000000000, 1.000000000000000000, 0.000000000000000000 ) ) ;
#11747 = FACE_BOUND ( 'NONE', #46562, .T. ) ;
#11748 = ORIENTED_EDGE ( 'NONE', *, *, #41081, .T. ) ;
#11749 = CARTESIAN_POINT ( 'NONE',  ( -95.72791768350677444, -183.6283474603465606, -115.7261930397105516 ) ) ;
#11750 = DIRECTION ( 'NONE',  ( -0.000000000000000000, -0.6631226582407885317, 0.7485107481711069655 ) ) ;
#11751 = EDGE_CURVE ( 'NONE', #14590, #33364, #39338, .T. ) ;
#11752 = ORIENTED_EDGE ( 'NONE', *, *, #21576, .T. ) ;
#11753 = ADVANCED_FACE ( 'NONE', ( #18078 ), #14150, .F. ) ;
#11754 = DIRECTION ( 'NONE',  ( -0.9890401873221623674, 0.000000000000000000, -0.1476465640024917925 ) ) ;
#11755 = ORIENTED_EDGE ( 'NONE', *, *, #24086, .T. ) ;
#11756 = VECTOR ( 'NONE', #7470, 1000.000000000000000 ) ;
#11757 = CIRCLE ( 'NONE', #18492, 125.0000000000000000 ) ;
#11758 = FACE_OUTER_BOUND ( 'NONE', #20580, .T. ) ;
#11759 = FACE_BOUND ( 'NONE', #21814, .T. ) ;
#11761 = ORIENTED_EDGE ( 'NONE', *, *, #40119, .T. ) ;
#11760 = DIRECTION ( 'NONE',  ( 1.000000000000000000, 6.525800561034949817E-17, -5.781354811211897260E-17 ) ) ;
#11762 = EDGE_CURVE ( 'NONE', #28114, #17942, #26465, .T. ) ;
#11763 = CARTESIAN_POINT ( 'NONE',  ( -336.3521761649654422, -176.9651911376907094, -25.08789112700655721 ) ) ;
#11764 = VERTEX_POINT ( 'NONE', #10186 ) ;
#11765 = EDGE_CURVE ( 'NONE', #10187, #20971, #17576, .T. ) ;
#11766 = ORIENTED_EDGE ( 'NONE', *, *, #39576, .F. ) ;
#11767 = DIRECTION ( 'NONE',  ( 0.000000000000000000, 0.000000000000000000, -1.000000000000000000 ) ) ;
#11768 = EDGE_CURVE ( 'NONE', #43264, #3693, #6522, .T. ) ;
#11769 = VECTOR ( 'NONE', #48829, 1000.000000000000000 ) ;
#11770 = ORIENTED_EDGE ( 'NONE', *, *, #7084, .F. ) ;
#11771 = FACE_OUTER_BOUND ( 'NONE', #33769, .T. ) ;
#11772 = DIRECTION ( 'NONE',  ( -0.000000000000000000, -0.4647231720437724478, -0.8854560256532078011 ) ) ;
#11773 = EDGE_CURVE ( 'NONE', #6751, #3432, #38564, .T. ) ;
#11774 = CARTESIAN_POINT ( 'NONE',  ( 51.70113075622899856, 30.00000000000000355, -45.78969942005421956 ) ) ;
#11775 = VERTEX_POINT ( 'NONE', #35645 ) ;
#11778 = VERTEX_POINT ( 'NONE', #23822 ) ;
#11777 = CARTESIAN_POINT ( 'NONE',  ( -11.80936624585915418, -175.3837268820161057, -119.5003291395395735 ) ) ;
#11776 = CARTESIAN_POINT ( 'NONE',  ( 60.02977459919873837, -175.3837268820161057, 60.01515274641010222 ) ) ;
#11779 = ORIENTED_EDGE ( 'NONE', *, *, #25017, .T. ) ;
#11780 = LINE ( 'NONE', #15226, #42417 ) ;
#11781 = ORIENTED_EDGE ( 'NONE', *, *, #10383, .T. ) ;
#11782 = DIRECTION ( 'NONE',  ( 0.000000000000000000, 0.1205366802553268363, 0.9927088740980534176 ) ) ;
#11783 = ORIENTED_EDGE ( 'NONE', *, *, #18126, .F. ) ;
#11784 = CARTESIAN_POINT ( 'NONE',  ( 64.29733702426837283, -175.3837268820161057, 53.91167979418564471 ) ) ;
#11785 = ORIENTED_EDGE ( 'NONE', *, *, #28260, .T. ) ;
#11787 = LINE ( 'NONE', #477, #27502 ) ;
#11786 = CARTESIAN_POINT ( 'NONE',  ( -48.47912675150885065, -189.7472609257535510, 6.938893903907228378E-15 ) ) ;
#11788 = ORIENTED_EDGE ( 'NONE', *, *, #5697, .F. ) ;
#11789 = AXIS2_PLACEMENT_3D ( 'NONE', #38921, #51047, #3697 ) ;
#11790 = AXIS2_PLACEMENT_3D ( 'NONE', #40697, #41224, #33360 ) ;
#11791 = DIRECTION ( 'NONE',  ( 0.000000000000000000, -1.000000000000000000, -0.000000000000000000 ) ) ;
#11792 = VERTEX_POINT ( 'NONE', #18843 ) ;
#11793 = PLANE ( 'NONE',  #48878 ) ;
#11794 = CARTESIAN_POINT ( 'NONE',  ( -47.70260288879081401, -189.7472609257535510, 0.6300878435817218737 ) ) ;
#11795 = DIRECTION ( 'NONE',  ( 0.000000000000000000, 0.000000000000000000, 1.000000000000000000 ) ) ;
#11796 = DIRECTION ( 'NONE',  ( 0.000000000000000000, 0.000000000000000000, -1.000000000000000000 ) ) ;
#11797 = DIRECTION ( 'NONE',  ( 0.000000000000000000, 0.000000000000000000, -1.000000000000000000 ) ) ;
#11798 = FACE_OUTER_BOUND ( 'NONE', #6545, .T. ) ;
#11799 = EDGE_LOOP ( 'NONE', ( #20755, #28912, #49451, #31665 ) ) ;
#11800 = DIRECTION ( 'NONE',  ( 0.000000000000000000, -0.000000000000000000, 1.000000000000000000 ) ) ;
#11801 = CARTESIAN_POINT ( 'NONE',  ( -339.1964088526558498, -130.1153096980144426, 58.63009191191295599 ) ) ;
#11802 = EDGE_CURVE ( 'NONE', #41880, #13092, #23564, .T. ) ;
#11803 = DIRECTION ( 'NONE',  ( 0.000000000000000000, -1.000000000000000000, 0.000000000000000000 ) ) ;
#11804 = EDGE_LOOP ( 'NONE', ( #8049, #1182, #16860, #29598 ) ) ;
#11805 = AXIS2_PLACEMENT_3D ( 'NONE', #25608, #17743, #6175 ) ;
#11806 = LINE ( 'NONE', #52040, #48340 ) ;
#11807 = ADVANCED_FACE ( 'NONE', ( #51967 ), #6773, .T. ) ;
#11808 = DIRECTION ( 'NONE',  ( 1.000000000000000000, -0.000000000000000000, -0.000000000000000000 ) ) ;
#11809 = CARTESIAN_POINT ( 'NONE',  ( -336.3521761649653854, -146.2946350401741711, -55.50139289590185854 ) ) ;
#11810 = EDGE_CURVE ( 'NONE', #32088, #26105, #34862, .T. ) ;
#11811 = ORIENTED_EDGE ( 'NONE', *, *, #31586, .T. ) ;
#11812 = EDGE_CURVE ( 'NONE', #18768, #29891, #31714, .T. ) ;
#11813 = VERTEX_POINT ( 'NONE', #3337 ) ;
#11814 = VERTEX_POINT ( 'NONE', #15700 ) ;
#11815 = ADVANCED_FACE ( 'NONE', ( #46981 ), #14926, .F. ) ;
#11816 = DIRECTION ( 'NONE',  ( -0.000000000000000000, 1.000000000000000000, -0.000000000000000000 ) ) ;
#11817 = ADVANCED_FACE ( 'NONE', ( #22794 ), #47758, .F. ) ;
#11818 = CARTESIAN_POINT ( 'NONE',  ( 46.00000000000000000, 0.000000000000000000, 0.000000000000000000 ) ) ;
#11819 = CARTESIAN_POINT ( 'NONE',  ( -104.8182102393454045, -189.7472609257535510, 111.5836353223472912 ) ) ;
#11820 = CARTESIAN_POINT ( 'NONE',  ( 24.15597040328004752, -177.1207230881787780, -101.7307360698543874 ) ) ;
#11821 = AXIS2_PLACEMENT_3D ( 'NONE', #26812, #40368, #8339 ) ;
#11822 = VERTEX_POINT ( 'NONE', #31443 ) ;
#11823 = EDGE_CURVE ( 'NONE', #28285, #28167, #26984, .T. ) ;
#11824 = CARTESIAN_POINT ( 'NONE',  ( 4.231823864385127365, 52.95470401233406932, -19.37596056129619981 ) ) ;
#11825 = EDGE_CURVE ( 'NONE', #32738, #49319, #43017, .T. ) ;
#11826 = CIRCLE ( 'NONE', #21905, 125.0000000000000000 ) ;
#11827 = ORIENTED_EDGE ( 'NONE', *, *, #19070, .T. ) ;
#11828 = VERTEX_POINT ( 'NONE', #3860 ) ;
#11829 = EDGE_CURVE ( 'NONE', #18286, #30079, #46941, .T. ) ;
#11830 = ORIENTED_EDGE ( 'NONE', *, *, #32291, .F. ) ;
#11831 = DIRECTION ( 'NONE',  ( -0.6965510290630033685, 0.000000000000000000, 0.7175072570443249420 ) ) ;
#11832 = EDGE_CURVE ( 'NONE', #37933, #23116, #39833, .T. ) ;
#11833 = ORIENTED_EDGE ( 'NONE', *, *, #30567, .F. ) ;
#11834 = EDGE_CURVE ( 'NONE', #4203, #37758, #19370, .T. ) ;
#11835 = ADVANCED_FACE ( 'NONE', ( #10707 ), #51695, .T. ) ;
#11836 = DIRECTION ( 'NONE',  ( -0.000000000000000000, 1.000000000000000000, -0.000000000000000000 ) ) ;
#11837 = FACE_OUTER_BOUND ( 'NONE', #4971, .T. ) ;
#11840 = EDGE_LOOP ( 'NONE', ( #8776, #9321, #7825, #22044 ) ) ;
#11839 = DIRECTION ( 'NONE',  ( -0.000000000000000000, 1.000000000000000000, -0.000000000000000000 ) ) ;
#11838 = CARTESIAN_POINT ( 'NONE',  ( 141.7825277784304205, -213.5000000000000000, -9.999999999999987566 ) ) ;
#11841 = AXIS2_PLACEMENT_3D ( 'NONE', #16648, #32655, #8733 ) ;
#11842 = DIRECTION ( 'NONE',  ( 0.000000000000000000, 0.000000000000000000, 1.000000000000000000 ) ) ;
#11843 = EDGE_LOOP ( 'NONE', ( #1006, #7772, #36955, #33585 ) ) ;
#11844 = CARTESIAN_POINT ( 'NONE',  ( -48.47912675150885065, -120.5000000000000284, -14.99999999999999289 ) ) ;
#11845 = ORIENTED_EDGE ( 'NONE', *, *, #45396, .F. ) ;
#11846 = DIRECTION ( 'NONE',  ( -0.000000000000000000, 1.000000000000000000, -0.000000000000000000 ) ) ;
#11847 = CARTESIAN_POINT ( 'NONE',  ( -332.3517673607765914, -64.31210272782786319, -9.838334030657643225 ) ) ;
#11849 = CARTESIAN_POINT ( 'NONE',  ( -15.24927435600542047, -183.6283474603465606, 120.5021863277719092 ) ) ;
#11848 = FACE_OUTER_BOUND ( 'NONE', #20271, .T. ) ;
#11850 = EDGE_CURVE ( 'NONE', #21083, #17362, #39577, .T. ) ;
#11851 = ORIENTED_EDGE ( 'NONE', *, *, #50939, .F. ) ;
#11852 = CARTESIAN_POINT ( 'NONE',  ( -81.47409310123204307, -183.6283474603465606, -119.5301634136912554 ) ) ;
#11853 = DIRECTION ( 'NONE',  ( 0.000000000000000000, 0.000000000000000000, 1.000000000000000000 ) ) ;
#11854 = ORIENTED_EDGE ( 'NONE', *, *, #42382, .T. ) ;
#11855 = CARTESIAN_POINT ( 'NONE',  ( -172.5669052183642123, -193.5000000000000000, 15.07392567185553567 ) ) ;
#11856 = DIRECTION ( 'NONE',  ( 1.000000000000000000, 0.000000000000000000, -0.000000000000000000 ) ) ;
#11857 = AXIS2_PLACEMENT_3D ( 'NONE', #42453, #6479, #22507 ) ;
#11858 = DIRECTION ( 'NONE',  ( -0.000000000000000000, 1.000000000000000000, 0.000000000000000000 ) ) ;
#11859 = VERTEX_POINT ( 'NONE', #51440 ) ;
#11860 = DIRECTION ( 'NONE',  ( 0.000000000000000000, 1.000000000000000000, -0.000000000000000000 ) ) ;
#11861 = AXIS2_PLACEMENT_3D ( 'NONE', #26410, #29841, #45892 ) ;
#11862 = CARTESIAN_POINT ( 'NONE',  ( -330.4913330509368166, -162.9984922102926532, -43.83057281297441676 ) ) ;
#11863 = CIRCLE ( 'NONE', #38690, 60.00000000000000000 ) ;
#11864 = EDGE_LOOP ( 'NONE', ( #7147, #3899, #5733, #13854 ) ) ;
#11865 = CARTESIAN_POINT ( 'NONE',  ( -336.3521761649654422, -92.15051119686104641, -50.05135858667769355 ) ) ;
#11866 = VERTEX_POINT ( 'NONE', #30661 ) ;
#11867 = PLANE ( 'NONE',  #33210 ) ;
#11868 = DIRECTION ( 'NONE',  ( 0.000000000000000000, 1.000000000000000000, -0.000000000000000000 ) ) ;
#11869 = ADVANCED_FACE ( 'NONE', ( #43544 ), #7543, .F. ) ;
#11870 = CARTESIAN_POINT ( 'NONE',  ( -48.82732838694323618, -193.5000000000000000, -0.9374196611341184537 ) ) ;
#11871 = CARTESIAN_POINT ( 'NONE',  ( -332.3517673607765914, -140.1754235130667610, -56.65561927338005432 ) ) ;
#11872 = DIRECTION ( 'NONE',  ( -0.000000000000000000, -0.9350162426854169428, -0.3546048870425300148 ) ) ;
#11873 = EDGE_CURVE ( 'NONE', #28415, #12983, #35137, .T. ) ;
#11874 = AXIS2_PLACEMENT_3D ( 'NONE', #4460, #48624, #28618 ) ;
#11875 = EDGE_CURVE ( 'NONE', #24196, #37502, #40348, .T. ) ;
#11876 = FACE_OUTER_BOUND ( 'NONE', #30073, .T. ) ;
#11877 = EDGE_CURVE ( 'NONE', #10455, #21654, #19210, .T. ) ;
#11878 = VECTOR ( 'NONE', #26188, 999.9999999999998863 ) ;
#11879 = LINE ( 'NONE', #35801, #12726 ) ;
#11880 = CARTESIAN_POINT ( 'NONE',  ( -339.1964088526558498, -131.1080185721133660, -58.50955523165751515 ) ) ;
#11882 = ORIENTED_EDGE ( 'NONE', *, *, #18590, .F. ) ;
#11881 = CARTESIAN_POINT ( 'NONE',  ( -107.6930423737362190, -177.1207230881787780, 110.0850225811110761 ) ) ;
#11883 = VERTEX_POINT ( 'NONE', #8056 ) ;
#11884 = DIRECTION ( 'NONE',  ( -0.000000000000000000, 1.000000000000000000, -0.000000000000000000 ) ) ;
#11885 = CARTESIAN_POINT ( 'NONE',  ( -127.4665351220365892, -193.5000000000000000, -96.88131563365291754 ) ) ;
#11886 = ORIENTED_EDGE ( 'NONE', *, *, #30191, .T. ) ;
#11887 = ORIENTED_EDGE ( 'NONE', *, *, #8949, .T. ) ;
#11888 = EDGE_CURVE ( 'NONE', #48776, #2708, #32220, .T. ) ;
#11889 = ORIENTED_EDGE ( 'NONE', *, *, #19193, .T. ) ;
#11890 = CARTESIAN_POINT ( 'NONE',  ( -336.3521761649654422, -65.24746378767824240, -9.724760635741734660 ) ) ;
#11891 = DIRECTION ( 'NONE',  ( 0.000000000000000000, 0.3546048870425363986, 0.9350162426854146114 ) ) ;
#11892 = VECTOR ( 'NONE', #28657, 1000.000000000000000 ) ;
#11893 = CARTESIAN_POINT ( 'NONE',  ( -171.9838957966129840, -189.7472609257535510, 19.27620354518724355 ) ) ;
#11894 = PLANE ( 'NONE',  #49299 ) ;
#11895 = AXIS2_PLACEMENT_3D ( 'NONE', #15074, #50806, #51323 ) ;
#11896 = ORIENTED_EDGE ( 'NONE', *, *, #32929, .T. ) ;
#11897 = ORIENTED_EDGE ( 'NONE', *, *, #36441, .T. ) ;
#11898 = EDGE_CURVE ( 'NONE', #8967, #35821, #49042, .T. ) ;
#11900 = ORIENTED_EDGE ( 'NONE', *, *, #52003, .F. ) ;
#11899 = AXIS2_PLACEMENT_3D ( 'NONE', #4797, #20822, #25530 ) ;
#11901 = PLANE ( 'NONE',  #44252 ) ;
#11902 = CARTESIAN_POINT ( 'NONE',  ( 15.23368049493606335, -175.3837268820161057, -107.5438431188757562 ) ) ;
#11903 = LINE ( 'NONE', #43967, #44256 ) ;
#11904 = DIRECTION ( 'NONE',  ( -0.000000000000000000, 1.000000000000000000, -0.000000000000000000 ) ) ;
#11905 = CARTESIAN_POINT ( 'NONE',  ( 29.40217425202905233, -177.1207230881787780, -96.49160960477045990 ) ) ;
#11906 = ORIENTED_EDGE ( 'NONE', *, *, #11651, .T. ) ;
#11907 = PLANE ( 'NONE',  #13786 ) ;
#11908 = LINE ( 'NONE', #28708, #8956 ) ;
#11909 = CARTESIAN_POINT ( 'NONE',  ( -22.44626007086657182, -177.1207230881787780, 122.2591094863196730 ) ) ;
#11910 = LINE ( 'NONE', #20066, #10613 ) ;
#11911 = AXIS2_PLACEMENT_3D ( 'NONE', #44476, #21073, #1094 ) ;
#11912 = ORIENTED_EDGE ( 'NONE', *, *, #18868, .F. ) ;
#11913 = ORIENTED_EDGE ( 'NONE', *, *, #32353, .F. ) ;
#11914 = VECTOR ( 'NONE', #30264, 1000.000000000000000 ) ;
#11915 = ORIENTED_EDGE ( 'NONE', *, *, #41660, .F. ) ;
#11916 = VECTOR ( 'NONE', #23496, 1000.000000000000000 ) ;
#11917 = DIRECTION ( 'NONE',  ( -1.000000000000000000, -0.000000000000000000, -0.000000000000000000 ) ) ;
#11918 = CARTESIAN_POINT ( 'NONE',  ( -170.0000000000000284, -123.5000000000000284, -45.63467731922664683 ) ) ;
#11919 = EDGE_LOOP ( 'NONE', ( #46264, #49208, #28591, #24805 ) ) ;
#11920 = CARTESIAN_POINT ( 'NONE',  ( -330.4913330509368166, -150.9396941197148294, 53.35787839313412206 ) ) ;
#11921 = LINE ( 'NONE', #14867, #6940 ) ;
#11922 = DIRECTION ( 'NONE',  ( -0.8294056854502090959, 0.000000000000000000, 0.5586467658036415873 ) ) ;
#11923 = EDGE_LOOP ( 'NONE', ( #20276, #47211, #2945, #19308 ) ) ;
#11924 = DIRECTION ( 'NONE',  ( -0.000000000000000000, -1.000000000000000000, -0.000000000000000000 ) ) ;
#11925 = ORIENTED_EDGE ( 'NONE', *, *, #1563, .T. ) ;
#11926 = DIRECTION ( 'NONE',  ( 0.000000000000000000, 1.000000000000000000, -0.000000000000000000 ) ) ;
#11927 = ORIENTED_EDGE ( 'NONE', *, *, #3146, .T. ) ;
#11928 = CARTESIAN_POINT ( 'NONE',  ( -339.1964088526558498, -75.22798428563991990, -33.92731199008514409 ) ) ;
#11929 = CARTESIAN_POINT ( 'NONE',  ( 7.859956736328458149, -193.5000000000000000, -111.5836353223468649 ) ) ;
#11930 = ORIENTED_EDGE ( 'NONE', *, *, #32416, .T. ) ;
#11931 = CIRCLE ( 'NONE', #28734, 16.00000000000000000 ) ;
#11932 = CARTESIAN_POINT ( 'NONE',  ( -180.0000000000000568, -123.5000000000000284, 41.63467731922665394 ) ) ;
#11933 = FACE_OUTER_BOUND ( 'NONE', #8577, .T. ) ;
#11934 = LINE ( 'NONE', #32174, #40809 ) ;
#11935 = EDGE_CURVE ( 'NONE', #12462, #47079, #37201, .T. ) ;
#11936 = DIRECTION ( 'NONE',  ( 0.000000000000000000, -0.000000000000000000, 1.000000000000000000 ) ) ;
#11937 = VECTOR ( 'NONE', #19705, 1000.000000000000000 ) ;
#11938 = VERTEX_POINT ( 'NONE', #13025 ) ;
#11939 = FACE_OUTER_BOUND ( 'NONE', #6431, .T. ) ;
#11940 = ORIENTED_EDGE ( 'NONE', *, *, #20326, .F. ) ;
#11941 = ORIENTED_EDGE ( 'NONE', *, *, #472, .T. ) ;
#11942 = FACE_OUTER_BOUND ( 'NONE', #37826, .T. ) ;
#11944 = EDGE_LOOP ( 'NONE', ( #596, #9595, #10897, #26076 ) ) ;
#11943 = CARTESIAN_POINT ( 'NONE',  ( -365.0000000000001137, -78.50000000000002842, -5.000000000000001776 ) ) ;
#11945 = ORIENTED_EDGE ( 'NONE', *, *, #39691, .T. ) ;
#11946 = LINE ( 'NONE', #9327, #42480 ) ;
#11947 = CIRCLE ( 'NONE', #13652, 125.0000000000000000 ) ;
#11948 = AXIS2_PLACEMENT_3D ( 'NONE', #47942, #43989, #3785 ) ;
#11949 = PRODUCT_DEFINITION ( 'UNKNOWN', '', #45229, #43199 ) ;
#11950 = DIRECTION ( 'NONE',  ( 0.000000000000000000, 1.000000000000000000, -0.000000000000000000 ) ) ;
#11951 = VECTOR ( 'NONE', #8576, 1000.000000000000000 ) ;
#11952 = VECTOR ( 'NONE', #41094, 1000.000000000000000 ) ;
#11953 = ORIENTED_EDGE ( 'NONE', *, *, #31220, .F. ) ;
#11954 = DIRECTION ( 'NONE',  ( 0.000000000000000000, -1.000000000000000000, 0.000000000000000000 ) ) ;
#11955 = DIRECTION ( 'NONE',  ( 0.000000000000000000, -6.568819562365509110E-14, 1.000000000000000000 ) ) ;
#11956 = EDGE_CURVE ( 'NONE', #9002, #30647, #7468, .T. ) ;
#11957 = ORIENTED_EDGE ( 'NONE', *, *, #47394, .F. ) ;
#11958 = DIRECTION ( 'NONE',  ( -1.000000000000000000, 0.000000000000000000, 0.000000000000000000 ) ) ;
#11959 = DIRECTION ( 'NONE',  ( -0.000000000000000000, 1.000000000000000000, -0.000000000000000000 ) ) ;
#11960 = CARTESIAN_POINT ( 'NONE',  ( -339.1964088526558498, -123.5000000000000284, 0.000000000000000000 ) ) ;
#11961 = LINE ( 'NONE', #23541, #11458 ) ;
#11962 = ORIENTED_EDGE ( 'NONE', *, *, #44287, .T. ) ;
#11963 = ORIENTED_EDGE ( 'NONE', *, *, #6101, .F. ) ;
#11964 = EDGE_CURVE ( 'NONE', #50728, #5970, #28014, .T. ) ;
#11965 = ORIENTED_EDGE ( 'NONE', *, *, #35748, .T. ) ;
#11966 = DIRECTION ( 'NONE',  ( -0.6965510290630033685, 0.000000000000000000, 0.7175072570443249420 ) ) ;
#11967 = DIRECTION ( 'NONE',  ( -0.000000000000000000, -0.2393156642875482742, 0.9709418174260544543 ) ) ;
#11968 = CARTESIAN_POINT ( 'NONE',  ( -56.71246971489870958, -189.7472609257535510, -124.7285535218267682 ) ) ;
#11969 = FACE_BOUND ( 'NONE', #36564, .T. ) ;
#11970 = CARTESIAN_POINT ( 'NONE',  ( -180.0000000000000568, -123.5000000000000284, -41.63467731922663972 ) ) ;
#11971 = VECTOR ( 'NONE', #23827, 1000.000000000000000 ) ;
#11972 = ORIENTED_EDGE ( 'NONE', *, *, #27480, .F. ) ;
#11973 = ADVANCED_FACE ( 'NONE', ( #31963 ), #24595, .F. ) ;
#11974 = PLANE ( 'NONE',  #3957 ) ;
#11975 = VERTEX_POINT ( 'NONE', #21180 ) ;
#11977 = VERTEX_POINT ( 'NONE', #159 ) ;
#11976 = DIRECTION ( 'NONE',  ( 0.000000000000000000, -0.8854560256532062468, 0.4647231720437755564 ) ) ;
#11978 = ORIENTED_EDGE ( 'NONE', *, *, #36487, .F. ) ;
#11979 = DIRECTION ( 'NONE',  ( 0.000000000000000000, 1.000000000000000000, -0.000000000000000000 ) ) ;
#11980 = FACE_OUTER_BOUND ( 'NONE', #14534, .T. ) ;
#11981 = CARTESIAN_POINT ( 'NONE',  ( -2.700932609314990351, -183.6283474603465606, -116.3157639405751667 ) ) ;
#11982 = DIRECTION ( 'NONE',  ( -8.718379230999707126E-17, -0.1205366802553095307, 0.9927088740980556381 ) ) ;
#11983 = EDGE_LOOP ( 'NONE', ( #27793, #17115, #25997, #46168 ) ) ;
#11984 = LINE ( 'NONE', #28282, #2383 ) ;
#11985 = VECTOR ( 'NONE', #47835, 1000.000000000000227 ) ;
#11986 = ORIENTED_EDGE ( 'NONE', *, *, #14637, .F. ) ;
#11987 = VECTOR ( 'NONE', #50688, 1000.000000000000000 ) ;
#11988 = EDGE_CURVE ( 'NONE', #38775, #39946, #32746, .T. ) ;
#11989 = EDGE_LOOP ( 'NONE', ( #35512, #45663, #3391, #31984 ) ) ;
#11990 = FACE_OUTER_BOUND ( 'NONE', #18184, .T. ) ;
#11991 = CIRCLE ( 'NONE', #30454, 60.00000000000000000 ) ;
#11992 = CARTESIAN_POINT ( 'NONE',  ( -31.30262293407084329, -177.1207230881787780, -123.8142468240611436 ) ) ;
#11993 = LINE ( 'NONE', #40116, #23205 ) ;
#11994 = FACE_OUTER_BOUND ( 'NONE', #1083, .T. ) ;
#11995 = FACE_OUTER_BOUND ( 'NONE', #37248, .T. ) ;
#11996 = DIRECTION ( 'NONE',  ( 0.000000000000000000, 0.000000000000000000, 1.000000000000000000 ) ) ;
#11997 = ADVANCED_FACE ( 'NONE', ( #48001 ), #28280, .F. ) ;
#11998 = VECTOR ( 'NONE', #28305, 1000.000000000000000 ) ;
#11999 = EDGE_LOOP ( 'NONE', ( #30901, #36558, #3917, #33661 ) ) ;
#12000 = LINE ( 'NONE', #431, #38080 ) ;
#12001 = DIRECTION ( 'NONE',  ( -1.000000000000000000, 0.000000000000000000, 0.000000000000000000 ) ) ;
#12002 = FACE_BOUND ( 'NONE', #26074, .T. ) ;
#12003 = ORIENTED_EDGE ( 'NONE', *, *, #14914, .F. ) ;
#12004 = EDGE_CURVE ( 'NONE', #25971, #16316, #44052, .T. ) ;
#12005 = DIRECTION ( 'NONE',  ( 1.000000000000000000, -7.175085443855143705E-17, -4.952603889763953902E-17 ) ) ;
#12006 = AXIS2_PLACEMENT_3D ( 'NONE', #7226, #43216, #19063 ) ;
#12007 = PLANE ( 'NONE',  #49629 ) ;
#12008 = ORIENTED_EDGE ( 'NONE', *, *, #46389, .T. ) ;
#12009 = DIRECTION ( 'NONE',  ( -0.000000000000000000, -3.491481338843133355E-15, -1.000000000000000000 ) ) ;
#12010 = ORIENTED_EDGE ( 'NONE', *, *, #34594, .T. ) ;
#12011 = AXIS2_PLACEMENT_3D ( 'NONE', #29289, #22183, #45080 ) ;
#12012 = DIRECTION ( 'NONE',  ( 0.000000000000000000, -0.000000000000000000, 1.000000000000000000 ) ) ;
#12013 = FACE_BOUND ( 'NONE', #33867, .T. ) ;
#12015 = ORIENTED_EDGE ( 'NONE', *, *, #37586, .T. ) ;
#12014 = CARTESIAN_POINT ( 'NONE',  ( -172.3973245609188041, -175.3837268820161057, 4.503971736581616092 ) ) ;
#12016 = EDGE_CURVE ( 'NONE', #44148, #43156, #42727, .T. ) ;
#12018 = CIRCLE ( 'NONE', #41406, 125.0000000000000000 ) ;
#12017 = DIRECTION ( 'NONE',  ( -0.000000000000000000, -0.8229838658936516893, 0.5680647467311626952 ) ) ;
#12019 = ORIENTED_EDGE ( 'NONE', *, *, #49762, .T. ) ;
#12020 = ORIENTED_EDGE ( 'NONE', *, *, #7699, .T. ) ;
#12021 = LINE ( 'NONE', #36198, #4083 ) ;
#12022 = VECTOR ( 'NONE', #1258, 1000.000000000000000 ) ;
#12023 = ORIENTED_EDGE ( 'NONE', *, *, #28860, .T. ) ;
#12024 = CARTESIAN_POINT ( 'NONE',  ( -49.45768324380835423, -177.1207230881787780, -0.2059786187411025149 ) ) ;
#12025 = DIRECTION ( 'NONE',  ( -0.1768902751225733261, 0.000000000000000000, 0.9842305779475966077 ) ) ;
#12026 = CARTESIAN_POINT ( 'NONE',  ( -47.55243714407701816, -193.5000000000000000, -0.3758275821142288420 ) ) ;
#12027 = ORIENTED_EDGE ( 'NONE', *, *, #7006, .F. ) ;
#12030 = ORIENTED_EDGE ( 'NONE', *, *, #38401, .T. ) ;
#12029 = DIRECTION ( 'NONE',  ( 0.000000000000000000, 1.000000000000000000, 0.000000000000000000 ) ) ;
#12028 = DIRECTION ( 'NONE',  ( -1.000000000000000000, 0.000000000000000000, 0.000000000000000000 ) ) ;
#12031 = VERTEX_POINT ( 'NONE', #413 ) ;
#12032 = DIRECTION ( 'NONE',  ( 0.000000000000000000, -1.000000000000000000, 0.000000000000000000 ) ) ;
#12033 = VERTEX_POINT ( 'NONE', #8823 ) ;
#12034 = DIRECTION ( 'NONE',  ( 0.000000000000000000, -0.000000000000000000, 1.000000000000000000 ) ) ;
#12035 = VECTOR ( 'NONE', #2834, 1000.000000000000000 ) ;
#12036 = EDGE_LOOP ( 'NONE', ( #21587, #49756, #7404, #31423 ) ) ;
#12037 = ADVANCED_FACE ( 'NONE', ( #48786 ), #28781, .F. ) ;
#12038 = EDGE_CURVE ( 'NONE', #12735, #20792, #49464, .T. ) ;
#12039 = DIRECTION ( 'NONE',  ( 0.000000000000000000, 1.000000000000000000, 0.000000000000000000 ) ) ;
#12040 = ORIENTED_EDGE ( 'NONE', *, *, #305, .F. ) ;
#12042 = LINE ( 'NONE', #29120, #10701 ) ;
#12041 = CARTESIAN_POINT ( 'NONE',  ( -305.0000000000000568, -77.52356969168074841, 38.55084767037245541 ) ) ;
#12043 = EDGE_LOOP ( 'NONE', ( #8945, #48752 ) ) ;
#12044 = VECTOR ( 'NONE', #35145, 1000.000000000000000 ) ;
#12045 = EDGE_LOOP ( 'NONE', ( #47661, #3834, #4684, #3790 ) ) ;
#12046 = DIRECTION ( 'NONE',  ( 0.000000000000000000, -0.4739294676984007193, 0.8805628084623552398 ) ) ;
#12047 = FACE_OUTER_BOUND ( 'NONE', #25787, .T. ) ;
#12048 = PLANE ( 'NONE',  #32230 ) ;
#12049 = DIRECTION ( 'NONE',  ( -0.000000000000000000, 1.000000000000000000, -0.000000000000000000 ) ) ;
#12050 = CARTESIAN_POINT ( 'NONE',  ( 53.56330073376472711, -175.3837268820161057, 72.19655804062050208 ) ) ;
#12051 = DIRECTION ( 'NONE',  ( 0.000000000000000000, -0.000000000000000000, 1.000000000000000000 ) ) ;
#12052 = ORIENTED_EDGE ( 'NONE', *, *, #40206, .T. ) ;
#12053 = DIRECTION ( 'NONE',  ( 0.000000000000000000, 0.000000000000000000, 1.000000000000000000 ) ) ;
#12054 = EDGE_CURVE ( 'NONE', #19748, #6892, #4907, .T. ) ;
#12055 = CIRCLE ( 'NONE', #44825, 125.0000000000000000 ) ;
#12056 = DIRECTION ( 'NONE',  ( 0.9890401873221654760, 0.000000000000000000, -0.1476465640024710868 ) ) ;
#12057 = CARTESIAN_POINT ( 'NONE',  ( -173.4724443937511751, -183.6283474603465606, 1.292495564989516454 ) ) ;
#12058 = EDGE_CURVE ( 'NONE', #36418, #7888, #11657, .T. ) ;
#12059 = FACE_OUTER_BOUND ( 'NONE', #46392, .T. ) ;
#12060 = ORIENTED_EDGE ( 'NONE', *, *, #16947, .F. ) ;
#12061 = ADVANCED_FACE ( 'NONE', ( #32995 ), #10380, .F. ) ;
#12062 = CARTESIAN_POINT ( 'NONE',  ( -7.515176836080581957, -183.6283474603465606, 117.0391155081705250 ) ) ;
#12063 = DIRECTION ( 'NONE',  ( -0.000000000000000000, -0.8854560256532062468, 0.4647231720437755564 ) ) ;
#12064 = DIRECTION ( 'NONE',  ( -1.000000000000000000, 0.000000000000000000, 0.000000000000000000 ) ) ;
#12065 = ORIENTED_EDGE ( 'NONE', *, *, #7953, .F. ) ;
#12066 = EDGE_LOOP ( 'NONE', ( #3846, #8341, #37130, #25197 ) ) ;
#12067 = ORIENTED_EDGE ( 'NONE', *, *, #4506, .F. ) ;
#12068 = CARTESIAN_POINT ( 'NONE',  ( -339.1964088526558498, -182.0095552316576573, -7.608018572112655420 ) ) ;
#12069 = LINE ( 'NONE', #11045, #41313 ) ;
#12070 = CARTESIAN_POINT ( 'NONE',  ( -48.47912675150885065, -120.5000000000000284, 6.938893903907228378E-15 ) ) ;
#12071 = CARTESIAN_POINT ( 'NONE',  ( -330.4913330509368166, -183.0001959263613571, 7.728304129925096966 ) ) ;
#12072 = VECTOR ( 'NONE', #16757, 1000.000000000000000 ) ;
#12073 = EDGE_LOOP ( 'NONE', ( #36097, #32914, #17637, #22500 ) ) ;
#12074 = VECTOR ( 'NONE', #4192, 1000.000000000000000 ) ;
#12075 = DIRECTION ( 'NONE',  ( 0.000000000000000000, 0.000000000000000000, -1.000000000000000000 ) ) ;
#12076 = EDGE_LOOP ( 'NONE', ( #23781, #15142, #49073, #44626 ) ) ;
#12077 = AXIS2_PLACEMENT_3D ( 'NONE', #48552, #28292, #36706 ) ;
#12078 = ORIENTED_EDGE ( 'NONE', *, *, #42271, .T. ) ;
#12079 = ORIENTED_EDGE ( 'NONE', *, *, #7670, .F. ) ;
#12080 = ORIENTED_EDGE ( 'NONE', *, *, #48430, .T. ) ;
#12081 = CARTESIAN_POINT ( 'NONE',  ( -336.3521761649654422, -100.1170788342122080, 54.23253582808833073 ) ) ;
#12083 = ORIENTED_EDGE ( 'NONE', *, *, #44217, .T. ) ;
#12082 = CIRCLE ( 'NONE', #41478, 60.00000000000000000 ) ;
#12084 = DIRECTION ( 'NONE',  ( -1.000000000000000000, -1.258058860540462198E-15, 1.036104688092336837E-14 ) ) ;
#12085 = CARTESIAN_POINT ( 'NONE',  ( 0.000000000000000000, -172.0560480877259408, -33.51582005713793677 ) ) ;
#12088 = ORIENTED_EDGE ( 'NONE', *, *, #44871, .F. ) ;
#12087 = DIRECTION ( 'NONE',  ( 0.000000000000000000, 0.7485107481710977506, -0.6631226582407989678 ) ) ;
#12086 = DIRECTION ( 'NONE',  ( -0.2920567706369694982, 0.000000000000000000, -0.9564009842765243130 ) ) ;
#12089 = CARTESIAN_POINT ( 'NONE',  ( 18.49541618049843095, -193.5000000000000000, 105.5434062319798159 ) ) ;
#12090 = VERTEX_POINT ( 'NONE', #45882 ) ;
#12091 = CARTESIAN_POINT ( 'NONE',  ( -339.1964088526558498, -66.09477493971917283, -13.63415328425296202 ) ) ;
#12092 = ORIENTED_EDGE ( 'NONE', *, *, #31985, .F. ) ;
#12093 = ADVANCED_FACE ( 'NONE', ( #38234 ), #25898, .F. ) ;
#12094 = ADVANCED_FACE ( 'NONE', ( #21709 ), #29318, .T. ) ;
#12095 = EDGE_CURVE ( 'NONE', #35357, #1515, #33504, .T. ) ;
#12096 = CARTESIAN_POINT ( 'NONE',  ( 20.93410174202488250, -189.7472609257535510, -102.7511748916624441 ) ) ;
#12097 = LINE ( 'NONE', #43137, #30490 ) ;
#12099 = LINE ( 'NONE', #40742, #36592 ) ;
#12098 = DIRECTION ( 'NONE',  ( -0.000000000000000000, 0.2393156642875685636, 0.9709418174260492362 ) ) ;
#12100 = EDGE_LOOP ( 'NONE', ( #23294, #37526, #27968, #49 ) ) ;
#12101 = EDGE_CURVE ( 'NONE', #34375, #3787, #18285, .T. ) ;
#12102 = CARTESIAN_POINT ( 'NONE',  ( -159.8192355313504720, -193.5000000000000000, -56.81883646197830018 ) ) ;
#12103 = CARTESIAN_POINT ( 'NONE',  ( 70.68712318874649725, -177.1207230881787780, -37.74128873232327663 ) ) ;
#12104 = ORIENTED_EDGE ( 'NONE', *, *, #27726, .T. ) ;
#12105 = ADVANCED_FACE ( 'NONE', ( #21954 ), #25630, .F. ) ;
#12106 = DIRECTION ( 'NONE',  ( 0.9993203489176063492, 0.000000000000000000, 0.03686245026030503941 ) ) ;
#12107 = DIRECTION ( 'NONE',  ( 0.9890401873221633666, 0.000000000000000000, 0.1476465640024850756 ) ) ;
#12108 = EDGE_CURVE ( 'NONE', #44462, #3230, #14334, .T. ) ;
#12109 = AXIS2_PLACEMENT_3D ( 'NONE', #31563, #16069, #48121 ) ;
#12110 = DIRECTION ( 'NONE',  ( 0.000000000000000000, 0.000000000000000000, 1.000000000000000000 ) ) ;
#12111 = VECTOR ( 'NONE', #48162, 1000.000000000000000 ) ;
#12112 = ORIENTED_EDGE ( 'NONE', *, *, #12497, .T. ) ;
#12113 = PLANE ( 'NONE',  #17545 ) ;
#12114 = EDGE_CURVE ( 'NONE', #39091, #46272, #25386, .T. ) ;
#12116 = AXIS2_PLACEMENT_3D ( 'NONE', #15079, #21914, #34503 ) ;
#12115 = CARTESIAN_POINT ( 'NONE',  ( -339.1964088526558498, -167.3305728129748786, -39.49849221029221269 ) ) ;
#12117 = ADVANCED_FACE ( 'NONE', ( #5420 ), #50089, .T. ) ;
#12118 = ORIENTED_EDGE ( 'NONE', *, *, #28607, .F. ) ;
#12119 = DIRECTION ( 'NONE',  ( 1.000000000000000000, -0.000000000000000000, -0.000000000000000000 ) ) ;
#12120 = ORIENTED_EDGE ( 'NONE', *, *, #29167, .F. ) ;
#12121 = EDGE_CURVE ( 'NONE', #30190, #41581, #22211, .T. ) ;
#12122 = DIRECTION ( 'NONE',  ( 0.000000000000000000, 0.000000000000000000, 1.000000000000000000 ) ) ;
#12123 = LINE ( 'NONE', #44202, #5136 ) ;
#12124 = EDGE_CURVE ( 'NONE', #1492, #12178, #50344, .T. ) ;
#12125 = DIRECTION ( 'NONE',  ( -0.000000000000000000, 1.000000000000000000, -1.047444401652940007E-14 ) ) ;
#12126 = CARTESIAN_POINT ( 'NONE',  ( -48.47912675150885065, -183.6283474603465606, 6.938893903907228378E-15 ) ) ;
#12127 = CARTESIAN_POINT ( 'NONE',  ( -330.4913330509368166, -162.2499814621216672, -44.49369547121515467 ) ) ;
#12128 = AXIS2_PLACEMENT_3D ( 'NONE', #43969, #23245, #28192 ) ;
#12129 = DIRECTION ( 'NONE',  ( -0.000000000000000000, 1.000000000000000000, -0.000000000000000000 ) ) ;
#12130 = CARTESIAN_POINT ( 'NONE',  ( 44.30815888362531041, -193.5000000000000000, 83.75869879877569701 ) ) ;
#12131 = DIRECTION ( 'NONE',  ( -0.000000000000000000, -0.1205366802553268363, -0.9927088740980534176 ) ) ;
#12133 = VERTEX_POINT ( 'NONE', #21437 ) ;
#12132 = CARTESIAN_POINT ( 'NONE',  ( -167.9436818089035057, -193.5000000000000000, 36.78613984830044359 ) ) ;
#12134 = VERTEX_POINT ( 'NONE', #26404 ) ;
#12135 = DIRECTION ( 'NONE',  ( -0.000000000000000000, 0.2393156642875547968, -0.9709418174260527890 ) ) ;
#12136 = EDGE_CURVE ( 'NONE', #6991, #49014, #37463, .T. ) ;
#12137 = DIRECTION ( 'NONE',  ( 0.000000000000000000, 1.000000000000000000, 0.000000000000000000 ) ) ;
#12138 = VERTEX_POINT ( 'NONE', #13551 ) ;
#12139 = ORIENTED_EDGE ( 'NONE', *, *, #6428, .F. ) ;
#12140 = AXIS2_PLACEMENT_3D ( 'NONE', #24668, #49633, #5495 ) ;
#12141 = VERTEX_POINT ( 'NONE', #1724 ) ;
#12142 = FACE_OUTER_BOUND ( 'NONE', #8554, .T. ) ;
#12143 = AXIS2_PLACEMENT_3D ( 'NONE', #45423, #33584, #16797 ) ;
#12144 = VECTOR ( 'NONE', #19129, 1000.000000000000114 ) ;
#12145 = PLANE ( 'NONE',  #17760 ) ;
#12146 = LINE ( 'NONE', #12671, #1458 ) ;
#12147 = ORIENTED_EDGE ( 'NONE', *, *, #6223, .T. ) ;
#12148 = EDGE_LOOP ( 'NONE', ( #35936, #41715, #1060, #38091 ) ) ;
#12149 = VECTOR ( 'NONE', #44728, 1000.000000000000000 ) ;
#12150 = EDGE_LOOP ( 'NONE', ( #49990, #42981, #38915, #24838 ) ) ;
#12151 = ADVANCED_FACE ( 'NONE', ( #33780 ), #14082, .T. ) ;
#12152 = LINE ( 'NONE', #16381, #40027 ) ;
#12153 = CYLINDRICAL_SURFACE ( 'NONE', #47041, 125.0000000000000000 ) ;
#12154 = CARTESIAN_POINT ( 'NONE',  ( 2.669657140899374337, -175.3837268820161057, 114.0561348912355868 ) ) ;
#12155 = VECTOR ( 'NONE', #12297, 1000.000000000000000 ) ;
#12156 = CARTESIAN_POINT ( 'NONE',  ( -305.0000000000000568, -167.3116148657362032, 40.99441916720376611 ) ) ;
#12157 = AXIS2_PLACEMENT_3D ( 'NONE', #8289, #11954, #1164 ) ;
#12158 = CARTESIAN_POINT ( 'NONE',  ( -48.47912675150885065, -120.5000000000000284, 15.00000000000000711 ) ) ;
#12159 = ORIENTED_EDGE ( 'NONE', *, *, #6704, .F. ) ;
#12160 = CARTESIAN_POINT ( 'NONE',  ( -99.62791064391781504, -175.3837268820161057, -114.0561348912352315 ) ) ;
#12161 = EDGE_CURVE ( 'NONE', #43135, #16449, #1980, .T. ) ;
#12162 = EDGE_CURVE ( 'NONE', #40574, #44930, #46146, .T. ) ;
#12163 = EDGE_CURVE ( 'NONE', #3974, #34018, #26808, .T. ) ;
#12164 = PLANE ( 'NONE',  #5638 ) ;
#12165 = AXIS2_PLACEMENT_3D ( 'NONE', #24992, #40472, #45235 ) ;
#12166 = DIRECTION ( 'NONE',  ( -0.7378332790417333475, 0.000000000000000000, 0.6749830015182038956 ) ) ;
#12167 = DIRECTION ( 'NONE',  ( -0.000000000000000000, 1.000000000000000000, -0.000000000000000000 ) ) ;
#12168 = EDGE_CURVE ( 'NONE', #50038, #1430, #48628, .T. ) ;
#12169 = CIRCLE ( 'NONE', #433, 125.0000000000000000 ) ;
#12170 = ORIENTED_EDGE ( 'NONE', *, *, #26239, .T. ) ;
#12171 = ORIENTED_EDGE ( 'NONE', *, *, #27174, .T. ) ;
#12172 = EDGE_LOOP ( 'NONE', ( #7504, #6318, #8631, #12015 ) ) ;
#12173 = CARTESIAN_POINT ( 'NONE',  ( -48.47912675150885065, -183.6283474603465606, 6.938893903907228378E-15 ) ) ;
#12174 = LINE ( 'NONE', #51896, #20795 ) ;
#12175 = EDGE_LOOP ( 'NONE', ( #28272, #14676, #14904, #41259 ) ) ;
#12176 = CARTESIAN_POINT ( 'NONE',  ( 32.99469856375238663, -193.5000000000000000, 94.79987230212020677 ) ) ;
#12177 = DIRECTION ( 'NONE',  ( 0.000000000000000000, 7.725301879683381348E-14, 1.000000000000000000 ) ) ;
#12178 = VERTEX_POINT ( 'NONE', #3013 ) ;
#12179 = DIRECTION ( 'NONE',  ( 0.000000000000000000, -0.9350162426854181641, -0.3546048870425267951 ) ) ;
#12180 = EDGE_CURVE ( 'NONE', #28004, #19813, #39277, .T. ) ;
#12181 = ORIENTED_EDGE ( 'NONE', *, *, #37833, .F. ) ;
#12182 = CARTESIAN_POINT ( 'NONE',  ( 67.29303306501927295, -193.5000000000000000, 47.13604789772129777 ) ) ;
#12183 = ORIENTED_EDGE ( 'NONE', *, *, #51100, .F. ) ;
#12184 = CARTESIAN_POINT ( 'NONE',  ( -330.4913330509368166, -84.75001853787871653, -44.49369547121542467 ) ) ;
#12185 = CARTESIAN_POINT ( 'NONE',  ( 67.64905612629584652, -193.5000000000000000, -43.47841891815122750 ) ) ;
#12186 = CIRCLE ( 'NONE', #21428, 60.00000000000000000 ) ;
#12187 = EDGE_CURVE ( 'NONE', #25065, #34424, #31380, .T. ) ;
#12188 = DIRECTION ( 'NONE',  ( -0.000000000000000000, -0.5680647467311596976, -0.8229838658936536877 ) ) ;
#12189 = ORIENTED_EDGE ( 'NONE', *, *, #45194, .T. ) ;
#12190 = VECTOR ( 'NONE', #26343, 1000.000000000000000 ) ;
#12191 = AXIS2_PLACEMENT_3D ( 'NONE', #4784, #7680, #33145 ) ;
#12192 = EDGE_CURVE ( 'NONE', #2225, #20894, #18534, .T. ) ;
#12193 = CARTESIAN_POINT ( 'NONE',  ( -118.9967449635792320, -175.3837268820161057, -103.2098131075562009 ) ) ;
#12194 = FACE_OUTER_BOUND ( 'NONE', #379, .T. ) ;
#12195 = CARTESIAN_POINT ( 'NONE',  ( -49.38192458147459263, -175.3837268820161057, -0.4300652022765235616 ) ) ;
#12196 = CARTESIAN_POINT ( 'NONE',  ( -339.1964088526558498, -64.50000000000000000, 0.4999999999999543698 ) ) ;
#12197 = VECTOR ( 'NONE', #37227, 1000.000000000000114 ) ;
#12198 = EDGE_CURVE ( 'NONE', #40491, #42583, #30971, .T. ) ;
#12199 = ORIENTED_EDGE ( 'NONE', *, *, #40056, .T. ) ;
#12200 = DIRECTION ( 'NONE',  ( -8.718379230999707126E-17, -0.8854560256532141294, -0.4647231720437604574 ) ) ;
#12201 = VERTEX_POINT ( 'NONE', #19561 ) ;
#12202 = VERTEX_POINT ( 'NONE', #47174 ) ;
#12203 = AXIS2_PLACEMENT_3D ( 'NONE', #9157, #38025, #29625 ) ;
#12204 = CARTESIAN_POINT ( 'NONE',  ( 30.05499637021956261, -183.6283474603465606, -97.24912084693207248 ) ) ;
#12206 = VERTEX_POINT ( 'NONE', #2752 ) ;
#12205 = PLANE ( 'NONE',  #10204 ) ;
#12207 = VECTOR ( 'NONE', #39493, 1000.000000000000000 ) ;
#12208 = ORIENTED_EDGE ( 'NONE', *, *, #41732, .T. ) ;
#12209 = PLANE ( 'NONE',  #21283 ) ;
#12210 = VECTOR ( 'NONE', #18526, 1000.000000000000114 ) ;
#12211 = EDGE_CURVE ( 'NONE', #18701, #4655, #39522, .T. ) ;
#12212 = AXIS2_PLACEMENT_3D ( 'NONE', #48843, #49095, #44379 ) ;
#12213 = DIRECTION ( 'NONE',  ( 0.000000000000000000, -1.000000000000000000, 0.000000000000000000 ) ) ;
#12214 = ORIENTED_EDGE ( 'NONE', *, *, #29740, .F. ) ;
#12215 = CARTESIAN_POINT ( 'NONE',  ( -171.9740864388383557, -175.3837268820161057, -11.18012358327901623 ) ) ;
#12216 = DIRECTION ( 'NONE',  ( -0.9890401873221623674, 0.000000000000000000, -0.1476465640024917925 ) ) ;
#12217 = ORIENTED_EDGE ( 'NONE', *, *, #29494, .F. ) ;
#12218 = CARTESIAN_POINT ( 'NONE',  ( -330.4913330509368166, -124.0000000000001990, -59.99791663049643375 ) ) ;
#12219 = CARTESIAN_POINT ( 'NONE',  ( -92.43312097795268301, -193.5000000000000000, -115.9484881370935483 ) ) ;
#12220 = CARTESIAN_POINT ( 'NONE',  ( -71.40672220061269115, -189.7472609257535510, -122.8793122007208751 ) ) ;
#12221 = PLANE ( 'NONE',  #2254 ) ;
#12222 = ORIENTED_EDGE ( 'NONE', *, *, #18952, .T. ) ;
#12223 = EDGE_LOOP ( 'NONE', ( #40513, #33703, #39484, #29358 ) ) ;
#12224 = ORIENTED_EDGE ( 'NONE', *, *, #17626, .F. ) ;
#12225 = DIRECTION ( 'NONE',  ( 0.6965510290629932655, 0.000000000000000000, 0.7175072570443347120 ) ) ;
#12226 = CARTESIAN_POINT ( 'NONE',  ( -365.0000000000001137, -168.5000000000000284, 10.00000000000000711 ) ) ;
#12227 = AXIS2_PLACEMENT_3D ( 'NONE', #43867, #7867, #32290 ) ;
#12228 = DIRECTION ( 'NONE',  ( 0.000000000000000000, 0.000000000000000000, -1.000000000000000000 ) ) ;
#12229 = AXIS2_PLACEMENT_3D ( 'NONE', #33343, #17582, #1270 ) ;
#12230 = FACE_BOUND ( 'NONE', #33332, .T. ) ;
#12231 = PLANE ( 'NONE',  #15495 ) ;
#12232 = ORIENTED_EDGE ( 'NONE', *, *, #24380, .T. ) ;
#12233 = VECTOR ( 'NONE', #51836, 1000.000000000000114 ) ;
#12234 = EDGE_CURVE ( 'NONE', #6625, #49882, #51381, .T. ) ;
#12235 = EDGE_CURVE ( 'NONE', #33039, #9410, #11405, .T. ) ;
#12236 = ORIENTED_EDGE ( 'NONE', *, *, #2219, .T. ) ;
#12238 = VERTEX_POINT ( 'NONE', #18788 ) ;
#12237 = PLANE ( 'NONE',  #25637 ) ;
#12239 = VERTEX_POINT ( 'NONE', #27444 ) ;
#12240 = DIRECTION ( 'NONE',  ( -0.000000000000000000, 1.000000000000000000, -0.000000000000000000 ) ) ;
#12241 = AXIS2_PLACEMENT_3D ( 'NONE', #5551, #34423, #49688 ) ;
#12242 = FACE_OUTER_BOUND ( 'NONE', #25160, .T. ) ;
#12243 = AXIS2_PLACEMENT_3D ( 'NONE', #29272, #45325, #49779 ) ;
#12244 = DIRECTION ( 'NONE',  ( -1.000000000000000000, -0.000000000000000000, 0.000000000000000000 ) ) ;
#12245 = DIRECTION ( 'NONE',  ( -0.000000000000000000, 1.000000000000000000, -0.000000000000000000 ) ) ;
#12246 = VERTEX_POINT ( 'NONE', #6963 ) ;
#12247 = DIRECTION ( 'NONE',  ( 0.4677363560876406923, 0.000000000000000000, 0.8838680338115276758 ) ) ;
#12248 = VECTOR ( 'NONE', #50473, 1000.000000000000000 ) ;
#12249 = VERTEX_POINT ( 'NONE', #43486 ) ;
#12250 = VECTOR ( 'NONE', #32538, 1000.000000000000227 ) ;
#12251 = ORIENTED_EDGE ( 'NONE', *, *, #39812, .F. ) ;
#12252 = DIRECTION ( 'NONE',  ( 0.2920567706369764371, 0.000000000000000000, -0.9564009842765223146 ) ) ;
#12253 = ADVANCED_FACE ( 'NONE', ( #23263 ), #26679, .F. ) ;
#12254 = DIRECTION ( 'NONE',  ( -0.6965510290629932655, 0.000000000000000000, -0.7175072570443347120 ) ) ;
#12255 = DIRECTION ( 'NONE',  ( -0.000000000000000000, 1.000000000000000000, -0.000000000000000000 ) ) ;
#12256 = DIRECTION ( 'NONE',  ( -0.000000000000000000, -0.5680647467311596976, -0.8229838658936536877 ) ) ;
#12257 = PLANE ( 'NONE',  #12077 ) ;
#12258 = PLANE ( 'NONE',  #211 ) ;
#12259 = ORIENTED_EDGE ( 'NONE', *, *, #30585, .F. ) ;
#12260 = CARTESIAN_POINT ( 'NONE',  ( -48.47912675150885065, -175.3837268820161057, 6.938893903907228378E-15 ) ) ;
#12261 = CARTESIAN_POINT ( 'NONE',  ( 74.00867759460086859, -189.7472609257535510, 24.93467037017223120 ) ) ;
#12262 = EDGE_CURVE ( 'NONE', #17784, #8540, #8323, .T. ) ;
#12263 = FACE_BOUND ( 'NONE', #12937, .T. ) ;
#12264 = VERTEX_POINT ( 'NONE', #7490 ) ;
#12265 = CIRCLE ( 'NONE', #24011, 60.00000000000000000 ) ;
#12266 = VECTOR ( 'NONE', #6535, 1000.000000000000227 ) ;
#12267 = CARTESIAN_POINT ( 'NONE',  ( -169.7849785064911998, -189.7472609257535510, -25.70779184431772890 ) ) ;
#12268 = VECTOR ( 'NONE', #37140, 1000.000000000000114 ) ;
#12269 = AXIS2_PLACEMENT_3D ( 'NONE', #30149, #10173, #13866 ) ;
#12270 = DIRECTION ( 'NONE',  ( 0.000000000000000000, 0.000000000000000000, 1.000000000000000000 ) ) ;
#12271 = ORIENTED_EDGE ( 'NONE', *, *, #23194, .F. ) ;
#12272 = LINE ( 'NONE', #36722, #218 ) ;
#12273 = ORIENTED_EDGE ( 'NONE', *, *, #23034, .F. ) ;
#12274 = DIRECTION ( 'NONE',  ( 0.000000000000000000, -1.000000000000000000, 0.000000000000000000 ) ) ;
#12275 = AXIS2_PLACEMENT_3D ( 'NONE', #34298, #10642, #14332 ) ;
#12276 = DIRECTION ( 'NONE',  ( -0.000000000000000000, -0.3546048870425267951, 0.9350162426854181641 ) ) ;
#12277 = AXIS2_PLACEMENT_3D ( 'NONE', #16867, #27644, #27884 ) ;
#12279 = ORIENTED_EDGE ( 'NONE', *, *, #8640, .F. ) ;
#12278 = PLANE ( 'NONE',  #23735 ) ;
#12280 = VECTOR ( 'NONE', #9629, 1000.000000000000114 ) ;
#12281 = CIRCLE ( 'NONE', #41656, 60.00000000000000000 ) ;
#12282 = VECTOR ( 'NONE', #27816, 1000.000000000000000 ) ;
#12283 = DIRECTION ( 'NONE',  ( 1.000000000000000000, -0.000000000000000000, 0.000000000000000000 ) ) ;
#12284 = ORIENTED_EDGE ( 'NONE', *, *, #18279, .F. ) ;
#12285 = ORIENTED_EDGE ( 'NONE', *, *, #42983, .T. ) ;
#12286 = VECTOR ( 'NONE', #28710, 1000.000000000000000 ) ;
#12287 = LINE ( 'NONE', #28318, #18378 ) ;
#12288 = ORIENTED_EDGE ( 'NONE', *, *, #27431, .F. ) ;
#12289 = AXIS2_PLACEMENT_3D ( 'NONE', #15482, #27289, #43329 ) ;
#12290 = PLANE ( 'NONE',  #44403 ) ;
#12291 = CARTESIAN_POINT ( 'NONE',  ( -336.3521761649654422, -164.5945333327934463, -42.41660376256285048 ) ) ;
#12292 = ADVANCED_FACE ( 'NONE', ( #3529 ), #3284, .F. ) ;
#12293 = DIRECTION ( 'NONE',  ( -0.000000000000000000, -0.3546048870425267951, 0.9350162426854181641 ) ) ;
#12294 = CARTESIAN_POINT ( 'NONE',  ( -336.3521761649654422, -76.43926241122620979, -35.68215131113738181 ) ) ;
#12295 = ORIENTED_EDGE ( 'NONE', *, *, #31823, .F. ) ;
#12298 = EDGE_LOOP ( 'NONE', ( #8953, #9081, #20333, #24532 ) ) ;
#12297 = DIRECTION ( 'NONE',  ( 1.000000000000000000, -0.000000000000000000, -0.000000000000000000 ) ) ;
#12296 = LINE ( 'NONE', #19934, #6569 ) ;
#12299 = VECTOR ( 'NONE', #51149, 1000.000000000000000 ) ;
#12300 = EDGE_LOOP ( 'NONE', ( #38066, #35533, #35110, #26174 ) ) ;
#12301 = AXIS2_PLACEMENT_3D ( 'NONE', #48738, #44791, #4322 ) ;
#12302 = DIRECTION ( 'NONE',  ( 1.000000000000000000, 4.952603889763975472E-17, -7.175085443855130147E-17 ) ) ;
#12303 = ORIENTED_EDGE ( 'NONE', *, *, #4493, .T. ) ;
#12304 = CARTESIAN_POINT ( 'NONE',  ( -134.9506378406916554, -193.5000000000000000, 90.26448786734091811 ) ) ;
#12305 = ORIENTED_EDGE ( 'NONE', *, *, #48652, .F. ) ;
#12306 = CIRCLE ( 'NONE', #42546, 125.0000000000000000 ) ;
#12307 = FACE_OUTER_BOUND ( 'NONE', #40753, .T. ) ;
#12308 = ORIENTED_EDGE ( 'NONE', *, *, #44941, .T. ) ;
#12310 = CARTESIAN_POINT ( 'NONE',  ( -59.81005805956450416, -193.5000000000000000, -123.4817304940906268 ) ) ;
#12309 = DIRECTION ( 'NONE',  ( -0.8455960035018234011, 0.000000000000000000, -0.5338233779647948429 ) ) ;
#12311 = ORIENTED_EDGE ( 'NONE', *, *, #44940, .F. ) ;
#12312 = EDGE_LOOP ( 'NONE', ( #40167, #41245, #14869, #17478 ) ) ;
#12313 = DIRECTION ( 'NONE',  ( -0.000000000000000000, 1.000000000000000000, -0.000000000000000000 ) ) ;
#12314 = VECTOR ( 'NONE', #43772, 1000.000000000000114 ) ;
#12315 = CARTESIAN_POINT ( 'NONE',  ( -48.47912675150885065, -121.5000000000000142, 15.00000000000000711 ) ) ;
#12316 = VECTOR ( 'NONE', #31109, 1000.000000000000000 ) ;
#12317 = EDGE_CURVE ( 'NONE', #9325, #3589, #35170, .T. ) ;
#12318 = DIRECTION ( 'NONE',  ( 0.8610436117673585521, 0.000000000000000000, -0.5085311186492154079 ) ) ;
#12319 = FACE_OUTER_BOUND ( 'NONE', #15380, .T. ) ;
#12320 = DIRECTION ( 'NONE',  ( -0.000000000000000000, -0.1205366802553130001, 0.9927088740980551940 ) ) ;
#12321 = VECTOR ( 'NONE', #24519, 1000.000000000000000 ) ;
#12322 = VECTOR ( 'NONE', #31584, 1000.000000000000000 ) ;
#12323 = PLANE ( 'NONE',  #41495 ) ;
#12324 = ORIENTED_EDGE ( 'NONE', *, *, #17980, .T. ) ;
#12325 = CIRCLE ( 'NONE', #32439, 125.0000000000000000 ) ;
#12326 = CARTESIAN_POINT ( 'NONE',  ( -339.1964088526558498, -182.1300919119129560, -6.615309698014600670 ) ) ;
#12327 = CARTESIAN_POINT ( 'NONE',  ( -336.3521761649654422, -64.31210272782786319, -9.838334030657643225 ) ) ;
#12328 = CIRCLE ( 'NONE', #20746, 60.00000000000000000 ) ;
#12329 = DIRECTION ( 'NONE',  ( -0.000000000000000000, -0.000000000000000000, -1.000000000000000000 ) ) ;
#12330 = ORIENTED_EDGE ( 'NONE', *, *, #10288, .F. ) ;
#12331 = PLANE ( 'NONE',  #18961 ) ;
#12332 = DIRECTION ( 'NONE',  ( 0.000000000000000000, 1.000000000000000000, -0.000000000000000000 ) ) ;
#12333 = DIRECTION ( 'NONE',  ( -0.000000000000000000, -0.6631226582407989678, -0.7485107481710977506 ) ) ;
#12334 = VERTEX_POINT ( 'NONE', #43733 ) ;
#12335 = VERTEX_POINT ( 'NONE', #7737 ) ;
#12336 = EDGE_LOOP ( 'NONE', ( #43344, #6042, #38213, #6065 ) ) ;
#12337 = AXIS2_PLACEMENT_3D ( 'NONE', #16201, #12240, #28277 ) ;
#12338 = DIRECTION ( 'NONE',  ( -0.08879589532294572540, 0.000000000000000000, 0.9960498426152160079 ) ) ;
#12339 = VECTOR ( 'NONE', #12333, 1000.000000000000000 ) ;
#12340 = DIRECTION ( 'NONE',  ( 0.000000000000000000, 0.000000000000000000, -1.000000000000000000 ) ) ;
#12341 = CARTESIAN_POINT ( 'NONE',  ( -149.5539421794694022, -193.5000000000000000, 73.54509967498655953 ) ) ;
#12342 = CARTESIAN_POINT ( 'NONE',  ( 76.51419089073347379, -183.6283474603465606, -1.292495564988661139 ) ) ;
#12343 = CIRCLE ( 'NONE', #27426, 125.0000000000000000 ) ;
#12344 = ORIENTED_EDGE ( 'NONE', *, *, #4131, .F. ) ;
#12345 = ADVANCED_FACE ( 'NONE', ( #38506 ), #2501, .T. ) ;
#12346 = CARTESIAN_POINT ( 'NONE',  ( -336.3521761649654422, -94.63601285149479736, 51.48334306143172512 ) ) ;
#12347 = ORIENTED_EDGE ( 'NONE', *, *, #51838, .T. ) ;
#12348 = ADVANCED_FACE ( 'NONE', ( #14595 ), #15055, .T. ) ;
#12349 = EDGE_LOOP ( 'NONE', ( #40209, #13863, #33091, #26003 ) ) ;
#12350 = VECTOR ( 'NONE', #50841, 1000.000000000000000 ) ;
#12351 = AXIS2_PLACEMENT_3D ( 'NONE', #23174, #43406, #6879 ) ;
#12352 = ORIENTED_EDGE ( 'NONE', *, *, #49362, .T. ) ;
#12353 = CARTESIAN_POINT ( 'NONE',  ( -165.2002711502080672, -193.5000000000000000, 44.73448837594998651 ) ) ;
#12354 = AXIS2_PLACEMENT_3D ( 'NONE', #36163, #47998, #43542 ) ;
#12355 = EDGE_CURVE ( 'NONE', #47028, #46485, #50861, .T. ) ;
#12356 = VECTOR ( 'NONE', #38977, 1000.000000000000000 ) ;
#12357 = ADVANCED_FACE ( 'NONE', ( #10905 ), #21319, .F. ) ;
#12358 = AXIS2_PLACEMENT_3D ( 'NONE', #27092, #30525, #16062 ) ;
#12359 = PLANE ( 'NONE',  #14241 ) ;
#12360 = CARTESIAN_POINT ( 'NONE',  ( -48.47912675150885065, -183.6283474603465606, 6.938893903907228378E-15 ) ) ;
#12363 = VERTEX_POINT ( 'NONE', #32160 ) ;
#12362 = PLANE ( 'NONE',  #10677 ) ;
#12361 = CYLINDRICAL_SURFACE ( 'NONE', #14075, 15.00000000000000000 ) ;
#12364 = EDGE_CURVE ( 'NONE', #19780, #19801, #32660, .T. ) ;
#12365 = CARTESIAN_POINT ( 'NONE',  ( -48.88225018079680950, -193.5000000000000000, -0.9151456172430169067 ) ) ;
#12366 = EDGE_LOOP ( 'NONE', ( #15127, #47463, #5486, #7015 ) ) ;
#12367 = PLANE ( 'NONE',  #7109 ) ;
#12368 = LINE ( 'NONE', #24456, #15745 ) ;
#12369 = ORIENTED_EDGE ( 'NONE', *, *, #50286, .F. ) ;
#12370 = DIRECTION ( 'NONE',  ( 0.9564009842765202052, 0.000000000000000000, 0.2920567706369833760 ) ) ;
#12371 = FACE_OUTER_BOUND ( 'NONE', #21186, .T. ) ;
#12373 = CARTESIAN_POINT ( 'NONE',  ( -48.47912675150885065, -183.6283474603465606, 6.938893903907228378E-15 ) ) ;
#12372 = CARTESIAN_POINT ( 'NONE',  ( -48.47912675150885065, -175.3837268820161057, 6.938893903907228378E-15 ) ) ;
#12374 = ORIENTED_EDGE ( 'NONE', *, *, #27187, .T. ) ;
#12375 = CARTESIAN_POINT ( 'NONE',  ( -98.10897907742933910, -193.5000000000000000, 114.7252272087849434 ) ) ;
#12376 = VECTOR ( 'NONE', #50594, 1000.000000000000114 ) ;
#12377 = LINE ( 'NONE', #15831, #30358 ) ;
#12378 = AXIS2_PLACEMENT_3D ( 'NONE', #17317, #17578, #41204 ) ;
#12379 = DIRECTION ( 'NONE',  ( 0.9929810960135161402, 0.000000000000000000, 0.1182731709213730997 ) ) ;
#12380 = ORIENTED_EDGE ( 'NONE', *, *, #24644, .T. ) ;
#12381 = CARTESIAN_POINT ( 'NONE',  ( -339.1964088526558498, -84.08827740916061089, 45.24064679492014562 ) ) ;
#12382 = CARTESIAN_POINT ( 'NONE',  ( -336.3521761649654422, -113.6616659693417546, 59.18789727217205154 ) ) ;
#12383 = AXIS2_PLACEMENT_3D ( 'NONE', #21931, #13528, #21410 ) ;
#12384 = CARTESIAN_POINT ( 'NONE',  ( 0.000000000000000000, -167.6621341420952547, -39.12423683620669124 ) ) ;
#12385 = ORIENTED_EDGE ( 'NONE', *, *, #40701, .T. ) ;
#12386 = DIRECTION ( 'NONE',  ( 0.000000000000000000, 0.000000000000000000, 1.000000000000000000 ) ) ;
#12387 = DIRECTION ( 'NONE',  ( -0.000000000000000000, -0.6631226582407989678, -0.7485107481710977506 ) ) ;
#12388 = ORIENTED_EDGE ( 'NONE', *, *, #15985, .F. ) ;
#12389 = DIRECTION ( 'NONE',  ( -1.000000000000000000, 0.000000000000000000, 0.000000000000000000 ) ) ;
#12390 = VERTEX_POINT ( 'NONE', #8974 ) ;
#12391 = CIRCLE ( 'NONE', #41783, 15.00000000000000000 ) ;
#12392 = DIRECTION ( 'NONE',  ( -0.000000000000000000, 1.000000000000000000, 0.000000000000000000 ) ) ;
#12393 = PLANE ( 'NONE',  #47108 ) ;
#12394 = AXIS2_PLACEMENT_3D ( 'NONE', #26677, #2246, #2499 ) ;
#12395 = PLANE ( 'NONE',  #34459 ) ;
#12396 = CYLINDRICAL_SURFACE ( 'NONE', #35649, 125.0000000000000000 ) ;
#12397 = DIRECTION ( 'NONE',  ( 0.000000000000000000, 0.000000000000000000, 1.000000000000000000 ) ) ;
#12399 = VECTOR ( 'NONE', #21306, 1000.000000000000000 ) ;
#12398 = DIRECTION ( 'NONE',  ( 0.000000000000000000, 0.000000000000000000, -1.000000000000000000 ) ) ;
#12400 = CARTESIAN_POINT ( 'NONE',  ( -160.4991136281923900, -189.7472609257535510, 53.17445600718621534 ) ) ;
#12401 = DIRECTION ( 'NONE',  ( -1.000000000000000000, 0.000000000000000000, 0.000000000000000000 ) ) ;
#12403 = ORIENTED_EDGE ( 'NONE', *, *, #46073, .F. ) ;
#12402 = DIRECTION ( 'NONE',  ( 0.000000000000000000, -0.000000000000000000, -1.000000000000000000 ) ) ;
#12404 = VERTEX_POINT ( 'NONE', #5301 ) ;
#12405 = EDGE_CURVE ( 'NONE', #16314, #29108, #44419, .T. ) ;
#12406 = EDGE_CURVE ( 'NONE', #2342, #117, #17399, .T. ) ;
#12407 = CARTESIAN_POINT ( 'NONE',  ( -141.5426765053792622, -193.5000000000000000, 81.94739446021135620 ) ) ;
#12408 = CARTESIAN_POINT ( 'NONE',  ( 68.79964045138288498, -177.1207230881787780, 43.25148278810710423 ) ) ;
#12409 = ORIENTED_EDGE ( 'NONE', *, *, #22952, .T. ) ;
#12410 = VECTOR ( 'NONE', #2686, 1000.000000000000114 ) ;
#12411 = AXIS2_PLACEMENT_3D ( 'NONE', #1782, #22273, #41463 ) ;
#12412 = ORIENTED_EDGE ( 'NONE', *, *, #32403, .T. ) ;
#12413 = ORIENTED_EDGE ( 'NONE', *, *, #9568, .T. ) ;
#12414 = FACE_OUTER_BOUND ( 'NONE', #17285, .T. ) ;
#12415 = ADVANCED_FACE ( 'NONE', ( #1340 ), #9240, .T. ) ;
#12416 = AXIS2_PLACEMENT_3D ( 'NONE', #33510, #41900, #5917 ) ;
#12417 = EDGE_CURVE ( 'NONE', #34708, #2282, #17652, .T. ) ;
#12418 = CARTESIAN_POINT ( 'NONE',  ( -48.82732838694323618, -189.7472609257535510, -0.9374196611341184537 ) ) ;
#12419 = DIRECTION ( 'NONE',  ( -0.000000000000000000, 1.000000000000000000, -0.000000000000000000 ) ) ;
#12420 = VERTEX_POINT ( 'NONE', #37613 ) ;
#12421 = ORIENTED_EDGE ( 'NONE', *, *, #45281, .F. ) ;
#12422 = EDGE_CURVE ( 'NONE', #14384, #22837, #13180, .T. ) ;
#12423 = EDGE_LOOP ( 'NONE', ( #33888, #23106, #659, #45042 ) ) ;
#12424 = LINE ( 'NONE', #16123, #43434 ) ;
#12425 = DIRECTION ( 'NONE',  ( -0.000000000000000000, 1.000000000000000000, -0.000000000000000000 ) ) ;
#12426 = CIRCLE ( 'NONE', #22543, 125.0000000000000000 ) ;
#12428 = ORIENTED_EDGE ( 'NONE', *, *, #18830, .T. ) ;
#12427 = DIRECTION ( 'NONE',  ( 0.000000000000000000, -1.000000000000000000, 0.000000000000000000 ) ) ;
#12429 = EDGE_CURVE ( 'NONE', #37940, #4967, #15896, .T. ) ;
#12430 = CARTESIAN_POINT ( 'NONE',  ( -91.49662025983754177, -193.5000000000000000, -116.2991637277475405 ) ) ;
#12431 = DIRECTION ( 'NONE',  ( -0.000000000000000000, 1.000000000000000000, 0.000000000000000000 ) ) ;
#12432 = EDGE_LOOP ( 'NONE', ( #28015, #41305, #47065, #23922 ) ) ;
#12433 = PLANE ( 'NONE',  #43148 ) ;
#12434 = EDGE_CURVE ( 'NONE', #23911, #48950, #49184, .T. ) ;
#12435 = DIRECTION ( 'NONE',  ( 0.000000000000000000, 0.000000000000000000, -1.000000000000000000 ) ) ;
#12436 = CARTESIAN_POINT ( 'NONE',  ( -48.47912675150885065, -175.3837268820161057, 1.000000000000006883 ) ) ;
#12437 = CARTESIAN_POINT ( 'NONE',  ( -113.4314575050762102, -123.5000000000000284, -20.00000000000001066 ) ) ;
#12438 = ORIENTED_EDGE ( 'NONE', *, *, #30997, .F. ) ;
#12439 = ORIENTED_EDGE ( 'NONE', *, *, #25497, .F. ) ;
#12440 = EDGE_LOOP ( 'NONE', ( #38611, #34712, #35125, #1955 ) ) ;
#12441 = PLANE ( 'NONE',  #44967 ) ;
#12442 = CARTESIAN_POINT ( 'NONE',  ( -336.3521761649654422, -105.0395444947681369, -56.09938080879045685 ) ) ;
#12443 = ORIENTED_EDGE ( 'NONE', *, *, #49129, .F. ) ;
#12444 = DIRECTION ( 'NONE',  ( 0.000000000000000000, 0.000000000000000000, 1.000000000000000000 ) ) ;
#12445 = DIRECTION ( 'NONE',  ( 0.9842305779475954974, 0.000000000000000000, 0.1768902751225803205 ) ) ;
#12446 = VERTEX_POINT ( 'NONE', #99 ) ;
#12447 = DIRECTION ( 'NONE',  ( -0.6965510290629982615, 0.000000000000000000, 0.7175072570443298270 ) ) ;
#12448 = DIRECTION ( 'NONE',  ( 1.000000000000000000, -0.000000000000000000, -0.000000000000000000 ) ) ;
#12449 = ORIENTED_EDGE ( 'NONE', *, *, #26435, .T. ) ;
#12450 = PLANE ( 'NONE',  #13990 ) ;
#12451 = ORIENTED_EDGE ( 'NONE', *, *, #42216, .F. ) ;
#12452 = ADVANCED_FACE ( 'NONE', ( #49698 ), #43990, .F. ) ;
#12453 = AXIS2_PLACEMENT_3D ( 'NONE', #36363, #27960, #15633 ) ;
#12454 = VECTOR ( 'NONE', #18128, 1000.000000000000000 ) ;
#12455 = CARTESIAN_POINT ( 'NONE',  ( 70.91428087927182844, -193.5000000000000000, -33.48461921608518566 ) ) ;
#12456 = ORIENTED_EDGE ( 'NONE', *, *, #16409, .T. ) ;
#12457 = VECTOR ( 'NONE', #31821, 1000.000000000000000 ) ;
#12458 = CARTESIAN_POINT ( 'NONE',  ( -118.9967449635792462, -189.7472609257535510, -103.2098131075562009 ) ) ;
#12459 = DIRECTION ( 'NONE',  ( -0.000000000000000000, 1.000000000000000000, -0.000000000000000000 ) ) ;
#12460 = DIRECTION ( 'NONE',  ( -0.000000000000000000, 1.000000000000000000, -0.000000000000000000 ) ) ;
#12461 = CARTESIAN_POINT ( 'NONE',  ( -332.3517673607765914, -68.38646289696045244, -23.71704087764493707 ) ) ;
#12462 = VERTEX_POINT ( 'NONE', #5042 ) ;
#12463 = DIRECTION ( 'NONE',  ( -0.000000000000000000, 0.2393156642875652051, 0.9709418174260502354 ) ) ;
#12464 = EDGE_LOOP ( 'NONE', ( #43768, #2535, #17177, #43949 ) ) ;
#12465 = EDGE_CURVE ( 'NONE', #22595, #13288, #34354, .T. ) ;
#12466 = ORIENTED_EDGE ( 'NONE', *, *, #17663, .F. ) ;
#12467 = VECTOR ( 'NONE', #11196, 1000.000000000000000 ) ;
#12468 = CARTESIAN_POINT ( 'NONE',  ( -336.3521761649653854, -94.18160986457394301, 52.34913561719000086 ) ) ;
#12470 = VERTEX_POINT ( 'NONE', #1074 ) ;
#12469 = DIRECTION ( 'NONE',  ( 0.000000000000000000, -0.9927088740980553050, -0.1205366802553130001 ) ) ;
#12471 = EDGE_CURVE ( 'NONE', #47778, #50157, #18424, .T. ) ;
#12472 = ADVANCED_FACE ( 'NONE', ( #4060 ), #33135, .F. ) ;
#12473 = ORIENTED_EDGE ( 'NONE', *, *, #16284, .T. ) ;
#12474 = ADVANCED_FACE ( 'NONE', ( #36104 ), #16146, .T. ) ;
#12475 = DIRECTION ( 'NONE',  ( 0.6528221181905119463, 0.000000000000000000, 0.7575112421616284619 ) ) ;
#12476 = ADVANCED_FACE ( 'NONE', ( #37337 ), #41531, .T. ) ;
#12477 = ADVANCED_FACE ( 'NONE', ( #23764 ), #26803, .F. ) ;
#12478 = AXIS2_PLACEMENT_3D ( 'NONE', #39065, #3075, #43275 ) ;
#12479 = DIRECTION ( 'NONE',  ( 0.000000000000000000, 0.000000000000000000, -1.000000000000000000 ) ) ;
#12480 = CARTESIAN_POINT ( 'NONE',  ( 61.22907552172956969, -177.1207230881787780, -57.79541595648220920 ) ) ;
#12481 = VERTEX_POINT ( 'NONE', #34182 ) ;
#12482 = DIRECTION ( 'NONE',  ( 0.000000000000000000, 0.000000000000000000, -1.000000000000000000 ) ) ;
#12483 = ADVANCED_FACE ( 'NONE', ( #38631 ), #42307, .T. ) ;
#12484 = ORIENTED_EDGE ( 'NONE', *, *, #32333, .F. ) ;
#12485 = CARTESIAN_POINT ( 'NONE',  ( -47.50057025920934706, -175.3837268820161057, -0.2059786187410884151 ) ) ;
#12486 = CARTESIAN_POINT ( 'NONE',  ( -33.86391487983341619, -193.5000000000000000, 124.1426420773540542 ) ) ;
#12487 = EDGE_CURVE ( 'NONE', #51223, #10121, #2474, .T. ) ;
#12488 = LINE ( 'NONE', #36394, #25259 ) ;
#12489 = DIRECTION ( 'NONE',  ( 0.000000000000000000, 1.000000000000000000, -0.000000000000000000 ) ) ;
#12490 = ORIENTED_EDGE ( 'NONE', *, *, #35002, .F. ) ;
#12491 = ORIENTED_EDGE ( 'NONE', *, *, #31655, .T. ) ;
#12492 = EDGE_CURVE ( 'NONE', #42007, #31317, #30487, .T. ) ;
#12493 = VERTEX_POINT ( 'NONE', #1853 ) ;
#12494 = DIRECTION ( 'NONE',  ( 0.9646355819083614058, 0.000000000000000000, -0.2635871660690581320 ) ) ;
#12495 = LINE ( 'NONE', #13537, #15156 ) ;
#12496 = AXIS2_PLACEMENT_3D ( 'NONE', #48405, #11860, #12386 ) ;
#12497 = EDGE_CURVE ( 'NONE', #33568, #27241, #2633, .T. ) ;
#12498 = VECTOR ( 'NONE', #6025, 1000.000000000000000 ) ;
#12499 = CARTESIAN_POINT ( 'NONE',  ( -48.77118352214581876, -177.1207230881787780, -0.9564009842765195391 ) ) ;
#12500 = FACE_BOUND ( 'NONE', #12366, .T. ) ;
#12501 = FACE_OUTER_BOUND ( 'NONE', #8435, .T. ) ;
#12502 = EDGE_LOOP ( 'NONE', ( #12746, #41271, #37915, #38586 ) ) ;
#12503 = VECTOR ( 'NONE', #29419, 1000.000000000000000 ) ;
#12504 = ADVANCED_FACE ( 'NONE', ( #50482 ), #46795, .F. ) ;
#12505 = EDGE_CURVE ( 'NONE', #7989, #18995, #29979, .T. ) ;
#12506 = VERTEX_POINT ( 'NONE', #26543 ) ;
#12508 = ORIENTED_EDGE ( 'NONE', *, *, #37557, .F. ) ;
#12507 = CARTESIAN_POINT ( 'NONE',  ( 44.58442300236217903, -177.1207230881787780, -81.94739446021065987 ) ) ;
#12509 = CIRCLE ( 'NONE', #37690, 125.0000000000000000 ) ;
#12510 = CARTESIAN_POINT ( 'NONE',  ( 11.66870402553033692, -193.5000000000000000, 108.4360005853211248 ) ) ;
#12511 = ORIENTED_EDGE ( 'NONE', *, *, #50094, .T. ) ;
#12512 = CARTESIAN_POINT ( 'NONE',  ( -41.30311180514221547, -189.7472609257535510, 123.7921848946937899 ) ) ;
#12513 = DIRECTION ( 'NONE',  ( 0.000000000000000000, 1.156482317317871232E-16, 1.000000000000000000 ) ) ;
#12514 = CARTESIAN_POINT ( 'NONE',  ( -148.6149069237406195, -183.6283474603465606, -74.81861753132355375 ) ) ;
#12515 = CARTESIAN_POINT ( 'NONE',  ( -339.1964088526558498, -64.50000000000000000, 0.4999999999999543698 ) ) ;
#12516 = EDGE_LOOP ( 'NONE', ( #23569, #7702, #7399, #32912 ) ) ;
#12517 = DIRECTION ( 'NONE',  ( 0.000000000000000000, 0.000000000000000000, 1.000000000000000000 ) ) ;
#12518 = ORIENTED_EDGE ( 'NONE', *, *, #37514, .T. ) ;
#12519 = ADVANCED_FACE ( 'NONE', ( #42581 ), #46032, .T. ) ;
#12520 = VECTOR ( 'NONE', #30100, 1000.000000000000000 ) ;
#12521 = EDGE_CURVE ( 'NONE', #33429, #36752, #6597, .T. ) ;
#12522 = EDGE_LOOP ( 'NONE', ( #7538, #21794, #21935, #31912 ) ) ;
#12523 = CARTESIAN_POINT ( 'NONE',  ( -47.66663987350317200, -177.1207230881787780, -0.5829794791144634614 ) ) ;
#12524 = DIRECTION ( 'NONE',  ( -0.000000000000000000, 0.9350162426854146114, -0.3546048870425363986 ) ) ;
#12525 = DIRECTION ( 'NONE',  ( 0.000000000000000000, 0.000000000000000000, 1.000000000000000000 ) ) ;
#12526 = DIRECTION ( 'NONE',  ( 0.000000000000000000, -1.000000000000000000, 0.000000000000000000 ) ) ;
#12527 = DIRECTION ( 'NONE',  ( 0.000000000000000000, 0.000000000000000000, 1.000000000000000000 ) ) ;
#12528 = DIRECTION ( 'NONE',  ( -0.05924062789370006937, 0.000000000000000000, -0.9982437317643222396 ) ) ;
#12529 = ORIENTED_EDGE ( 'NONE', *, *, #26739, .F. ) ;
#12530 = CARTESIAN_POINT ( 'NONE',  ( -339.1964088526558498, -172.5932850007654054, 34.49419324804723175 ) ) ;
#12531 = DIRECTION ( 'NONE',  ( 0.000000000000000000, -0.9709418174260535661, -0.2393156642875516327 ) ) ;
#12532 = DIRECTION ( 'NONE',  ( 0.000000000000000000, 0.000000000000000000, 1.000000000000000000 ) ) ;
#12533 = FACE_BOUND ( 'NONE', #51906, .T. ) ;
#12534 = ORIENTED_EDGE ( 'NONE', *, *, #48332, .F. ) ;
#12535 = VECTOR ( 'NONE', #48235, 1000.000000000000000 ) ;
#12536 = CYLINDRICAL_SURFACE ( 'NONE', #8828, 125.0000000000000000 ) ;
#12537 = EDGE_LOOP ( 'NONE', ( #14146, #9395, #37843, #27791, #46630 ) ) ;
#12538 = AXIS2_PLACEMENT_3D ( 'NONE', #16453, #48525, #677 ) ;
#12539 = CARTESIAN_POINT ( 'NONE',  ( -108.4791267515088435, -132.5479369270331915, -60.00000000000002842 ) ) ;
#12540 = EDGE_CURVE ( 'NONE', #32868, #41179, #38378, .T. ) ;
#12541 = EDGE_CURVE ( 'NONE', #48639, #50010, #33537, .T. ) ;
#12542 = FACE_OUTER_BOUND ( 'NONE', #31048, .T. ) ;
#12543 = ORIENTED_EDGE ( 'NONE', *, *, #2754, .F. ) ;
#12544 = ADVANCED_FACE ( 'NONE', ( #14729 ), #18157, .F. ) ;
#12545 = EDGE_CURVE ( 'NONE', #23080, #20926, #26035, .T. ) ;
#12546 = CARTESIAN_POINT ( 'NONE',  ( -332.3517673607765914, -154.8494888031386836, 50.05135858667791382 ) ) ;
#12547 = DIRECTION ( 'NONE',  ( 0.000000000000000000, -0.000000000000000000, -1.000000000000000000 ) ) ;
#12549 = ORIENTED_EDGE ( 'NONE', *, *, #46337, .T. ) ;
#12548 = CARTESIAN_POINT ( 'NONE',  ( -336.3521761649654422, -107.7955183043589500, 56.89493493766750731 ) ) ;
#12550 = LINE ( 'NONE', #730, #47059 ) ;
#12551 = ORIENTED_EDGE ( 'NONE', *, *, #2656, .T. ) ;
#12552 = VECTOR ( 'NONE', #33764, 1000.000000000000114 ) ;
#12553 = ORIENTED_EDGE ( 'NONE', *, *, #13436, .F. ) ;
#12554 = APPLICATION_CONTEXT ( 'automotive_design' ) ;
#12555 = DIRECTION ( 'NONE',  ( -0.8455960035018311727, 0.000000000000000000, 0.5338233779647826305 ) ) ;
#12556 = VERTEX_POINT ( 'NONE', #22090 ) ;
#12557 = PRODUCT_RELATED_PRODUCT_CATEGORY ( 'part', '', ( #5888 ) ) ;
#12558 = LINE ( 'NONE', #21228, #2422 ) ;
#12559 = DIRECTION ( 'NONE',  ( 1.000000000000000000, -0.000000000000000000, 0.000000000000000000 ) ) ;
#12560 = FACE_OUTER_BOUND ( 'NONE', #22254, .T. ) ;
#12561 = EDGE_CURVE ( 'NONE', #25331, #17110, #14477, .T. ) ;
#12562 = CARTESIAN_POINT ( 'NONE',  ( -260.0000000000000000, -63.50000000000000000, 60.00000000000000711 ) ) ;
#12563 = PLANE ( 'NONE',  #32315 ) ;
#12564 = VERTEX_POINT ( 'NONE', #981 ) ;
#12567 = ORIENTED_EDGE ( 'NONE', *, *, #25001, .F. ) ;
#12566 = DIRECTION ( 'NONE',  ( 0.000000000000000000, -9.251858538542971828E-16, -1.000000000000000000 ) ) ;
#12565 = LINE ( 'NONE', #13084, #19791 ) ;
#12568 = VERTEX_POINT ( 'NONE', #37250 ) ;
#12569 = CARTESIAN_POINT ( 'NONE',  ( -339.1964088526558498, -144.3080463282014136, 56.27632902032101470 ) ) ;
#12570 = EDGE_LOOP ( 'NONE', ( #11178, #18865, #23848, #39702 ) ) ;
#12571 = LINE ( 'NONE', #20986, #2111 ) ;
#12572 = ORIENTED_EDGE ( 'NONE', *, *, #42962, .T. ) ;
#12573 = DIRECTION ( 'NONE',  ( -0.9720229140804107493, 0.000000000000000000, -0.2348860457809842095 ) ) ;
#12574 = CARTESIAN_POINT ( 'NONE',  ( -171.9838957966129556, -193.5000000000000000, 19.27620354518722579 ) ) ;
#12575 = EDGE_LOOP ( 'NONE', ( #22398, #13459, #40204, #44509 ) ) ;
#12577 = CARTESIAN_POINT ( 'NONE',  ( -170.2790847791494855, -183.6283474603465606, -28.10285082451570915 ) ) ;
#12576 = CARTESIAN_POINT ( 'NONE',  ( -336.3521761649654422, -176.9651911376907094, -25.08789112700655721 ) ) ;
#12578 = EDGE_LOOP ( 'NONE', ( #406, #7316, #21211, #10934 ) ) ;
#12579 = EDGE_LOOP ( 'NONE', ( #13155, #3317, #31925, #13503 ) ) ;
#12580 = DIRECTION ( 'NONE',  ( 0.000000000000000000, 0.000000000000000000, 1.000000000000000000 ) ) ;
#12581 = CARTESIAN_POINT ( 'NONE',  ( -330.4913330509368166, -84.75001853787871653, -44.49369547121542467 ) ) ;
#12582 = DIRECTION ( 'NONE',  ( 0.000000000000000000, -0.4647231720437573488, 0.8854560256532157947 ) ) ;
#12583 = DIRECTION ( 'NONE',  ( -0.9785564922995017012, 0.000000000000000000, -0.2059786187411094538 ) ) ;
#12584 = DIRECTION ( 'NONE',  ( 0.000000000000000000, 0.000000000000000000, 1.000000000000000000 ) ) ;
#12585 = CARTESIAN_POINT ( 'NONE',  ( -167.9436818089035057, -177.1207230881787780, 36.78613984830044359 ) ) ;
#12586 = CARTESIAN_POINT ( 'NONE',  ( -163.3872488209693756, -183.6283474603465606, -49.20491319441543254 ) ) ;
#12587 = LINE ( 'NONE', #4198, #15411 ) ;
#12588 = DIRECTION ( 'NONE',  ( -0.9785564922995017012, 0.000000000000000000, -0.2059786187411094538 ) ) ;
#12589 = AXIS2_PLACEMENT_3D ( 'NONE', #24841, #40862, #37441 ) ;
#12590 = VECTOR ( 'NONE', #14558, 1000.000000000000114 ) ;
#12591 = CARTESIAN_POINT ( 'NONE',  ( -305.0000000000000568, -137.3729703655840524, -58.37414404713467064 ) ) ;
#12592 = EDGE_LOOP ( 'NONE', ( #50550, #27693, #8744, #39271 ) ) ;
#12593 = ORIENTED_EDGE ( 'NONE', *, *, #31408, .F. ) ;
#12594 = DIRECTION ( 'NONE',  ( -0.000000000000000000, 1.000000000000000000, 0.000000000000000000 ) ) ;
#12595 = CARTESIAN_POINT ( 'NONE',  ( -77.67449977936063021, -175.3837268820161057, -121.5427093402339267 ) ) ;
#12596 = FACE_OUTER_BOUND ( 'NONE', #21113, .T. ) ;
#12597 = ORIENTED_EDGE ( 'NONE', *, *, #49778, .F. ) ;
#12598 = EDGE_CURVE ( 'NONE', #17248, #24620, #33570, .T. ) ;
#12599 = ORIENTED_EDGE ( 'NONE', *, *, #24643, .T. ) ;
#12600 = ORIENTED_EDGE ( 'NONE', *, *, #43645, .T. ) ;
#12601 = DIRECTION ( 'NONE',  ( 0.000000000000000000, -0.000000000000000000, -1.000000000000000000 ) ) ;
#12602 = CIRCLE ( 'NONE', #42841, 125.0000000000000000 ) ;
#12603 = DIRECTION ( 'NONE',  ( -0.000000000000000000, 1.000000000000000000, 0.000000000000000000 ) ) ;
#12604 = CARTESIAN_POINT ( 'NONE',  ( -99.02518858244150124, -193.5000000000000000, 114.3245189510261497 ) ) ;
#12605 = CARTESIAN_POINT ( 'NONE',  ( -330.4913330509368166, -71.02573290043841325, 26.97593913775512320 ) ) ;
#12606 = ORIENTED_EDGE ( 'NONE', *, *, #22182, .F. ) ;
#12607 = CARTESIAN_POINT ( 'NONE',  ( 0.000000000000000000, -84.37576316379318087, -44.16213414209506283 ) ) ;
#12608 = DIRECTION ( 'NONE',  ( -1.000000000000000000, -0.000000000000000000, 0.000000000000000000 ) ) ;
#12609 = ORIENTED_EDGE ( 'NONE', *, *, #49547, .T. ) ;
#12610 = CARTESIAN_POINT ( 'NONE',  ( -152.3176060415594861, -177.1207230881787780, -69.58857822034967455 ) ) ;
#12611 = ORIENTED_EDGE ( 'NONE', *, *, #44601, .T. ) ;
#12612 = ORIENTED_EDGE ( 'NONE', *, *, #49412, .F. ) ;
#12613 = EDGE_CURVE ( 'NONE', #48065, #17157, #36989, .T. ) ;
#12614 = FACE_OUTER_BOUND ( 'NONE', #51166, .T. ) ;
#12615 = VECTOR ( 'NONE', #16876, 1000.000000000000000 ) ;
#12616 = DIRECTION ( 'NONE',  ( 0.9960498426152177842, 0.000000000000000000, -0.08879589532292482545 ) ) ;
#12617 = CARTESIAN_POINT ( 'NONE',  ( 75.04604393171729271, -175.3837268820161057, -10.84123789944573701 ) ) ;
#12620 = ORIENTED_EDGE ( 'NONE', *, *, #13599, .T. ) ;
#12619 = DIRECTION ( 'NONE',  ( 1.000000000000000000, -0.000000000000000000, -0.000000000000000000 ) ) ;
#12618 = DIRECTION ( 'NONE',  ( 0.000000000000000000, -0.9927088740980526405, 0.1205366802553337890 ) ) ;
#12621 = CARTESIAN_POINT ( 'NONE',  ( -336.3521761649653854, -158.9146170832377720, -48.43351006119259949 ) ) ;
#12622 = ORIENTED_EDGE ( 'NONE', *, *, #37934, .F. ) ;
#12623 = PLANE ( 'NONE',  #29750 ) ;
#12624 = CARTESIAN_POINT ( 'NONE',  ( -330.4913330509368166, -143.9541802141664562, 55.34326076196094135 ) ) ;
#12625 = VERTEX_POINT ( 'NONE', #17288 ) ;
#12626 = CARTESIAN_POINT ( 'NONE',  ( -140.1460956102404509, -193.5000000000000000, 84.98333260264821831 ) ) ;
#12627 = EDGE_CURVE ( 'NONE', #37301, #25289, #9921, .T. ) ;
#12628 = CARTESIAN_POINT ( 'NONE',  ( 54.46899307705341187, -183.6283474603465606, -70.89911581792812001 ) ) ;
#12630 = CARTESIAN_POINT ( 'NONE',  ( 30.50828161901818092, -183.6283474603465606, 96.88131563365348597 ) ) ;
#12629 = CARTESIAN_POINT ( 'NONE',  ( -336.3521761649654422, -123.5000000000000284, 0.000000000000000000 ) ) ;
#12631 = EDGE_LOOP ( 'NONE', ( #24281, #48634, #7564, #33691 ) ) ;
#12632 = CARTESIAN_POINT ( 'NONE',  ( -332.3517673607765914, -141.9604555052315220, 56.09938080879057765 ) ) ;
#12633 = CARTESIAN_POINT ( 'NONE',  ( 62.13187335169531167, -193.5000000000000000, -58.22548115875872554 ) ) ;
#12635 = AXIS2_PLACEMENT_3D ( 'NONE', #15413, #18566, #26709 ) ;
#12634 = DIRECTION ( 'NONE',  ( 0.000000000000000000, 0.000000000000000000, -1.000000000000000000 ) ) ;
#12636 = ORIENTED_EDGE ( 'NONE', *, *, #11391, .F. ) ;
#12637 = LINE ( 'NONE', #8973, #15731 ) ;
#12638 = CARTESIAN_POINT ( 'NONE',  ( -47.78257572244585560, -189.7472609257535510, -0.7175072570443230546 ) ) ;
#12639 = PLANE ( 'NONE',  #24019 ) ;
#12640 = ORIENTED_EDGE ( 'NONE', *, *, #7353, .T. ) ;
#12641 = DIRECTION ( 'NONE',  ( 0.000000000000000000, 0.000000000000000000, -1.000000000000000000 ) ) ;
#12642 = EDGE_CURVE ( 'NONE', #22860, #48670, #21225, .T. ) ;
#12643 = VERTEX_POINT ( 'NONE', #4949 ) ;
#12644 = CARTESIAN_POINT ( 'NONE',  ( 18.00181100848376303, -177.1207230881787780, -105.8550183720733742 ) ) ;
#12645 = EDGE_LOOP ( 'NONE', ( #5693, #46324, #10076, #30400 ) ) ;
#12646 = DIRECTION ( 'NONE',  ( -0.000000000000000000, -0.1205366802553164696, 0.9927088740980548609 ) ) ;
#12647 = CARTESIAN_POINT ( 'NONE',  ( -59.86929868745817629, -183.6283474603465606, -124.4799742258549458 ) ) ;
#12648 = CIRCLE ( 'NONE', #86, 125.0000000000000000 ) ;
#12649 = DIRECTION ( 'NONE',  ( -1.000000000000000000, 0.000000000000000000, 0.000000000000000000 ) ) ;
#12650 = DIRECTION ( 'NONE',  ( 0.000000000000000000, -4.394632805807911569E-15, -1.000000000000000000 ) ) ;
#12651 = DIRECTION ( 'NONE',  ( 0.9720229140804123036, 0.000000000000000000, -0.2348860457809775759 ) ) ;
#12652 = EDGE_CURVE ( 'NONE', #31272, #40382, #1235, .T. ) ;
#12653 = EDGE_CURVE ( 'NONE', #7505, #6993, #37507, .T. ) ;
#12654 = CIRCLE ( 'NONE', #47076, 60.00000000000000000 ) ;
#12655 = LINE ( 'NONE', #45001, #8666 ) ;
#12656 = EDGE_CURVE ( 'NONE', #25190, #38286, #16781, .T. ) ;
#12657 = DIRECTION ( 'NONE',  ( -0.000000000000000000, 0.9709418174260553425, 0.2393156642875449158 ) ) ;
#12658 = DIRECTION ( 'NONE',  ( 0.000000000000000000, 0.4647231720437695057, 0.8854560256532093554 ) ) ;
#12660 = VERTEX_POINT ( 'NONE', #49605 ) ;
#12659 = DIRECTION ( 'NONE',  ( 0.000000000000000000, -1.000000000000000000, 0.000000000000000000 ) ) ;
#12661 = VERTEX_POINT ( 'NONE', #45936 ) ;
#12662 = DIRECTION ( 'NONE',  ( -0.000000000000000000, 1.000000000000000000, -0.000000000000000000 ) ) ;
#12663 = CARTESIAN_POINT ( 'NONE',  ( -26.20043062753591201, -189.7472609257535510, -122.9986166548862911 ) ) ;
#12664 = ORIENTED_EDGE ( 'NONE', *, *, #12235, .T. ) ;
#12665 = VERTEX_POINT ( 'NONE', #49863 ) ;
#12666 = VECTOR ( 'NONE', #31938, 1000.000000000000000 ) ;
#12667 = VERTEX_POINT ( 'NONE', #49354 ) ;
#12668 = EDGE_CURVE ( 'NONE', #32981, #23734, #5206, .T. ) ;
#12669 = DIRECTION ( 'NONE',  ( -0.5586467658036415873, 0.000000000000000000, -0.8294056854502090959 ) ) ;
#12670 = DIRECTION ( 'NONE',  ( 0.000000000000000000, 1.000000000000000000, 0.000000000000000000 ) ) ;
#12671 = CARTESIAN_POINT ( 'NONE',  ( 49.10711742958949344, -193.5000000000000000, 78.11481899503480975 ) ) ;
#12672 = ORIENTED_EDGE ( 'NONE', *, *, #43872, .F. ) ;
#12673 = EDGE_CURVE ( 'NONE', #26290, #16305, #43616, .T. ) ;
#12674 = ORIENTED_EDGE ( 'NONE', *, *, #27243, .T. ) ;
#12675 = LINE ( 'NONE', #8737, #2322 ) ;
#12676 = DIRECTION ( 'NONE',  ( 0.9960498426152177842, 0.000000000000000000, -0.08879589532292482545 ) ) ;
#12678 = ORIENTED_EDGE ( 'NONE', *, *, #155, .T. ) ;
#12677 = CARTESIAN_POINT ( 'NONE',  ( -47.60339180931321579, -193.5000000000000000, 0.4827922027307559594 ) ) ;
#12679 = LINE ( 'NONE', #28451, #39597 ) ;
#12680 = CARTESIAN_POINT ( 'NONE',  ( -31.30262293407085039, -183.6283474603465606, -123.8142468240611294 ) ) ;
#12681 = VERTEX_POINT ( 'NONE', #29357 ) ;
#12682 = PLANE ( 'NONE',  #38939 ) ;
#12683 = AXIS2_PLACEMENT_3D ( 'NONE', #27459, #39293, #43747 ) ;
#12684 = VERTEX_POINT ( 'NONE', #25172 ) ;
#12685 = CARTESIAN_POINT ( 'NONE',  ( -48.13092511607445090, -177.1207230881787780, -0.9374196611341135688 ) ) ;
#12686 = LINE ( 'NONE', #13228, #3665 ) ;
#12687 = DIRECTION ( 'NONE',  ( -0.5085311186492273983, 0.000000000000000000, 0.8610436117673514467 ) ) ;
#12688 = ORIENTED_EDGE ( 'NONE', *, *, #4473, .T. ) ;
#12689 = EDGE_LOOP ( 'NONE', ( #329, #41353, #46147, #4498 ) ) ;
#12690 = LINE ( 'NONE', #349, #43254 ) ;
#12691 = FACE_OUTER_BOUND ( 'NONE', #18022, .T. ) ;
#12692 = EDGE_LOOP ( 'NONE', ( #35246, #28567, #24664, #11000 ) ) ;
#12693 = CARTESIAN_POINT ( 'NONE',  ( -26.20043062753592977, -175.3837268820161057, -122.9986166548863196 ) ) ;
#12694 = CARTESIAN_POINT ( 'NONE',  ( -156.7610986364826999, -193.5000000000000000, -62.45009659481510766 ) ) ;
#12695 = EDGE_CURVE ( 'NONE', #28854, #37405, #48834, .T. ) ;
#12696 = EDGE_CURVE ( 'NONE', #34751, #33745, #41182, .T. ) ;
#12697 = ORIENTED_EDGE ( 'NONE', *, *, #48895, .T. ) ;
#12698 = LINE ( 'NONE', #24288, #46882 ) ;
#12699 = VECTOR ( 'NONE', #8782, 1000.000000000000000 ) ;
#12700 = LINE ( 'NONE', #37670, #6320 ) ;
#12701 = ORIENTED_EDGE ( 'NONE', *, *, #6275, .F. ) ;
#12702 = DIRECTION ( 'NONE',  ( -0.2348860457809911206, 0.000000000000000000, 0.9720229140804089729 ) ) ;
#12703 = ORIENTED_EDGE ( 'NONE', *, *, #23468, .F. ) ;
#12704 = VECTOR ( 'NONE', #46634, 1000.000000000000114 ) ;
#12705 = PLANE ( 'NONE',  #13597 ) ;
#12706 = VERTEX_POINT ( 'NONE', #9398 ) ;
#12707 = CARTESIAN_POINT ( 'NONE',  ( -48.47912675150885065, -177.1207230881787780, 6.938893903907228378E-15 ) ) ;
#12708 = PLANE ( 'NONE',  #43189 ) ;
#12709 = DIRECTION ( 'NONE',  ( 0.000000000000000000, 0.000000000000000000, 1.000000000000000000 ) ) ;
#12710 = ADVANCED_FACE ( 'NONE', ( #33042 ), #41711, .T. ) ;
#12711 = CARTESIAN_POINT ( 'NONE',  ( -167.9436818089035057, -177.1207230881787780, 36.78613984830044359 ) ) ;
#12712 = EDGE_CURVE ( 'NONE', #11444, #28167, #1762, .T. ) ;
#12713 = VERTEX_POINT ( 'NONE', #41442 ) ;
#12714 = CARTESIAN_POINT ( 'NONE',  ( -47.47956591500005885, -177.1207230881787780, 0.02963332782257025594 ) ) ;
#12715 = ORIENTED_EDGE ( 'NONE', *, *, #12234, .F. ) ;
#12716 = ORIENTED_EDGE ( 'NONE', *, *, #13516, .T. ) ;
#12717 = EDGE_CURVE ( 'NONE', #12625, #34416, #20967, .T. ) ;
#12718 = DIRECTION ( 'NONE',  ( -0.000000000000000000, 1.000000000000000000, 0.000000000000000000 ) ) ;
#12720 = ORIENTED_EDGE ( 'NONE', *, *, #8357, .F. ) ;
#12719 = DIRECTION ( 'NONE',  ( 0.000000000000000000, 0.000000000000000000, 1.000000000000000000 ) ) ;
#12721 = VECTOR ( 'NONE', #47627, 1000.000000000000227 ) ;
#12722 = EDGE_CURVE ( 'NONE', #13819, #48760, #29613, .T. ) ;
#12723 = EDGE_LOOP ( 'NONE', ( #33996, #4481, #14501, #43674 ) ) ;
#12724 = DIRECTION ( 'NONE',  ( 0.000000000000000000, 0.000000000000000000, -1.000000000000000000 ) ) ;
#12725 = AXIS2_PLACEMENT_3D ( 'NONE', #39285, #11155, #4070 ) ;
#12726 = VECTOR ( 'NONE', #39722, 1000.000000000000000 ) ;
#12727 = DIRECTION ( 'NONE',  ( 0.6528221181905280446, 0.000000000000000000, -0.7575112421616145841 ) ) ;
#12728 = ORIENTED_EDGE ( 'NONE', *, *, #44591, .F. ) ;
#12729 = FACE_OUTER_BOUND ( 'NONE', #51482, .T. ) ;
#12730 = ORIENTED_EDGE ( 'NONE', *, *, #39465, .T. ) ;
#12731 = DIRECTION ( 'NONE',  ( -1.000000000000000000, 0.000000000000000000, 0.000000000000000000 ) ) ;
#12732 = FACE_OUTER_BOUND ( 'NONE', #14530, .T. ) ;
#12733 = CARTESIAN_POINT ( 'NONE',  ( -339.1964088526558498, -162.2499814621209850, 44.49369547121574442 ) ) ;
#12734 = PLANE ( 'NONE',  #21577 ) ;
#12735 = VERTEX_POINT ( 'NONE', #45666 ) ;
#12736 = CIRCLE ( 'NONE', #3517, 125.0000000000000000 ) ;
#12737 = ORIENTED_EDGE ( 'NONE', *, *, #33827, .T. ) ;
#12738 = VERTEX_POINT ( 'NONE', #40926 ) ;
#12739 = CARTESIAN_POINT ( 'NONE',  ( -330.4913330509368166, -74.65991953890876687, -33.10432812419148263 ) ) ;
#12740 = LINE ( 'NONE', #8805, #46152 ) ;
#12741 = VECTOR ( 'NONE', #42755, 1000.000000000000114 ) ;
#12742 = CARTESIAN_POINT ( 'NONE',  ( -121.5885020763900997, -193.5000000000000000, -101.3904297239420913 ) ) ;
#12743 = FACE_BOUND ( 'NONE', #43955, .T. ) ;
#12744 = FACE_OUTER_BOUND ( 'NONE', #47664, .T. ) ;
#12745 = EDGE_LOOP ( 'NONE', ( #49237, #13668, #30713, #40875 ) ) ;
#12746 = ORIENTED_EDGE ( 'NONE', *, *, #34547, .T. ) ;
#12748 = EDGE_LOOP ( 'NONE', ( #33201, #50401, #45219, #25902 ) ) ;
#12747 = LINE ( 'NONE', #36409, #13032 ) ;
#12749 = ORIENTED_EDGE ( 'NONE', *, *, #34509, .T. ) ;
#12750 = DIRECTION ( 'NONE',  ( 0.000000000000000000, 0.000000000000000000, -1.000000000000000000 ) ) ;
#12751 = ADVANCED_FACE ( 'NONE', ( #9650 ), #25678, .F. ) ;
#12752 = LINE ( 'NONE', #692, #9039 ) ;
#12753 = CIRCLE ( 'NONE', #9403, 124.9999999999999858 ) ;
#12754 = EDGE_CURVE ( 'NONE', #2898, #50750, #42753, .T. ) ;
#12755 = DIRECTION ( 'NONE',  ( -1.000000000000000000, 0.000000000000000000, -0.000000000000000000 ) ) ;
#12756 = EDGE_CURVE ( 'NONE', #33118, #42260, #38787, .T. ) ;
#12757 = EDGE_CURVE ( 'NONE', #28909, #20222, #22778, .T. ) ;
#12758 = DIRECTION ( 'NONE',  ( 0.000000000000000000, 0.000000000000000000, -1.000000000000000000 ) ) ;
#12759 = ORIENTED_EDGE ( 'NONE', *, *, #1594, .T. ) ;
#12760 = LINE ( 'NONE', #19884, #33415 ) ;
#12761 = EDGE_LOOP ( 'NONE', ( #45379, #18813, #44950, #2695 ) ) ;
#12762 = EDGE_CURVE ( 'NONE', #8786, #51399, #39043, .T. ) ;
#12763 = ORIENTED_EDGE ( 'NONE', *, *, #17676, .F. ) ;
#12764 = DIRECTION ( 'NONE',  ( 0.000000000000000000, 0.000000000000000000, 1.000000000000000000 ) ) ;
#12765 = EDGE_CURVE ( 'NONE', #20806, #2378, #42479, .T. ) ;
#12766 = CARTESIAN_POINT ( 'NONE',  ( 22.03849146056077757, -189.7472609257535510, 103.2098131075567409 ) ) ;
#12767 = DIRECTION ( 'NONE',  ( 0.000000000000000000, -1.000000000000000000, 0.000000000000000000 ) ) ;
#12768 = PLANE ( 'NONE',  #47433 ) ;
#12769 = FACE_OUTER_BOUND ( 'NONE', #31155, .T. ) ;
#12770 = FACE_OUTER_BOUND ( 'NONE', #39583, .T. ) ;
#12771 = DIRECTION ( 'NONE',  ( 0.9960498426152171181, 0.000000000000000000, -0.08879589532293157006 ) ) ;
#12772 = ADVANCED_FACE ( 'NONE', ( #43001 ), #46186, .T. ) ;
#12773 = ORIENTED_EDGE ( 'NONE', *, *, #33684, .F. ) ;
#12774 = DIRECTION ( 'NONE',  ( 0.8124868780056825335, 0.000000000000000000, -0.5829794791144703447 ) ) ;
#12775 = DIRECTION ( 'NONE',  ( 0.000000000000000000, 0.000000000000000000, -1.000000000000000000 ) ) ;
#12776 = AXIS2_PLACEMENT_3D ( 'NONE', #35227, #7121, #11303 ) ;
#12777 = VECTOR ( 'NONE', #6960, 1000.000000000000000 ) ;
#12778 = EDGE_CURVE ( 'NONE', #5079, #32692, #22531, .T. ) ;
#12779 = CARTESIAN_POINT ( 'NONE',  ( -330.4913330509368166, -71.02573290043841325, 26.97593913775512320 ) ) ;
#12780 = FACE_BOUND ( 'NONE', #36818, .T. ) ;
#12781 = ORIENTED_EDGE ( 'NONE', *, *, #27566, .T. ) ;
#12782 = VECTOR ( 'NONE', #42516, 1000.000000000000000 ) ;
#12783 = AXIS2_PLACEMENT_3D ( 'NONE', #2997, #19039, #35065 ) ;
#12784 = EDGE_CURVE ( 'NONE', #49515, #14469, #34585, .T. ) ;
#12785 = LINE ( 'NONE', #28553, #18035 ) ;
#12786 = ORIENTED_EDGE ( 'NONE', *, *, #5598, .T. ) ;
#12787 = DIRECTION ( 'NONE',  ( 0.000000000000000000, -0.1205366802553268640, -0.9927088740980535286 ) ) ;
#12788 = EDGE_CURVE ( 'NONE', #45115, #27547, #34348, .T. ) ;
#12789 = ORIENTED_EDGE ( 'NONE', *, *, #26891, .F. ) ;
#12790 = DIRECTION ( 'NONE',  ( 0.000000000000000000, 0.000000000000000000, 1.000000000000000000 ) ) ;
#12791 = ORIENTED_EDGE ( 'NONE', *, *, #38812, .T. ) ;
#12792 = ADVANCED_FACE ( 'NONE', ( #50904 ), #14909, .F. ) ;
#12793 = PLANE ( 'NONE',  #14236 ) ;
#12794 = DIRECTION ( 'NONE',  ( 0.000000000000000000, -1.119474883163699554E-13, -1.000000000000000000 ) ) ;
#12796 = ORIENTED_EDGE ( 'NONE', *, *, #1569, .F. ) ;
#12795 = LINE ( 'NONE', #974, #47243 ) ;
#12797 = AXIS2_PLACEMENT_3D ( 'NONE', #20730, #1539, #17321 ) ;
#12798 = DIRECTION ( 'NONE',  ( 0.000000000000000000, 0.000000000000000000, -1.000000000000000000 ) ) ;
#12799 = EDGE_CURVE ( 'NONE', #37529, #30910, #1685, .T. ) ;
#12800 = ORIENTED_EDGE ( 'NONE', *, *, #41967, .F. ) ;
#12801 = AXIS2_PLACEMENT_3D ( 'NONE', #25279, #33437, #1360 ) ;
#12802 = ORIENTED_EDGE ( 'NONE', *, *, #240, .T. ) ;
#12803 = LINE ( 'NONE', #8867, #24219 ) ;
#12804 = CARTESIAN_POINT ( 'NONE',  ( 21.21056010634072564, -175.3837268820161057, 103.7706487676302061 ) ) ;
#12805 = ORIENTED_EDGE ( 'NONE', *, *, #29740, .T. ) ;
#12806 = CARTESIAN_POINT ( 'NONE',  ( 52.59568867645218404, -193.5000000000000000, -73.54509967498589162 ) ) ;
#12807 = FACE_OUTER_BOUND ( 'NONE', #21427, .T. ) ;
#12808 = PLANE ( 'NONE',  #9563 ) ;
#12809 = VECTOR ( 'NONE', #51468, 1000.000000000000227 ) ;
#12810 = DIRECTION ( 'NONE',  ( 1.000000000000000000, -0.000000000000000000, -0.000000000000000000 ) ) ;
#12811 = EDGE_CURVE ( 'NONE', #33588, #7429, #50349, .T. ) ;
#12812 = LINE ( 'NONE', #35964, #34021 ) ;
#12813 = ORIENTED_EDGE ( 'NONE', *, *, #28568, .T. ) ;
#12816 = ORIENTED_EDGE ( 'NONE', *, *, #49475, .T. ) ;
#12815 = FACE_OUTER_BOUND ( 'NONE', #43784, .T. ) ;
#12814 = CARTESIAN_POINT ( 'NONE',  ( 74.80070215680143519, -183.6283474603465606, 13.35228579481199596 ) ) ;
#12817 = VECTOR ( 'NONE', #4588, 1000.000000000000227 ) ;
#12818 = CIRCLE ( 'NONE', #8621, 125.0000000000000000 ) ;
#12819 = ORIENTED_EDGE ( 'NONE', *, *, #21208, .T. ) ;
#12820 = DIRECTION ( 'NONE',  ( -0.000000000000000000, 0.5680647467311656929, 0.8229838658936495799 ) ) ;
#12821 = ORIENTED_EDGE ( 'NONE', *, *, #41733, .F. ) ;
#12822 = CARTESIAN_POINT ( 'NONE',  ( 76.48781641346532467, -175.3837268820161057, 2.874563619424060246 ) ) ;
#12823 = EDGE_LOOP ( 'NONE', ( #41728, #1387, #4723, #24322 ) ) ;
#12824 = ADVANCED_FACE ( 'NONE', ( #15160 ), #38016, .T. ) ;
#12825 = CARTESIAN_POINT ( 'NONE',  ( -135.6699833737243353, -193.5000000000000000, 89.56983042009326823 ) ) ;
#12826 = EDGE_CURVE ( 'NONE', #40339, #48757, #14372, .T. ) ;
#12827 = EDGE_CURVE ( 'NONE', #34100, #9007, #7007, .T. ) ;
#12828 = VECTOR ( 'NONE', #13908, 1000.000000000000000 ) ;
#12829 = DIRECTION ( 'NONE',  ( 0.9785564922995032555, 0.000000000000000000, 0.2059786187411021818 ) ) ;
#12830 = VERTEX_POINT ( 'NONE', #3055 ) ;
#12832 = FACE_OUTER_BOUND ( 'NONE', #34144, .T. ) ;
#12831 = CARTESIAN_POINT ( 'NONE',  ( -336.3521761649654422, -123.5000000000000284, 0.000000000000000000 ) ) ;
#12833 = VERTEX_POINT ( 'NONE', #35114 ) ;
#12834 = ADVANCED_FACE ( 'NONE', ( #31171 ), #47221, .T. ) ;
#12835 = ORIENTED_EDGE ( 'NONE', *, *, #964, .F. ) ;
#12836 = CYLINDRICAL_SURFACE ( 'NONE', #37111, 125.0000000000000000 ) ;
#12837 = DIRECTION ( 'NONE',  ( -0.000000000000000000, 0.000000000000000000, -1.000000000000000000 ) ) ;
#12838 = LINE ( 'NONE', #29127, #38941 ) ;
#12839 = LINE ( 'NONE', #36483, #3895 ) ;
#12840 = ORIENTED_EDGE ( 'NONE', *, *, #22405, .F. ) ;
#12841 = AXIS2_PLACEMENT_3D ( 'NONE', #24028, #6968, #43490 ) ;
#12842 = DIRECTION ( 'NONE',  ( -1.000000000000000000, 0.000000000000000000, 0.000000000000000000 ) ) ;
#12843 = APPLICATION_PROTOCOL_DEFINITION ( 'draft international standard', 'automotive_design', 1998, #15947 ) ;
#12844 = DIRECTION ( 'NONE',  ( 1.000000000000000000, 0.000000000000000000, -0.000000000000000000 ) ) ;
#12845 = CARTESIAN_POINT ( 'NONE',  ( -339.1964088526558498, -108.8949048983213004, -57.16590939599337418 ) ) ;
#12846 = CARTESIAN_POINT ( 'NONE',  ( -173.0563034899574859, -189.7472609257535510, -10.27263529369816908 ) ) ;
#12847 = AXIS2_PLACEMENT_3D ( 'NONE', #19287, #42672, #6682 ) ;
#12848 = LINE ( 'NONE', #43870, #24901 ) ;
#12849 = ORIENTED_EDGE ( 'NONE', *, *, #22279, .F. ) ;
#12850 = VERTEX_POINT ( 'NONE', #30143 ) ;
#12851 = CARTESIAN_POINT ( 'NONE',  ( -48.53836737940255119, -175.3837268820161057, -0.9982437317643153563 ) ) ;
#12852 = EDGE_CURVE ( 'NONE', #47304, #23327, #6233, .T. ) ;
#12853 = LINE ( 'NONE', #24957, #27771 ) ;
#12854 = EDGE_CURVE ( 'NONE', #19578, #22206, #40332, .T. ) ;
#12855 = CARTESIAN_POINT ( 'NONE',  ( -114.9600645115007467, -183.6283474603465606, 105.8550183720738147 ) ) ;
#12856 = EDGE_LOOP ( 'NONE', ( #27139, #7475, #25058, #9653 ) ) ;
#12857 = VERTEX_POINT ( 'NONE', #44313 ) ;
#12858 = VECTOR ( 'NONE', #23397, 1000.000000000000000 ) ;
#12859 = ORIENTED_EDGE ( 'NONE', *, *, #39344, .F. ) ;
#12860 = VECTOR ( 'NONE', #18047, 1000.000000000000000 ) ;
#12861 = EDGE_CURVE ( 'NONE', #42654, #47556, #27741, .T. ) ;
#12862 = LINE ( 'NONE', #28882, #41039 ) ;
#12863 = VECTOR ( 'NONE', #36060, 1000.000000000000000 ) ;
#12864 = DIRECTION ( 'NONE',  ( -0.000000000000000000, 1.000000000000000000, -0.000000000000000000 ) ) ;
#12865 = FACE_OUTER_BOUND ( 'NONE', #37225, .T. ) ;
#12866 = DIRECTION ( 'NONE',  ( 0.000000000000000000, -0.000000000000000000, -1.000000000000000000 ) ) ;
#12867 = ORIENTED_EDGE ( 'NONE', *, *, #20608, .T. ) ;
#12868 = DIRECTION ( 'NONE',  ( 0.000000000000000000, 0.8854560256532157947, 0.4647231720437573488 ) ) ;
#12869 = VECTOR ( 'NONE', #48026, 1000.000000000000000 ) ;
#12870 = PLANE ( 'NONE',  #51197 ) ;
#12871 = VERTEX_POINT ( 'NONE', #397 ) ;
#12872 = CARTESIAN_POINT ( 'NONE',  ( -53.47502265695602119, -183.6283474603465606, -124.9001241957025883 ) ) ;
#12873 = ORIENTED_EDGE ( 'NONE', *, *, #19845, .F. ) ;
#12874 = LINE ( 'NONE', #43458, #28368 ) ;
#12875 = ORIENTED_EDGE ( 'NONE', *, *, #33827, .F. ) ;
#12876 = LINE ( 'NONE', #33631, #30960 ) ;
#12877 = VECTOR ( 'NONE', #48616, 1000.000000000000227 ) ;
#12878 = CIRCLE ( 'NONE', #6188, 125.0000000000000000 ) ;
#12879 = DIRECTION ( 'NONE',  ( -0.000000000000000000, 1.000000000000000000, 0.000000000000000000 ) ) ;
#12880 = LINE ( 'NONE', #9214, #36976 ) ;
#12883 = ORIENTED_EDGE ( 'NONE', *, *, #7791, .T. ) ;
#12882 = DIRECTION ( 'NONE',  ( -0.000000000000000000, -1.000000000000000000, 0.000000000000000000 ) ) ;
#12881 = CARTESIAN_POINT ( 'NONE',  ( -75.31296732259116311, -183.6283474603465606, -121.0625654437172614 ) ) ;
#12884 = DIRECTION ( 'NONE',  ( 0.000000000000000000, 0.000000000000000000, 1.000000000000000000 ) ) ;
#12885 = ORIENTED_EDGE ( 'NONE', *, *, #30442, .F. ) ;
#12886 = CARTESIAN_POINT ( 'NONE',  ( 60.00000000000000000, -113.5000000000000000, 60.00000000000000711 ) ) ;
#12887 = DIRECTION ( 'NONE',  ( 0.000000000000000000, 0.000000000000000000, -1.000000000000000000 ) ) ;
#12888 = ORIENTED_EDGE ( 'NONE', *, *, #19651, .T. ) ;
#12889 = ADVANCED_FACE ( 'NONE', ( #143 ), #15421, .T. ) ;
#12890 = ADVANCED_FACE ( 'NONE', ( #27217 ), #28000, .T. ) ;
#12891 = FACE_OUTER_BOUND ( 'NONE', #5557, .T. ) ;
#12893 = DIRECTION ( 'NONE',  ( 0.000000000000000000, 1.000000000000000000, 0.000000000000000000 ) ) ;
#12892 = DIRECTION ( 'NONE',  ( 0.000000000000000000, 0.000000000000000000, 1.000000000000000000 ) ) ;
#12894 = AXIS2_PLACEMENT_3D ( 'NONE', #24521, #36614, #5349 ) ;
#12895 = ORIENTED_EDGE ( 'NONE', *, *, #3409, .T. ) ;
#12896 = CARTESIAN_POINT ( 'NONE',  ( -173.4291566779743050, -189.7472609257535510, 3.534122433558314125 ) ) ;
#12897 = CIRCLE ( 'NONE', #14566, 20.00000000000000000 ) ;
#12898 = DIRECTION ( 'NONE',  ( -0.9473263538541876194, 0.000000000000000000, -0.3202698538628486746 ) ) ;
#12899 = CARTESIAN_POINT ( 'NONE',  ( -47.63353074800702558, -189.7472609257535510, -0.5338233779647817423 ) ) ;
#12900 = VERTEX_POINT ( 'NONE', #47467 ) ;
#12901 = PRESENTATION_STYLE_ASSIGNMENT (( #33133 ) ) ;
#12902 = FACE_OUTER_BOUND ( 'NONE', #17523, .T. ) ;
#12903 = DIRECTION ( 'NONE',  ( 0.000000000000000000, 0.000000000000000000, 1.000000000000000000 ) ) ;
#12904 = FACE_OUTER_BOUND ( 'NONE', #34674, .T. ) ;
#12905 = VERTEX_POINT ( 'NONE', #51425 ) ;
#12906 = DIRECTION ( 'NONE',  ( 0.000000000000000000, 1.000000000000000000, 0.000000000000000000 ) ) ;
#12907 = FACE_OUTER_BOUND ( 'NONE', #42358, .T. ) ;
#12908 = VERTEX_POINT ( 'NONE', #39816 ) ;
#12909 = CARTESIAN_POINT ( 'NONE',  ( -168.8371699641976704, -175.3837268820161057, 33.74820638215506108 ) ) ;
#12910 = DIRECTION ( 'NONE',  ( -0.000000000000000000, 1.000000000000000000, -0.000000000000000000 ) ) ;
#12911 = EDGE_CURVE ( 'NONE', #27896, #39147, #44034, .T. ) ;
#12912 = VECTOR ( 'NONE', #48015, 1000.000000000000000 ) ;
#12913 = CARTESIAN_POINT ( 'NONE',  ( -71.40672220061269115, -175.3837268820161057, -122.8793122007208751 ) ) ;
#12914 = CARTESIAN_POINT ( 'NONE',  ( -339.1964088526558498, -116.7644047441726656, 59.62073260661660612 ) ) ;
#12915 = CARTESIAN_POINT ( 'NONE',  ( -81.70897914701313880, -193.5000000000000000, -120.5021863277716534 ) ) ;
#12916 = AXIS2_PLACEMENT_3D ( 'NONE', #40893, #28799, #8836 ) ;
#12917 = EDGE_CURVE ( 'NONE', #36663, #24196, #36148, .T. ) ;
#12918 = FACE_OUTER_BOUND ( 'NONE', #32187, .T. ) ;
#12919 = FACE_OUTER_BOUND ( 'NONE', #2640, .T. ) ;
#12920 = CARTESIAN_POINT ( 'NONE',  ( -47.50057025920934706, -193.5000000000000000, 0.2059786187411091207 ) ) ;
#12922 = ORIENTED_EDGE ( 'NONE', *, *, #18472, .T. ) ;
#12921 = DIRECTION ( 'NONE',  ( 1.000000000000000000, 0.000000000000000000, 0.000000000000000000 ) ) ;
#12923 = ORIENTED_EDGE ( 'NONE', *, *, #47907, .F. ) ;
#12924 = CARTESIAN_POINT ( 'NONE',  ( -51.89154260666836649, -177.1207230881787780, 124.9534129907280828 ) ) ;
#12925 = DIRECTION ( 'NONE',  ( -0.2920567706369764371, 0.000000000000000000, 0.9564009842765223146 ) ) ;
#12926 = ORIENTED_EDGE ( 'NONE', *, *, #35337, .F. ) ;
#12927 = VERTEX_POINT ( 'NONE', #51946 ) ;
#12928 = VERTEX_POINT ( 'NONE', #12226 ) ;
#12929 = FACE_OUTER_BOUND ( 'NONE', #46649, .T. ) ;
#12930 = DIRECTION ( 'NONE',  ( -0.000000000000000000, 0.000000000000000000, 1.000000000000000000 ) ) ;
#12931 = DIRECTION ( 'NONE',  ( 0.000000000000000000, 0.000000000000000000, -1.000000000000000000 ) ) ;
#12932 = ORIENTED_EDGE ( 'NONE', *, *, #18250, .T. ) ;
#12933 = ORIENTED_EDGE ( 'NONE', *, *, #43822, .F. ) ;
#12934 = EDGE_CURVE ( 'NONE', #28114, #39634, #48524, .T. ) ;
#12935 = FACE_OUTER_BOUND ( 'NONE', #14646, .T. ) ;
#12937 = EDGE_LOOP ( 'NONE', ( #47426, #9261, #24819, #45784 ) ) ;
#12936 = LINE ( 'NONE', #36871, #24120 ) ;
#12938 = DIRECTION ( 'NONE',  ( 0.000000000000000000, 1.000000000000000000, 0.000000000000000000 ) ) ;
#12939 = AXIS2_PLACEMENT_3D ( 'NONE', #36089, #48711, #8237 ) ;
#12940 = ORIENTED_EDGE ( 'NONE', *, *, #23126, .F. ) ;
#12941 = FACE_OUTER_BOUND ( 'NONE', #13745, .T. ) ;
#12942 = ORIENTED_EDGE ( 'NONE', *, *, #47675, .F. ) ;
#12943 = VECTOR ( 'NONE', #19431, 1000.000000000000000 ) ;
#12944 = ADVANCED_FACE ( 'NONE', ( #48248 ), #24075, .T. ) ;
#12945 = DIRECTION ( 'NONE',  ( -1.000000000000000000, 0.000000000000000000, 0.000000000000000000 ) ) ;
#12946 = CARTESIAN_POINT ( 'NONE',  ( -112.1919339979530150, -175.3837268820161057, 107.5438431188761683 ) ) ;
#12947 = CARTESIAN_POINT ( 'NONE',  ( 74.77174840718836890, -193.5000000000000000, 20.83798868929603643 ) ) ;
#12948 = AXIS2_PLACEMENT_3D ( 'NONE', #25089, #25854, #1144 ) ;
#12949 = VERTEX_POINT ( 'NONE', #35626 ) ;
#12950 = ADVANCED_FACE ( 'NONE', ( #40091 ), #7776, .F. ) ;
#12951 = ORIENTED_EDGE ( 'NONE', *, *, #43319, .T. ) ;
#12952 = LINE ( 'NONE', #28976, #39905 ) ;
#12953 = LINE ( 'NONE', #25068, #28359 ) ;
#12954 = ORIENTED_EDGE ( 'NONE', *, *, #19492, .T. ) ;
#12955 = CARTESIAN_POINT ( 'NONE',  ( -48.47912675150885065, -175.3837268820161057, 6.938893903907228378E-15 ) ) ;
#12956 = DIRECTION ( 'NONE',  ( -0.000000000000000000, 1.000000000000000000, -0.000000000000000000 ) ) ;
#12957 = VERTEX_POINT ( 'NONE', #27489 ) ;
#12958 = DIRECTION ( 'NONE',  ( -0.000000000000000000, 1.000000000000000000, -0.000000000000000000 ) ) ;
#12959 = CIRCLE ( 'NONE', #42338, 4.999999999999997335 ) ;
#12960 = CARTESIAN_POINT ( 'NONE',  ( -336.3521761649654422, -135.0638248728647852, 57.91551518289418254 ) ) ;
#12961 = PRODUCT ( 'Eccentric Cam Locking Shaft', 'Eccentric Cam Locking Shaft', '', ( #1275 ) ) ;
#12962 = VERTEX_POINT ( 'NONE', #31427 ) ;
#12963 = LINE ( 'NONE', #16684, #24034 ) ;
#12964 = VERTEX_POINT ( 'NONE', #11446 ) ;
#12965 = CARTESIAN_POINT ( 'NONE',  ( -339.1964088526558498, -182.0095552316576573, -7.608018572112655420 ) ) ;
#12966 = DIRECTION ( 'NONE',  ( 0.6528221181905227155, 0.000000000000000000, -0.7575112421616191360 ) ) ;
#12967 = EDGE_CURVE ( 'NONE', #12202, #41381, #3839, .T. ) ;
#12968 = ORIENTED_EDGE ( 'NONE', *, *, #29528, .T. ) ;
#12969 = ADVANCED_BREP_SHAPE_REPRESENTATION ( '', ( #36582, #31742 ), #8256 ) ;
#12970 = DIRECTION ( 'NONE',  ( -0.7575112421616191360, 0.000000000000000000, -0.6528221181905227155 ) ) ;
#12971 = CARTESIAN_POINT ( 'NONE',  ( -305.0000000000000568, -113.6616659693417546, 59.18789727217205154 ) ) ;
#12972 = PLANE ( 'NONE',  #5619 ) ;
#12973 = CARTESIAN_POINT ( 'NONE',  ( -11.17913199888832843, -189.7472609257535510, 119.3051146910914326 ) ) ;
#12974 = ORIENTED_EDGE ( 'NONE', *, *, #18207, .F. ) ;
#12975 = PLANE ( 'NONE',  #27836 ) ;
#12976 = ORIENTED_EDGE ( 'NONE', *, *, #20373, .T. ) ;
#12977 = ORIENTED_EDGE ( 'NONE', *, *, #47534, .T. ) ;
#12978 = CARTESIAN_POINT ( 'NONE',  ( 11.52087324849114580, -173.5000000000000284, -60.00000000000002842 ) ) ;
#12980 = VERTEX_POINT ( 'NONE', #8302 ) ;
#12979 = CARTESIAN_POINT ( 'NONE',  ( -8.721998590732187751, -177.1207230881787780, -118.5089480183145270 ) ) ;
#12981 = AXIS2_PLACEMENT_3D ( 'NONE', #42290, #2372, #18402 ) ;
#12982 = CIRCLE ( 'NONE', #2903, 125.0000000000000000 ) ;
#12983 = VERTEX_POINT ( 'NONE', #20376 ) ;
#12984 = DIRECTION ( 'NONE',  ( 1.000000000000000000, 0.000000000000000000, 0.000000000000000000 ) ) ;
#12985 = CIRCLE ( 'NONE', #49965, 125.0000000000000000 ) ;
#12986 = DIRECTION ( 'NONE',  ( 0.000000000000000000, 0.9927088740980539727, -0.1205366802553233252 ) ) ;
#12987 = CARTESIAN_POINT ( 'NONE',  ( -173.4460699164830260, -175.3837268820161057, -2.874563619423202265 ) ) ;
#12988 = ORIENTED_EDGE ( 'NONE', *, *, #50875, .T. ) ;
#12989 = DIRECTION ( 'NONE',  ( -0.000000000000000000, 0.8229838658936634577, 0.5680647467311457088 ) ) ;
#12990 = CIRCLE ( 'NONE', #44896, 60.00000000000000000 ) ;
#12991 = ORIENTED_EDGE ( 'NONE', *, *, #36154, .F. ) ;
#12992 = CARTESIAN_POINT ( 'NONE',  ( -330.4913330509368166, -182.1300919119128423, 6.615309698015510165 ) ) ;
#12993 = CARTESIAN_POINT ( 'NONE',  ( -339.1964088526558498, -78.25935320507889514, 39.41172259083828777 ) ) ;
#12994 = AXIS2_PLACEMENT_3D ( 'NONE', #28755, #48508, #41120 ) ;
#12995 = ADVANCED_FACE ( 'NONE', ( #32469, #43252 ), #23307, .F. ) ;
#12997 = AXIS2_PLACEMENT_3D ( 'NONE', #11389, #7474, #47926 ) ;
#12996 = LINE ( 'NONE', #16716, #29445 ) ;
#12998 = CARTESIAN_POINT ( 'NONE',  ( -47.57632892154310866, -183.6283474603465606, -0.4300652022765113491 ) ) ;
#12999 = ORIENTED_EDGE ( 'NONE', *, *, #896, .F. ) ;
#13000 = ORIENTED_EDGE ( 'NONE', *, *, #5805, .T. ) ;
#13001 = ORIENTED_EDGE ( 'NONE', *, *, #34535, .T. ) ;
#13002 = EDGE_CURVE ( 'NONE', #16187, #25920, #35366, .T. ) ;
#13003 = CARTESIAN_POINT ( 'NONE',  ( -48.47912675150885065, -183.6283474603465606, 6.938893903907228378E-15 ) ) ;
#13004 = DIRECTION ( 'NONE',  ( 0.000000000000000000, 1.000000000000000000, -0.000000000000000000 ) ) ;
#13005 = FACE_OUTER_BOUND ( 'NONE', #8430, .T. ) ;
#13006 = DIRECTION ( 'NONE',  ( -0.000000000000000000, -1.000000000000000000, -0.000000000000000000 ) ) ;
#13007 = FACE_OUTER_BOUND ( 'NONE', #32466, .T. ) ;
#13008 = VERTEX_POINT ( 'NONE', #39561 ) ;
#13009 = ADVANCED_FACE ( 'NONE', ( #19606 ), #51678, .T. ) ;
#13010 = EDGE_CURVE ( 'NONE', #24862, #10381, #37712, .T. ) ;
#13011 = EDGE_CURVE ( 'NONE', #12713, #24991, #4200, .T. ) ;
#13012 = ORIENTED_EDGE ( 'NONE', *, *, #3112, .T. ) ;
#13014 = ORIENTED_EDGE ( 'NONE', *, *, #10991, .F. ) ;
#13013 = DIRECTION ( 'NONE',  ( -8.718379230999708359E-17, -0.2393156642875652051, -0.9709418174260502354 ) ) ;
#13015 = VERTEX_POINT ( 'NONE', #4611 ) ;
#13016 = EDGE_CURVE ( 'NONE', #36281, #31485, #12740, .T. ) ;
#13017 = VECTOR ( 'NONE', #21852, 1000.000000000000114 ) ;
#13018 = FACE_OUTER_BOUND ( 'NONE', #6214, .T. ) ;
#13019 = EDGE_CURVE ( 'NONE', #48355, #6199, #44558, .T. ) ;
#13020 = DIRECTION ( 'NONE',  ( 0.000000000000000000, 1.000000000000000000, -0.000000000000000000 ) ) ;
#13021 = CIRCLE ( 'NONE', #51634, 125.0000000000000000 ) ;
#13022 = VECTOR ( 'NONE', #36703, 999.9999999999998863 ) ;
#13023 = PLANE ( 'NONE',  #17866 ) ;
#13024 = DIRECTION ( 'NONE',  ( -1.000000000000000000, -0.000000000000000000, 0.000000000000000000 ) ) ;
#13025 = CARTESIAN_POINT ( 'NONE',  ( -330.4913330509368166, -143.9541802141672235, -55.34326076196065003 ) ) ;
#13026 = EDGE_LOOP ( 'NONE', ( #31259, #28413, #34326, #49616 ) ) ;
#13027 = CARTESIAN_POINT ( 'NONE',  ( -48.47912675150885065, -175.3837268820161057, 125.0000000000000000 ) ) ;
#13028 = ORIENTED_EDGE ( 'NONE', *, *, #50354, .F. ) ;
#13029 = AXIS2_PLACEMENT_3D ( 'NONE', #9902, #37744, #13046 ) ;
#13030 = ORIENTED_EDGE ( 'NONE', *, *, #971, .F. ) ;
#13031 = CARTESIAN_POINT ( 'NONE',  ( -336.3521761649654422, -65.58448481710581746, 11.56382487286456140 ) ) ;
#13032 = VECTOR ( 'NONE', #44043, 1000.000000000000000 ) ;
#13033 = PLANE ( 'NONE',  #39580 ) ;
#13034 = AXIS2_PLACEMENT_3D ( 'NONE', #28502, #5132, #27987 ) ;
#13035 = PLANE ( 'NONE',  #45800 ) ;
#13036 = CARTESIAN_POINT ( 'NONE',  ( -330.4913330509368166, -116.8846903019851311, -58.63009191191288494 ) ) ;
#13037 = DIRECTION ( 'NONE',  ( -1.000000000000000000, 0.000000000000000000, 0.000000000000000000 ) ) ;
#13038 = ORIENTED_EDGE ( 'NONE', *, *, #17516, .F. ) ;
#13039 = AXIS2_PLACEMENT_3D ( 'NONE', #29430, #22325, #45483 ) ;
#13040 = CARTESIAN_POINT ( 'NONE',  ( -117.0614752283615019, -193.5000000000000000, 103.3076327631967928 ) ) ;
#13041 = CARTESIAN_POINT ( 'NONE',  ( -129.4514457347087273, -193.5000000000000000, 95.22858582633115532 ) ) ;
#13043 = AXIS2_PLACEMENT_3D ( 'NONE', #17809, #22981, #21236 ) ;
#13042 = DIRECTION ( 'NONE',  ( 0.000000000000000000, 0.000000000000000000, 1.000000000000000000 ) ) ;
#13044 = FACE_BOUND ( 'NONE', #46602, .T. ) ;
#13045 = ORIENTED_EDGE ( 'NONE', *, *, #11224, .T. ) ;
#13046 = DIRECTION ( 'NONE',  ( 0.000000000000000000, -2.567390744445674500E-14, 1.000000000000000000 ) ) ;
#13047 = ORIENTED_EDGE ( 'NONE', *, *, #7681, .T. ) ;
#13048 = CARTESIAN_POINT ( 'NONE',  ( -130.2106798473772642, -175.3837268820161057, 94.57776286494217288 ) ) ;
#13049 = ORIENTED_EDGE ( 'NONE', *, *, #22700, .T. ) ;
#13050 = CARTESIAN_POINT ( 'NONE',  ( -305.0000000000000568, -67.57827586672165410, -21.74306257088711547 ) ) ;
#13051 = ORIENTED_EDGE ( 'NONE', *, *, #33725, .F. ) ;
#13052 = CARTESIAN_POINT ( 'NONE',  ( 55.92943606843918047, -189.7472609257535510, -66.89437584437831674 ) ) ;
#13053 = AXIS2_PLACEMENT_3D ( 'NONE', #39217, #30817, #14280 ) ;
#13054 = CARTESIAN_POINT ( 'NONE',  ( 46.00000000000000711, -57.64213562373095101, -51.00000000000000000 ) ) ;
#13056 = ORIENTED_EDGE ( 'NONE', *, *, #18533, .F. ) ;
#13055 = DIRECTION ( 'NONE',  ( -0.9473263538541876194, 0.000000000000000000, -0.3202698538628486746 ) ) ;
#13057 = AXIS2_PLACEMENT_3D ( 'NONE', #26082, #21643, #37663 ) ;
#13058 = AXIS2_PLACEMENT_3D ( 'NONE', #50547, #27123, #47118 ) ;
#13059 = ADVANCED_FACE ( 'NONE', ( #37187 ), #9342, .F. ) ;
#13060 = ADVANCED_FACE ( 'NONE', ( #49558 ), #925, .T. ) ;
#13061 = EDGE_CURVE ( 'NONE', #3589, #44850, #20638, .T. ) ;
#13062 = LINE ( 'NONE', #41177, #862 ) ;
#13063 = VERTEX_POINT ( 'NONE', #676 ) ;
#13064 = VERTEX_POINT ( 'NONE', #32728 ) ;
#13065 = EDGE_CURVE ( 'NONE', #46710, #36128, #45612, .T. ) ;
#13066 = ORIENTED_EDGE ( 'NONE', *, *, #49350, .F. ) ;
#13067 = DIRECTION ( 'NONE',  ( 0.000000000000000000, -1.000000000000000000, 0.000000000000000000 ) ) ;
#13068 = DIRECTION ( 'NONE',  ( 0.7175072570443249420, 0.000000000000000000, 0.6965510290630033685 ) ) ;
#13069 = ORIENTED_EDGE ( 'NONE', *, *, #5103, .F. ) ;
#13070 = VECTOR ( 'NONE', #7908, 1000.000000000000000 ) ;
#13071 = FACE_OUTER_BOUND ( 'NONE', #43452, .T. ) ;
#13072 = ADVANCED_FACE ( 'NONE', ( #16724 ), #29029, .F. ) ;
#13073 = AXIS2_PLACEMENT_3D ( 'NONE', #18506, #19023, #47139 ) ;
#13074 = CARTESIAN_POINT ( 'NONE',  ( -339.1964088526558498, -123.5000000000000284, 0.000000000000000000 ) ) ;
#13075 = CARTESIAN_POINT ( 'NONE',  ( -330.4913330509368166, -68.15673923803900891, 20.45418021416622878 ) ) ;
#13076 = ORIENTED_EDGE ( 'NONE', *, *, #38803, .T. ) ;
#13077 = EDGE_CURVE ( 'NONE', #8870, #22194, #12495, .T. ) ;
#13078 = VECTOR ( 'NONE', #29112, 1000.000000000000227 ) ;
#13079 = ADVANCED_FACE ( 'NONE', ( #29556 ), #8543, .F. ) ;
#13080 = CIRCLE ( 'NONE', #32391, 125.0000000000000000 ) ;
#13081 = DIRECTION ( 'NONE',  ( -0.000000000000000000, 1.000000000000000000, -0.000000000000000000 ) ) ;
#13082 = CARTESIAN_POINT ( 'NONE',  ( 32.34187644556188701, -189.7472609257535510, 94.04236105995856576 ) ) ;
#13083 = EDGE_LOOP ( 'NONE', ( #23623, #16842, #3079, #48576 ) ) ;
#13086 = ORIENTED_EDGE ( 'NONE', *, *, #37473, .F. ) ;
#13085 = DIRECTION ( 'NONE',  ( -0.000000000000000000, -0.9709418174260511236, 0.2393156642875615969 ) ) ;
#13084 = CARTESIAN_POINT ( 'NONE',  ( -336.3521761649654422, -127.9985676343858501, 58.88711093124869222 ) ) ;
#13087 = ORIENTED_EDGE ( 'NONE', *, *, #22931, .T. ) ;
#13088 = ADVANCED_FACE ( 'NONE', ( #5405 ), #24578, .F. ) ;
#13089 = CARTESIAN_POINT ( 'NONE',  ( -116.2964108826154330, -183.6283474603465606, -105.0038855142073260 ) ) ;
#13090 = ORIENTED_EDGE ( 'NONE', *, *, #46564, .F. ) ;
#13091 = CARTESIAN_POINT ( 'NONE',  ( 8.294189685504184339, -189.7472609257535510, -110.2396968984190977 ) ) ;
#13092 = VERTEX_POINT ( 'NONE', #16971 ) ;
#13093 = EDGE_CURVE ( 'NONE', #48020, #51413, #4889, .T. ) ;
#13094 = DIRECTION ( 'NONE',  ( -0.000000000000000000, 1.000000000000000000, -0.000000000000000000 ) ) ;
#13095 = PLANE ( 'NONE',  #25879 ) ;
#13096 = ORIENTED_EDGE ( 'NONE', *, *, #22634, .T. ) ;
#13097 = FACE_OUTER_BOUND ( 'NONE', #26136, .T. ) ;
#13098 = ORIENTED_EDGE ( 'NONE', *, *, #788, .F. ) ;
#13099 = ORIENTED_EDGE ( 'NONE', *, *, #49093, .F. ) ;
#13100 = LINE ( 'NONE', #45187, #27871 ) ;
#13101 = AXIS2_PLACEMENT_3D ( 'NONE', #6332, #2638, #34692 ) ;
#13102 = FACE_OUTER_BOUND ( 'NONE', #25452, .T. ) ;
#13103 = AXIS2_PLACEMENT_3D ( 'NONE', #9432, #25972, #25457 ) ;
#13104 = CARTESIAN_POINT ( 'NONE',  ( 39.18328161278951427, -189.7472609257535510, 89.10837311819236106 ) ) ;
#13105 = ORIENTED_EDGE ( 'NONE', *, *, #33964, .F. ) ;
#13106 = CIRCLE ( 'NONE', #485, 125.0000000000000000 ) ;
#13107 = PLANE ( 'NONE',  #43184 ) ;
#13108 = VECTOR ( 'NONE', #38685, 1000.000000000000000 ) ;
#13109 = APPLICATION_PROTOCOL_DEFINITION ( 'draft international standard', 'automotive_design', 1998, #12554 ) ;
#13110 = CARTESIAN_POINT ( 'NONE',  ( -330.4913330509368166, -83.33976666098958219, 44.57752413667940772 ) ) ;
#13111 = CARTESIAN_POINT ( 'NONE',  ( 0.000000000000000000, -68.33404168156025094, 20.92168833550889673 ) ) ;
#13112 = FACE_OUTER_BOUND ( 'NONE', #16011, .T. ) ;
#13113 = ADVANCED_FACE ( 'NONE', ( #33243 ), #36936, .F. ) ;
#13114 = CARTESIAN_POINT ( 'NONE',  ( 75.95066919219054569, -175.3837268820161057, -11.92584929509535385 ) ) ;
#13115 = DIRECTION ( 'NONE',  ( 0.000000000000000000, 0.2393156642875482742, -0.9709418174260544543 ) ) ;
#13116 = ORIENTED_EDGE ( 'NONE', *, *, #37869, .T. ) ;
#13117 = ORIENTED_EDGE ( 'NONE', *, *, #48386, .T. ) ;
#13118 = VECTOR ( 'NONE', #39704, 1000.000000000000000 ) ;
#13119 = VECTOR ( 'NONE', #51146, 1000.000000000000000 ) ;
#13120 = AXIS2_PLACEMENT_3D ( 'NONE', #47309, #43359, #11023 ) ;
#13121 = CARTESIAN_POINT ( 'NONE',  ( 60.02977459919872416, -193.5000000000000000, 60.01515274641010222 ) ) ;
#13122 = CARTESIAN_POINT ( 'NONE',  ( -336.3521761649653854, -183.4777928329299357, 1.632288850093980725 ) ) ;
#13123 = ORIENTED_EDGE ( 'NONE', *, *, #7918, .T. ) ;
#13124 = DIRECTION ( 'NONE',  ( -0.000000000000000000, 0.1205366802553303196, 0.9927088740980530845 ) ) ;
#13125 = VECTOR ( 'NONE', #13946, 1000.000000000000000 ) ;
#13126 = VERTEX_POINT ( 'NONE', #17503 ) ;
#13127 = AXIS2_PLACEMENT_3D ( 'NONE', #12372, #43662, #16321 ) ;
#13128 = ADVANCED_FACE ( 'NONE', ( #33517 ), #41638, .T. ) ;
#13129 = DIRECTION ( 'NONE',  ( 0.000000000000000000, 1.000000000000000000, 0.000000000000000000 ) ) ;
#13130 = CARTESIAN_POINT ( 'NONE',  ( 2.449293598294706513E-15, -53.50000000000000000, 20.00000000000000000 ) ) ;
#13131 = DIRECTION ( 'NONE',  ( 1.000000000000000000, -0.000000000000000000, -0.000000000000000000 ) ) ;
#13132 = CARTESIAN_POINT ( 'NONE',  ( -48.47912675150885065, -183.6283474603465606, 6.938893903907228378E-15 ) ) ;
#13133 = VERTEX_POINT ( 'NONE', #49810 ) ;
#13134 = EDGE_CURVE ( 'NONE', #11371, #10636, #36107, .T. ) ;
#13135 = EDGE_CURVE ( 'NONE', #49319, #16002, #23512, .T. ) ;
#13136 = EDGE_CURVE ( 'NONE', #38627, #28107, #6698, .T. ) ;
#13137 = ADVANCED_FACE ( 'NONE', ( #34023 ), #50069, .F. ) ;
#13138 = DIRECTION ( 'NONE',  ( 0.6528221181905119463, 0.000000000000000000, 0.7575112421616284619 ) ) ;
#13139 = EDGE_CURVE ( 'NONE', #37982, #2579, #14846, .T. ) ;
#13140 = DIRECTION ( 'NONE',  ( -1.000000000000000000, 0.000000000000000000, 0.000000000000000000 ) ) ;
#13141 = ORIENTED_EDGE ( 'NONE', *, *, #7360, .F. ) ;
#13142 = CYLINDRICAL_SURFACE ( 'NONE', #43503, 125.0000000000000000 ) ;
#13143 = VECTOR ( 'NONE', #16483, 1000.000000000000000 ) ;
#13144 = AXIS2_PLACEMENT_3D ( 'NONE', #45066, #112, #20342 ) ;
#13145 = VERTEX_POINT ( 'NONE', #5926 ) ;
#13146 = EDGE_CURVE ( 'NONE', #45652, #38573, #9857, .T. ) ;
#13147 = EDGE_CURVE ( 'NONE', #3885, #21496, #42157, .T. ) ;
#13148 = DIRECTION ( 'NONE',  ( 0.000000000000000000, 0.000000000000000000, -1.000000000000000000 ) ) ;
#13149 = EDGE_CURVE ( 'NONE', #33039, #49664, #1967, .T. ) ;
#13150 = EDGE_CURVE ( 'NONE', #46777, #17068, #33606, .T. ) ;
#13151 = DIRECTION ( 'NONE',  ( 0.000000000000000000, 6.476300976980080240E-14, -1.000000000000000000 ) ) ;
#13152 = DIRECTION ( 'NONE',  ( 1.000000000000000000, -0.000000000000000000, 0.000000000000000000 ) ) ;
#13155 = ORIENTED_EDGE ( 'NONE', *, *, #6398, .T. ) ;
#13154 = FACE_OUTER_BOUND ( 'NONE', #51109, .T. ) ;
#13153 = CARTESIAN_POINT ( 'NONE',  ( 43.33156026654913262, 30.00000000000000355, -51.04247435516399634 ) ) ;
#13156 = AXIS2_PLACEMENT_3D ( 'NONE', #51677, #15676, #4610 ) ;
#13157 = ADVANCED_FACE ( 'NONE', ( #34530 ), #38488, .F. ) ;
#13158 = VECTOR ( 'NONE', #26281, 1000.000000000000000 ) ;
#13159 = VECTOR ( 'NONE', #25981, 999.9999999999998863 ) ;
#13160 = CARTESIAN_POINT ( 'NONE',  ( -47.82630463331833681, -183.6283474603465606, 0.7575112421616305713 ) ) ;
#13162 = ORIENTED_EDGE ( 'NONE', *, *, #40725, .T. ) ;
#13161 = AXIS2_PLACEMENT_3D ( 'NONE', #48482, #24540, #36634 ) ;
#13163 = LINE ( 'NONE', #9478, #24738 ) ;
#13164 = DIRECTION ( 'NONE',  ( 0.000000000000000000, -0.9709418174260492362, 0.2393156642875685636 ) ) ;
#13165 = ORIENTED_EDGE ( 'NONE', *, *, #29852, .T. ) ;
#13166 = EDGE_CURVE ( 'NONE', #3937, #40253, #14580, .T. ) ;
#13167 = AXIS2_PLACEMENT_3D ( 'NONE', #137, #3316, #36141 ) ;
#13168 = DIRECTION ( 'NONE',  ( 0.000000000000000000, 0.3546048870425363986, 0.9350162426854146114 ) ) ;
#13170 = DIRECTION ( 'NONE',  ( 1.000000000000000000, -0.000000000000000000, -0.000000000000000000 ) ) ;
#13169 = DIRECTION ( 'NONE',  ( -0.2920567706369833760, 0.000000000000000000, 0.9564009842765202052 ) ) ;
#13171 = VERTEX_POINT ( 'NONE', #26658 ) ;
#13172 = EDGE_CURVE ( 'NONE', #32165, #26290, #2227, .T. ) ;
#13173 = AXIS2_PLACEMENT_3D ( 'NONE', #10065, #50277, #1662 ) ;
#13174 = DIRECTION ( 'NONE',  ( -0.000000000000000000, -0.9350162426854169428, -0.3546048870425300148 ) ) ;
#13175 = FACE_BOUND ( 'NONE', #10071, .T. ) ;
#13176 = LINE ( 'NONE', #29444, #47515 ) ;
#13177 = EDGE_LOOP ( 'NONE', ( #20687, #42146, #9291, #23836 ) ) ;
#13178 = CARTESIAN_POINT ( 'NONE',  ( -339.1964088526558498, -182.5000000000000568, 0.5000000000000457412 ) ) ;
#13179 = CYLINDRICAL_SURFACE ( 'NONE', #50948, 125.0000000000000000 ) ;
#13180 = LINE ( 'NONE', #13433, #7501 ) ;
#13181 = CARTESIAN_POINT ( 'NONE',  ( -365.0000000000001137, -168.5000000000000284, 10.00000000000000711 ) ) ;
#13182 = ORIENTED_EDGE ( 'NONE', *, *, #8681, .T. ) ;
#13183 = DIRECTION ( 'NONE',  ( -1.000000000000000000, 0.000000000000000000, -0.000000000000000000 ) ) ;
#13184 = CARTESIAN_POINT ( 'NONE',  ( -19.28375372365792728, -175.3837268820161057, 121.5427093402341541 ) ) ;
#13185 = EDGE_CURVE ( 'NONE', #21275, #44850, #16817, .T. ) ;
#13186 = CARTESIAN_POINT ( 'NONE',  ( 50.70030191143631271, -177.1207230881787780, -76.08180419845318454 ) ) ;
#13187 = ORIENTED_EDGE ( 'NONE', *, *, #612, .F. ) ;
#13188 = AXIS2_PLACEMENT_3D ( 'NONE', #51642, #8004, #31662 ) ;
#13189 = CARTESIAN_POINT ( 'NONE',  ( 25.43954814678888710, -183.6283474603465606, 100.8019320314832754 ) ) ;
#13190 = PLANE ( 'NONE',  #37868 ) ;
#13191 = AXIS2_PLACEMENT_3D ( 'NONE', #51863, #31343, #40254 ) ;
#13192 = LINE ( 'NONE', #306, #10942 ) ;
#13193 = CARTESIAN_POINT ( 'NONE',  ( 60.00000000000001421, 20.00000000000000000, -60.00000000000000711 ) ) ;
#13194 = LINE ( 'NONE', #40769, #46450 ) ;
#13195 = AXIS2_PLACEMENT_3D ( 'NONE', #51359, #19300, #28187 ) ;
#13196 = CIRCLE ( 'NONE', #14069, 125.0000000000000000 ) ;
#13197 = LINE ( 'NONE', #29219, #36208 ) ;
#13198 = LINE ( 'NONE', #24757, #2718 ) ;
#13200 = ORIENTED_EDGE ( 'NONE', *, *, #7952, .T. ) ;
#13199 = DIRECTION ( 'NONE',  ( -1.000000000000000000, 0.000000000000000000, 0.000000000000000000 ) ) ;
#13201 = CIRCLE ( 'NONE', #9000, 125.0000000000000000 ) ;
#13202 = EDGE_LOOP ( 'NONE', ( #33084, #30088, #23181, #18275 ) ) ;
#13203 = EDGE_CURVE ( 'NONE', #12033, #41128, #39434, .T. ) ;
#13204 = EDGE_CURVE ( 'NONE', #31327, #3759, #38216, .T. ) ;
#13205 = FACE_OUTER_BOUND ( 'NONE', #6293, .T. ) ;
#13206 = VECTOR ( 'NONE', #19787, 1000.000000000000000 ) ;
#13207 = CARTESIAN_POINT ( 'NONE',  ( -48.47912675150885065, -189.7472609257535510, 6.938893903907228378E-15 ) ) ;
#13209 = ORIENTED_EDGE ( 'NONE', *, *, #19202, .T. ) ;
#13208 = CARTESIAN_POINT ( 'NONE',  ( -15.81236726369125023, -193.5000000000000000, -120.6560517527615417 ) ) ;
#13210 = ORIENTED_EDGE ( 'NONE', *, *, #26302, .F. ) ;
#13211 = VERTEX_POINT ( 'NONE', #6943 ) ;
#13212 = CARTESIAN_POINT ( 'NONE',  ( 64.44365795514079309, -175.3837268820161057, -53.60452120946195009 ) ) ;
#13213 = DIRECTION ( 'NONE',  ( -0.3482016354343866471, 0.000000000000000000, -0.9374196611341253371 ) ) ;
#13214 = DIRECTION ( 'NONE',  ( -0.000000000000000000, 1.000000000000000000, 0.000000000000000000 ) ) ;
#13215 = VERTEX_POINT ( 'NONE', #18268 ) ;
#13216 = LINE ( 'NONE', #4547, #1714 ) ;
#13217 = VECTOR ( 'NONE', #7283, 1000.000000000000000 ) ;
#13219 = ORIENTED_EDGE ( 'NONE', *, *, #19208, .T. ) ;
#13218 = DIRECTION ( 'NONE',  ( 0.000000000000000000, 0.000000000000000000, -1.000000000000000000 ) ) ;
#13220 = CIRCLE ( 'NONE', #21630, 20.00000000000000000 ) ;
#13221 = EDGE_CURVE ( 'NONE', #49515, #17649, #34288, .T. ) ;
#13222 = DIRECTION ( 'NONE',  ( -0.000000000000000000, 1.000000000000000000, -0.000000000000000000 ) ) ;
#13223 = EDGE_LOOP ( 'NONE', ( #39125, #24687, #20891, #24250 ) ) ;
#13224 = DIRECTION ( 'NONE',  ( -1.000000000000000000, 0.000000000000000000, 0.000000000000000000 ) ) ;
#13225 = AXIS2_PLACEMENT_3D ( 'NONE', #21549, #45462, #1572 ) ;
#13226 = ORIENTED_EDGE ( 'NONE', *, *, #19984, .F. ) ;
#13227 = PLANE ( 'NONE',  #17380 ) ;
#13228 = CARTESIAN_POINT ( 'NONE',  ( -339.1964088526558498, -75.22798428563991990, -33.92731199008514409 ) ) ;
#13229 = PLANE ( 'NONE',  #16509 ) ;
#13230 = ADVANCED_FACE ( 'NONE', ( #38984 ), #18771, .T. ) ;
#13231 = EDGE_LOOP ( 'NONE', ( #18728, #30871, #36443, #30692 ) ) ;
#13232 = VECTOR ( 'NONE', #8794, 1000.000000000000000 ) ;
#13233 = ORIENTED_EDGE ( 'NONE', *, *, #40053, .F. ) ;
#13234 = DIRECTION ( 'NONE',  ( -0.000000000000000000, 1.000000000000000000, -0.000000000000000000 ) ) ;
#13235 = DIRECTION ( 'NONE',  ( 0.000000000000000000, -0.7485107481710999711, 0.6631226582407964143 ) ) ;
#13236 = AXIS2_PLACEMENT_3D ( 'NONE', #44693, #36274, #275 ) ;
#13237 = VERTEX_POINT ( 'NONE', #44236 ) ;
#13238 = FACE_OUTER_BOUND ( 'NONE', #33496, .T. ) ;
#13239 = VECTOR ( 'NONE', #41923, 1000.000000000000000 ) ;
#13240 = PLANE ( 'NONE',  #204 ) ;
#13241 = ORIENTED_EDGE ( 'NONE', *, *, #1457, .T. ) ;
#13242 = FACE_BOUND ( 'NONE', #47033, .T. ) ;
#13243 = CIRCLE ( 'NONE', #24859, 125.0000000000000000 ) ;
#13244 = LINE ( 'NONE', #12960, #6358 ) ;
#13245 = AXIS2_PLACEMENT_3D ( 'NONE', #13153, #37839, #49436 ) ;
#13246 = ORIENTED_EDGE ( 'NONE', *, *, #14564, .F. ) ;
#13247 = DIRECTION ( 'NONE',  ( -0.000000000000000000, -1.000000000000000000, 0.000000000000000000 ) ) ;
#13248 = ORIENTED_EDGE ( 'NONE', *, *, #24720, .F. ) ;
#13249 = CARTESIAN_POINT ( 'NONE',  ( 63.31225588004632243, -177.1207230881787780, 55.92572546981597981 ) ) ;
#13250 = VERTEX_POINT ( 'NONE', #11386 ) ;
#13251 = CARTESIAN_POINT ( 'NONE',  ( 0.000000000000000000, -137.6196241929653752, 57.28556722813723212 ) ) ;
#13252 = LINE ( 'NONE', #12971, #10442 ) ;
#13253 = LINE ( 'NONE', #34255, #34963 ) ;
#13254 = CARTESIAN_POINT ( 'NONE',  ( -336.3521761649654422, -113.7752393642576720, 58.25253621232167944 ) ) ;
#13255 = ORIENTED_EDGE ( 'NONE', *, *, #24896, .T. ) ;
#13256 = DIRECTION ( 'NONE',  ( -0.000000000000000000, -1.000000000000000000, 0.000000000000000000 ) ) ;
#13257 = EDGE_LOOP ( 'NONE', ( #25420, #15587, #2524, #6863 ) ) ;
#13258 = ORIENTED_EDGE ( 'NONE', *, *, #33779, .T. ) ;
#13259 = AXIS2_PLACEMENT_3D ( 'NONE', #7983, #48719, #20324 ) ;
#13260 = VECTOR ( 'NONE', #4371, 1000.000000000000000 ) ;
#13261 = CARTESIAN_POINT ( 'NONE',  ( -305.0000000000000568, -182.3303666475049170, -11.78931550685388707 ) ) ;
#13263 = VERTEX_POINT ( 'NONE', #47677 ) ;
#13262 = CARTESIAN_POINT ( 'NONE',  ( -48.47912675150885065, -175.3837268820161057, 124.0000000000000142 ) ) ;
#13264 = AXIS2_PLACEMENT_3D ( 'NONE', #5336, #28952, #41844 ) ;
#13265 = ORIENTED_EDGE ( 'NONE', *, *, #52011, .F. ) ;
#13266 = DIRECTION ( 'NONE',  ( 1.000000000000000000, 0.000000000000000000, -0.000000000000000000 ) ) ;
#13267 = EDGE_CURVE ( 'NONE', #9868, #7246, #8232, .T. ) ;
#13268 = PLANE ( 'NONE',  #33817 ) ;
#13269 = DIRECTION ( 'NONE',  ( -0.000000000000000000, 1.000000000000000000, -0.000000000000000000 ) ) ;
#13270 = AXIS2_PLACEMENT_3D ( 'NONE', #38600, #2604, #14694 ) ;
#13271 = VERTEX_POINT ( 'NONE', #27683 ) ;
#13272 = LINE ( 'NONE', #29799, #34009 ) ;
#13273 = VERTEX_POINT ( 'NONE', #32140 ) ;
#13274 = CARTESIAN_POINT ( 'NONE',  ( 50.27798938500057346, -183.6283474603465606, 74.98773087994527486 ) ) ;
#13275 = CARTESIAN_POINT ( 'NONE',  ( -305.0000000000000568, -144.3080463282022663, -56.27632902032068785 ) ) ;
#13276 = CARTESIAN_POINT ( 'NONE',  ( -332.3517673607765914, -65.58448481710581746, 11.56382487286456140 ) ) ;
#13277 = DIRECTION ( 'NONE',  ( 0.000000000000000000, 1.000000000000000000, 0.000000000000000000 ) ) ;
#13278 = EDGE_LOOP ( 'NONE', ( #26018, #18347, #11986, #14401 ) ) ;
#13279 = ORIENTED_EDGE ( 'NONE', *, *, #14110, .T. ) ;
#13280 = ORIENTED_EDGE ( 'NONE', *, *, #50656, .T. ) ;
#13281 = VECTOR ( 'NONE', #34913, 1000.000000000000000 ) ;
#13282 = FACE_OUTER_BOUND ( 'NONE', #38421, .T. ) ;
#13283 = DIRECTION ( 'NONE',  ( -8.718379230999708359E-17, -0.7485107481710934207, 0.6631226582408039638 ) ) ;
#13284 = ADVANCED_FACE ( 'NONE', ( #7962 ), #20057, .T. ) ;
#13285 = PLANE ( 'NONE',  #32923 ) ;
#13286 = PLANE ( 'NONE',  #31420 ) ;
#13287 = ORIENTED_EDGE ( 'NONE', *, *, #22833, .T. ) ;
#13288 = VERTEX_POINT ( 'NONE', #39258 ) ;
#13290 = VERTEX_POINT ( 'NONE', #23740 ) ;
#13289 = CARTESIAN_POINT ( 'NONE',  ( -339.1964088526558498, -180.6659093959932250, 14.60509510167942437 ) ) ;
#13291 = ORIENTED_EDGE ( 'NONE', *, *, #10221, .F. ) ;
#13292 = AXIS2_PLACEMENT_3D ( 'NONE', #51140, #15124, #46401 ) ;
#13294 = STYLED_ITEM ( 'NONE', ( #19467 ), #36319 ) ;
#13293 = PLANE ( 'NONE',  #24964 ) ;
#13295 = CARTESIAN_POINT ( 'NONE',  ( -48.47912675150883643, -173.5000000000000284, -125.0000000000000000 ) ) ;
#13296 = AXIS2_PLACEMENT_3D ( 'NONE', #18702, #30518, #46062 ) ;
#13297 = CARTESIAN_POINT ( 'NONE',  ( 49.27559354810669845, -177.1207230881787780, -76.29032973288636299 ) ) ;
#13298 = DIRECTION ( 'NONE',  ( -0.9646355819083594074, 0.000000000000000000, 0.2635871660690647933 ) ) ;
#13299 = DIRECTION ( 'NONE',  ( 1.000000000000000000, -0.000000000000000000, -0.000000000000000000 ) ) ;
#13300 = ORIENTED_EDGE ( 'NONE', *, *, #42632, .F. ) ;
#13302 = EDGE_CURVE ( 'NONE', #48835, #43321, #47157, .T. ) ;
#13301 = CARTESIAN_POINT ( 'NONE',  ( -332.3517673607765914, -123.5000000000000284, 0.000000000000000000 ) ) ;
#13303 = EDGE_LOOP ( 'NONE', ( #4619, #17060, #35404, #45950 ) ) ;
#13304 = VERTEX_POINT ( 'NONE', #19535 ) ;
#13305 = CARTESIAN_POINT ( 'NONE',  ( -332.3517673607765914, -113.7752393642576720, 58.25253621232167944 ) ) ;
#13306 = VECTOR ( 'NONE', #30386, 1000.000000000000000 ) ;
#13307 = LINE ( 'NONE', #48793, #7710 ) ;
#13308 = ORIENTED_EDGE ( 'NONE', *, *, #20230, .T. ) ;
#13309 = ADVANCED_FACE ( 'NONE', ( #27936 ), #48184, .T. ) ;
#13310 = DIRECTION ( 'NONE',  ( -0.5085311186492216251, 0.000000000000000000, 0.8610436117673548884 ) ) ;
#13311 = FACE_OUTER_BOUND ( 'NONE', #32698, .T. ) ;
#13312 = CARTESIAN_POINT ( 'NONE',  ( -339.1964088526558498, -67.22367097967925531, -20.80804632820203182 ) ) ;
#13313 = FACE_OUTER_BOUND ( 'NONE', #2906, .T. ) ;
#13314 = PLANE ( 'NONE',  #3039 ) ;
#13315 = VECTOR ( 'NONE', #33064, 1000.000000000000000 ) ;
#13316 = ADVANCED_FACE ( 'NONE', ( #15876 ), #12153, .T. ) ;
#13317 = DIRECTION ( 'NONE',  ( -0.000000000000000000, -1.000000000000000000, 0.000000000000000000 ) ) ;
#13318 = CARTESIAN_POINT ( 'NONE',  ( -152.3176060415594861, -177.1207230881787780, -69.58857822034967455 ) ) ;
#13319 = VERTEX_POINT ( 'NONE', #11902 ) ;
#13320 = CARTESIAN_POINT ( 'NONE',  ( -339.1964088526558498, -66.09477493971894546, 13.63415328425207917 ) ) ;
#13321 = ORIENTED_EDGE ( 'NONE', *, *, #17550, .F. ) ;
#13322 = CARTESIAN_POINT ( 'NONE',  ( -147.8383830610225971, -183.6283474603465606, -74.18852968774183410 ) ) ;
#13323 = ORIENTED_EDGE ( 'NONE', *, *, #32392, .T. ) ;
#13324 = DIRECTION ( 'NONE',  ( 0.000000000000000000, -0.8854560256532126861, -0.4647231720437631775 ) ) ;
#13325 = EDGE_CURVE ( 'NONE', #50173, #40815, #24266, .T. ) ;
#13326 = EDGE_LOOP ( 'NONE', ( #11725, #26110, #1042, #8765 ) ) ;
#13327 = EDGE_CURVE ( 'NONE', #26701, #41833, #31622, .T. ) ;
#13328 = AXIS2_PLACEMENT_3D ( 'NONE', #27829, #39148, #3156 ) ;
#13329 = CARTESIAN_POINT ( 'NONE',  ( -144.0067397530739584, -193.5000000000000000, -80.61932246194587037 ) ) ;
#13330 = VECTOR ( 'NONE', #31580, 1000.000000000000000 ) ;
#13331 = EDGE_CURVE ( 'NONE', #6422, #43736, #23240, .T. ) ;
#13332 = STYLED_ITEM ( 'NONE', ( #33004 ), #36851 ) ;
#13333 = FACE_BOUND ( 'NONE', #33876, .T. ) ;
#13335 = ORIENTED_EDGE ( 'NONE', *, *, #9880, .F. ) ;
#13334 = LINE ( 'NONE', #25667, #7797 ) ;
#13336 = AXIS2_PLACEMENT_3D ( 'NONE', #23602, #3122, #15214 ) ;
#13337 = DIRECTION ( 'NONE',  ( -1.000000000000000000, 0.000000000000000000, 0.000000000000000000 ) ) ;
#13338 = ORIENTED_EDGE ( 'NONE', *, *, #9616, .F. ) ;
#13339 = VERTEX_POINT ( 'NONE', #3268 ) ;
#13340 = VERTEX_POINT ( 'NONE', #36083 ) ;
#13341 = DIRECTION ( 'NONE',  ( -0.2920567706369694982, 0.000000000000000000, -0.9564009842765243130 ) ) ;
#13342 = AXIS2_PLACEMENT_3D ( 'NONE', #188, #16237, #40915 ) ;
#13343 = DIRECTION ( 'NONE',  ( 0.000000000000000000, -1.000000000000000000, 0.000000000000000000 ) ) ;
#13344 = ORIENTED_EDGE ( 'NONE', *, *, #41657, .F. ) ;
#13345 = ADVANCED_FACE ( 'NONE', ( #7717 ), #19301, .F. ) ;
#13346 = DIRECTION ( 'NONE',  ( 0.000000000000000000, 1.000000000000000000, 0.000000000000000000 ) ) ;
#13347 = CARTESIAN_POINT ( 'NONE',  ( 76.48781641346532467, -189.7472609257535510, 2.874563619424056249 ) ) ;
#13348 = CARTESIAN_POINT ( 'NONE',  ( -330.4913330509368166, -96.52406086224361559, 52.47426709956096147 ) ) ;
#13349 = EDGE_LOOP ( 'NONE', ( #10341, #23795, #36305, #33524 ) ) ;
#13350 = AXIS2_PLACEMENT_3D ( 'NONE', #31188, #35383, #2814 ) ;
#13351 = LINE ( 'NONE', #12562, #26755 ) ;
#13352 = CARTESIAN_POINT ( 'NONE',  ( 46.00000000000000711, -43.50000000000000000, -46.00000000000000000 ) ) ;
#13353 = VERTEX_POINT ( 'NONE', #51360 ) ;
#13356 = VERTEX_POINT ( 'NONE', #15105 ) ;
#13355 = DIRECTION ( 'NONE',  ( 0.000000000000000000, 0.9927088740980527515, -0.1205366802553337890 ) ) ;
#13354 = DIRECTION ( 'NONE',  ( -0.05924062789372142729, 0.000000000000000000, 0.9982437317643209074 ) ) ;
#13357 = ORIENTED_EDGE ( 'NONE', *, *, #28179, .T. ) ;
#13358 = ORIENTED_EDGE ( 'NONE', *, *, #43214, .F. ) ;
#13359 = CARTESIAN_POINT ( 'NONE',  ( -48.47912675150885065, -177.1207230881787780, 6.938893903907228378E-15 ) ) ;
#13360 = VERTEX_POINT ( 'NONE', #19793 ) ;
#13361 = LINE ( 'NONE', #9417, #22140 ) ;
#13362 = CARTESIAN_POINT ( 'NONE',  ( -10.02015192278479816, -177.1207230881787780, -117.8859915627474493 ) ) ;
#13363 = VERTEX_POINT ( 'NONE', #31884 ) ;
#13364 = FACE_OUTER_BOUND ( 'NONE', #5796, .T. ) ;
#13365 = ORIENTED_EDGE ( 'NONE', *, *, #17072, .F. ) ;
#13366 = EDGE_LOOP ( 'NONE', ( #20291, #22411, #25181, #48559 ) ) ;
#13367 = DIRECTION ( 'NONE',  ( 0.000000000000000000, -1.000000000000000000, 0.000000000000000000 ) ) ;
#13368 = LINE ( 'NONE', #5237, #46577 ) ;
#13369 = VECTOR ( 'NONE', #21276, 1000.000000000000000 ) ;
#13370 = DIRECTION ( 'NONE',  ( 0.000000000000000000, -0.8229838658936596829, -0.5680647467311510379 ) ) ;
#13371 = DIRECTION ( 'NONE',  ( -0.000000000000000000, 1.000000000000000000, -0.000000000000000000 ) ) ;
#13372 = ORIENTED_EDGE ( 'NONE', *, *, #4725, .T. ) ;
#13373 = LINE ( 'NONE', #6262, #30956 ) ;
#13374 = VECTOR ( 'NONE', #21998, 1000.000000000000000 ) ;
#13375 = CARTESIAN_POINT ( 'NONE',  ( 15.80042947435468470, -193.5000000000000000, 107.2060569716377927 ) ) ;
#13376 = EDGE_CURVE ( 'NONE', #19012, #11792, #3764, .T. ) ;
#13377 = EDGE_CURVE ( 'NONE', #26105, #1712, #845, .T. ) ;
#13378 = CARTESIAN_POINT ( 'NONE',  ( -180.0000000000000568, -155.0173647354142759, 14.76740078976490622 ) ) ;
#13379 = CARTESIAN_POINT ( 'NONE',  ( 72.14504940832446778, -175.3837268820161057, -32.78426643622660208 ) ) ;
#13380 = LINE ( 'NONE', #48872, #28847 ) ;
#13381 = FACE_OUTER_BOUND ( 'NONE', #8308, .T. ) ;
#13382 = DIRECTION ( 'NONE',  ( 0.000000000000000000, 0.000000000000000000, 1.000000000000000000 ) ) ;
#13383 = VERTEX_POINT ( 'NONE', #43966 ) ;
#13384 = EDGE_LOOP ( 'NONE', ( #32411, #36902, #21700, #43416 ) ) ;
#13385 = CARTESIAN_POINT ( 'NONE',  ( -88.49718702276007321, -183.6283474603465606, -117.3655938605927673 ) ) ;
#13386 = LINE ( 'NONE', #45207, #26249 ) ;
#13387 = VERTEX_POINT ( 'NONE', #43468 ) ;
#13388 = DIRECTION ( 'NONE',  ( -0.5586467658036415873, 0.000000000000000000, -0.8294056854502090959 ) ) ;
#13389 = ADVANCED_FACE ( 'NONE', ( #35825 ), #47922, .T. ) ;
#13390 = ORIENTED_EDGE ( 'NONE', *, *, #20390, .T. ) ;
#13391 = EDGE_CURVE ( 'NONE', #33271, #22773, #13216, .T. ) ;
#13392 = AXIS2_PLACEMENT_3D ( 'NONE', #2110, #5833, #10022 ) ;
#13393 = DIRECTION ( 'NONE',  ( 0.000000000000000000, -0.000000000000000000, 1.000000000000000000 ) ) ;
#13394 = EDGE_CURVE ( 'NONE', #7329, #5830, #32394, .T. ) ;
#13395 = DIRECTION ( 'NONE',  ( -0.6965510290629882695, 0.000000000000000000, -0.7175072570443395970 ) ) ;
#13396 = LINE ( 'NONE', #29409, #31263 ) ;
#13397 = LINE ( 'NONE', #33097, #20356 ) ;
#13398 = ADVANCED_FACE ( 'NONE', ( #28448 ), #8738, .F. ) ;
#13399 = ORIENTED_EDGE ( 'NONE', *, *, #44171, .T. ) ;
#13400 = FACE_OUTER_BOUND ( 'NONE', #7721, .T. ) ;
#13401 = VERTEX_POINT ( 'NONE', #29240 ) ;
#13402 = CARTESIAN_POINT ( 'NONE',  ( -166.1003692892502102, -183.6283474603465606, -42.31126686685033889 ) ) ;
#13403 = ORIENTED_EDGE ( 'NONE', *, *, #3657, .F. ) ;
#13404 = CARTESIAN_POINT ( 'NONE',  ( -49.29161362951452929, -193.5000000000000000, -0.5829794791144748967 ) ) ;
#13405 = AXIS2_PLACEMENT_3D ( 'NONE', #50622, #34331, #14360 ) ;
#13406 = ORIENTED_EDGE ( 'NONE', *, *, #31081, .F. ) ;
#13407 = DIRECTION ( 'NONE',  ( -1.000000000000000000, -0.000000000000000000, -0.000000000000000000 ) ) ;
#13408 = EDGE_LOOP ( 'NONE', ( #28139, #27807, #19325, #18987 ) ) ;
#13409 = CARTESIAN_POINT ( 'NONE',  ( 9.518239912201957864, -213.5000000000000000, 110.7307791902283043 ) ) ;
#13410 = DIRECTION ( 'NONE',  ( -0.000000000000000000, 1.000000000000000000, -0.000000000000000000 ) ) ;
#13411 = ORIENTED_EDGE ( 'NONE', *, *, #25650, .F. ) ;
#13414 = ORIENTED_EDGE ( 'NONE', *, *, #16236, .T. ) ;
#13413 = DIRECTION ( 'NONE',  ( -0.000000000000000000, 0.3546048870425463906, 0.9350162426854107256 ) ) ;
#13412 = CARTESIAN_POINT ( 'NONE',  ( -29.85296035031868911, -193.5000000000000000, 122.5936119678275702 ) ) ;
#13415 = FACE_OUTER_BOUND ( 'NONE', #50016, .T. ) ;
#13416 = VERTEX_POINT ( 'NONE', #24511 ) ;
#13417 = DIRECTION ( 'NONE',  ( 0.1182731709213592358, 0.000000000000000000, 0.9929810960135178055 ) ) ;
#13418 = ORIENTED_EDGE ( 'NONE', *, *, #31823, .T. ) ;
#13419 = DIRECTION ( 'NONE',  ( -1.000000000000000000, -0.000000000000000000, 0.000000000000000000 ) ) ;
#13422 = ORIENTED_EDGE ( 'NONE', *, *, #50690, .T. ) ;
#13421 = DIRECTION ( 'NONE',  ( 1.000000000000000000, 0.000000000000000000, -0.000000000000000000 ) ) ;
#13420 = CARTESIAN_POINT ( 'NONE',  ( 24.88090138098523241, -177.1207230881787780, 99.97252634603304955 ) ) ;
#13423 = VERTEX_POINT ( 'NONE', #8478 ) ;
#13424 = AXIS2_PLACEMENT_3D ( 'NONE', #43526, #39318, #35897 ) ;
#13425 = VECTOR ( 'NONE', #20616, 1000.000000000000000 ) ;
#13426 = ADVANCED_FACE ( 'NONE', ( #25549 ), #1383, .T. ) ;
#13427 = DIRECTION ( 'NONE',  ( 0.000000000000000000, -1.000000000000000000, 0.000000000000000000 ) ) ;
#13428 = CARTESIAN_POINT ( 'NONE',  ( -130.7087404384255080, -189.7472609257535510, -94.14505102712755047 ) ) ;
#13429 = DIRECTION ( 'NONE',  ( 0.000000000000000000, -1.000000000000000000, 0.000000000000000000 ) ) ;
#13430 = ORIENTED_EDGE ( 'NONE', *, *, #30055, .F. ) ;
#13431 = CARTESIAN_POINT ( 'NONE',  ( 26.10278175629141018, -189.7472609257535510, -99.06333546307678262 ) ) ;
#13432 = CYLINDRICAL_SURFACE ( 'NONE', #46697, 125.0000000000000000 ) ;
#13433 = CARTESIAN_POINT ( 'NONE',  ( -305.0000000000000568, -130.2355952558269223, -59.62073260661665586 ) ) ;
#13434 = DIRECTION ( 'NONE',  ( -0.9993908270190956511, 0.000000000000000000, 0.03489949670250096919 ) ) ;
#13435 = EDGE_CURVE ( 'NONE', #44829, #21855, #25210, .T. ) ;
#13436 = EDGE_CURVE ( 'NONE', #7246, #45277, #40530, .T. ) ;
#13437 = ORIENTED_EDGE ( 'NONE', *, *, #51660, .T. ) ;
#13438 = EDGE_CURVE ( 'NONE', #22275, #16038, #36339, .T. ) ;
#13439 = LINE ( 'NONE', #33140, #45615 ) ;
#13440 = CARTESIAN_POINT ( 'NONE',  ( 9.518239912201957864, -213.5000000000000000, -110.7307791902283043 ) ) ;
#13441 = EDGE_CURVE ( 'NONE', #20535, #8894, #16382, .T. ) ;
#13442 = CARTESIAN_POINT ( 'NONE',  ( -339.1964088526558498, -168.7406467949202806, 39.41172259083927543 ) ) ;
#13443 = ORIENTED_EDGE ( 'NONE', *, *, #2155, .F. ) ;
#13444 = VECTOR ( 'NONE', #2654, 1000.000000000000000 ) ;
#13445 = DIRECTION ( 'NONE',  ( -1.000000000000000000, 0.000000000000000000, 0.000000000000000000 ) ) ;
#13446 = EDGE_CURVE ( 'NONE', #14916, #27618, #45539, .T. ) ;
#13447 = DIRECTION ( 'NONE',  ( 0.000000000000000000, 0.8229838658936516893, -0.5680647467311626952 ) ) ;
#13448 = PLANE ( 'NONE',  #49563 ) ;
#13449 = CARTESIAN_POINT ( 'NONE',  ( -170.0000000000000284, -123.5000000000000284, 37.63467731922665394 ) ) ;
#13450 = EDGE_CURVE ( 'NONE', #45109, #31967, #41314, .T. ) ;
#13451 = ADVANCED_FACE ( 'NONE', ( #32908 ), #25297, .T. ) ;
#13452 = CARTESIAN_POINT ( 'NONE',  ( -339.1964088526558498, -144.8891964568526305, -54.98865587491811624 ) ) ;
#13453 = EDGE_CURVE ( 'NONE', #30392, #44484, #17436, .T. ) ;
#13454 = DIRECTION ( 'NONE',  ( 0.9960498426152165630, 0.000000000000000000, 0.08879589532293852283 ) ) ;
#13455 = CARTESIAN_POINT ( 'NONE',  ( -336.3521761649654422, -177.7994952405510389, -25.52576769896207054 ) ) ;
#13457 = ORIENTED_EDGE ( 'NONE', *, *, #3377, .T. ) ;
#13456 = DIRECTION ( 'NONE',  ( 0.000000000000000000, -0.000000000000000000, 1.000000000000000000 ) ) ;
#13458 = ADVANCED_FACE ( 'NONE', ( #28699 ), #44755, .F. ) ;
#13459 = ORIENTED_EDGE ( 'NONE', *, *, #25265, .F. ) ;
#13460 = LINE ( 'NONE', #45013, #3088 ) ;
#13461 = ADVANCED_FACE ( 'NONE', ( #49499 ), #4820, .T. ) ;
#13462 = AXIS2_PLACEMENT_3D ( 'NONE', #29485, #36870, #32662 ) ;
#13463 = AXIS2_PLACEMENT_3D ( 'NONE', #14813, #30828, #46875 ) ;
#13464 = CARTESIAN_POINT ( 'NONE',  ( -180.0000000000000568, -115.7896721143442278, -18.45401972188387418 ) ) ;
#13466 = ORIENTED_EDGE ( 'NONE', *, *, #28496, .F. ) ;
#13465 = FACE_OUTER_BOUND ( 'NONE', #8291, .T. ) ;
#13467 = ORIENTED_EDGE ( 'NONE', *, *, #40053, .T. ) ;
#13468 = ORIENTED_EDGE ( 'NONE', *, *, #35982, .T. ) ;
#13469 = FACE_OUTER_BOUND ( 'NONE', #46887, .T. ) ;
#13470 = DIRECTION ( 'NONE',  ( -0.9890401873221654760, 0.000000000000000000, 0.1476465640024710868 ) ) ;
#13471 = FACE_OUTER_BOUND ( 'NONE', #49867, .T. ) ;
#13472 = ORIENTED_EDGE ( 'NONE', *, *, #3146, .F. ) ;
#13473 = ADVANCED_FACE ( 'NONE', ( #12935 ), #45028, .T. ) ;
#13474 = CARTESIAN_POINT ( 'NONE',  ( -18.31235070009513421, -189.7472609257535510, 121.3052580173829966 ) ) ;
#13476 = ORIENTED_EDGE ( 'NONE', *, *, #13522, .T. ) ;
#13475 = DIRECTION ( 'NONE',  ( 0.000000000000000000, 0.000000000000000000, -1.000000000000000000 ) ) ;
#13477 = VECTOR ( 'NONE', #46959, 1000.000000000000000 ) ;
#13478 = FACE_OUTER_BOUND ( 'NONE', #26133, .T. ) ;
#13479 = EDGE_LOOP ( 'NONE', ( #4727, #26591, #46433, #31282 ) ) ;
#13480 = CARTESIAN_POINT ( 'NONE',  ( -305.0000000000000568, -170.1129345408508868, -37.77875505479702412 ) ) ;
#13481 = ORIENTED_EDGE ( 'NONE', *, *, #42109, .T. ) ;
#13482 = FACE_OUTER_BOUND ( 'NONE', #47911, .T. ) ;
#13483 = FACE_OUTER_BOUND ( 'NONE', #47599, .T. ) ;
#13484 = CARTESIAN_POINT ( 'NONE',  ( -336.3521761649654422, -133.2247606357419443, -58.25253621232173629 ) ) ;
#13485 = ORIENTED_EDGE ( 'NONE', *, *, #12934, .F. ) ;
#13486 = ORIENTED_EDGE ( 'NONE', *, *, #9529, .T. ) ;
#13487 = LINE ( 'NONE', #29505, #448 ) ;
#13488 = CARTESIAN_POINT ( 'NONE',  ( -336.3521761649654422, -149.4733471526596134, 53.00046796564699036 ) ) ;
#13489 = VERTEX_POINT ( 'NONE', #5077 ) ;
#13490 = CARTESIAN_POINT ( 'NONE',  ( -332.3517673607765914, -155.6724726690323450, 49.48329383994676078 ) ) ;
#13491 = VECTOR ( 'NONE', #43493, 1000.000000000000000 ) ;
#13492 = ADVANCED_FACE ( 'NONE', ( #17158 ), #33175, .T. ) ;
#13493 = ADVANCED_FACE ( 'NONE', ( #18709 ), #42619, .F. ) ;
#13494 = ORIENTED_EDGE ( 'NONE', *, *, #44666, .F. ) ;
#13495 = DIRECTION ( 'NONE',  ( 0.000000000000000000, 0.000000000000000000, 1.000000000000000000 ) ) ;
#13496 = CARTESIAN_POINT ( 'NONE',  ( -336.3521761649654422, -182.5000000000000568, 1.632288850093980725 ) ) ;
#13497 = VECTOR ( 'NONE', #17937, 1000.000000000000000 ) ;
#13498 = EDGE_CURVE ( 'NONE', #12238, #27379, #6792, .T. ) ;
#13499 = AXIS2_PLACEMENT_3D ( 'NONE', #32574, #25215, #5251 ) ;
#13500 = EDGE_CURVE ( 'NONE', #44345, #18213, #38417, .T. ) ;
#13501 = ORIENTED_EDGE ( 'NONE', *, *, #12114, .F. ) ;
#13502 = FACE_OUTER_BOUND ( 'NONE', #3188, .T. ) ;
#13503 = ORIENTED_EDGE ( 'NONE', *, *, #18878, .T. ) ;
#13504 = DIRECTION ( 'NONE',  ( -1.000000000000000000, -0.000000000000000000, 0.000000000000000000 ) ) ;
#13505 = DIRECTION ( 'NONE',  ( 0.1476465640024710868, 0.000000000000000000, 0.9890401873221654760 ) ) ;
#13506 = EDGE_LOOP ( 'NONE', ( #48352, #10564, #45191, #12664 ) ) ;
#13507 = DIRECTION ( 'NONE',  ( -0.000000000000000000, 1.000000000000000000, -0.000000000000000000 ) ) ;
#13508 = CARTESIAN_POINT ( 'NONE',  ( -27.18512803868276251, -193.5000000000000000, -123.1729094355498404 ) ) ;
#13509 = LINE ( 'NONE', #29274, #28244 ) ;
#13510 = LINE ( 'NONE', #39158, #25749 ) ;
#13511 = VERTEX_POINT ( 'NONE', #2151 ) ;
#13512 = DIRECTION ( 'NONE',  ( 0.5085311186492154079, 0.000000000000000000, 0.8610436117673585521 ) ) ;
#13513 = VERTEX_POINT ( 'NONE', #1652 ) ;
#13514 = VERTEX_POINT ( 'NONE', #6119 ) ;
#13515 = AXIS2_PLACEMENT_3D ( 'NONE', #1961, #34014, #29023 ) ;
#13516 = EDGE_CURVE ( 'NONE', #3140, #32119, #35282, .T. ) ;
#13517 = DIRECTION ( 'NONE',  ( 0.000000000000000000, -0.7485107481710934207, 0.6631226582408039638 ) ) ;
#13519 = VERTEX_POINT ( 'NONE', #42352 ) ;
#13518 = CARTESIAN_POINT ( 'NONE',  ( -69.59623518921151231, -175.3837268820161057, 122.1886788576023974 ) ) ;
#13520 = ORIENTED_EDGE ( 'NONE', *, *, #10646, .T. ) ;
#13521 = DIRECTION ( 'NONE',  ( -0.000000000000000000, 1.000000000000000000, -0.000000000000000000 ) ) ;
#13522 = EDGE_CURVE ( 'NONE', #10774, #6991, #22395, .T. ) ;
#13523 = CARTESIAN_POINT ( 'NONE',  ( 68.72094416275764672, -193.5000000000000000, -40.49875167738977666 ) ) ;
#13524 = EDGE_LOOP ( 'NONE', ( #13265, #33337, #16856, #41689 ) ) ;
#13525 = CARTESIAN_POINT ( 'NONE',  ( -104.3615810019516772, -193.5000000000000000, 110.6939782313525455 ) ) ;
#13526 = VERTEX_POINT ( 'NONE', #34222 ) ;
#13527 = CARTESIAN_POINT ( 'NONE',  ( -47.53180039765466347, -193.5000000000000000, 0.3202698538628485636 ) ) ;
#13528 = DIRECTION ( 'NONE',  ( 0.000000000000000000, 1.000000000000000000, -0.000000000000000000 ) ) ;
#13529 = AXIS2_PLACEMENT_3D ( 'NONE', #53, #12910, #24235 ) ;
#13530 = DIRECTION ( 'NONE',  ( 0.000000000000000000, 0.000000000000000000, -1.000000000000000000 ) ) ;
#13531 = CARTESIAN_POINT ( 'NONE',  ( -48.47912675150885065, -183.6283474603465606, 6.938893903907228378E-15 ) ) ;
#13532 = ORIENTED_EDGE ( 'NONE', *, *, #18375, .T. ) ;
#13533 = ORIENTED_EDGE ( 'NONE', *, *, #7502, .F. ) ;
#13535 = ORIENTED_EDGE ( 'NONE', *, *, #38410, .T. ) ;
#13534 = AXIS2_PLACEMENT_3D ( 'NONE', #20160, #48024, #8080 ) ;
#13536 = DIRECTION ( 'NONE',  ( 0.000000000000000000, 0.000000000000000000, 1.000000000000000000 ) ) ;
#13537 = CARTESIAN_POINT ( 'NONE',  ( -305.0000000000000568, -67.22367097967925531, -20.80804632820203182 ) ) ;
#13538 = DIRECTION ( 'NONE',  ( 0.2059786187411021818, 0.000000000000000000, -0.9785564922995032555 ) ) ;
#13539 = PLANE ( 'NONE',  #46558 ) ;
#13540 = VERTEX_POINT ( 'NONE', #10055 ) ;
#13541 = EDGE_CURVE ( 'NONE', #21790, #21281, #14256, .T. ) ;
#13542 = ORIENTED_EDGE ( 'NONE', *, *, #26102, .F. ) ;
#13544 = VERTEX_POINT ( 'NONE', #38665 ) ;
#13543 = DIRECTION ( 'NONE',  ( 0.000000000000000000, 0.9709418174260502354, -0.2393156642875652051 ) ) ;
#13545 = VERTEX_POINT ( 'NONE', #18454 ) ;
#13546 = AXIS2_PLACEMENT_3D ( 'NONE', #14312, #31101, #6691 ) ;
#13547 = FACE_OUTER_BOUND ( 'NONE', #35434, .T. ) ;
#13548 = LINE ( 'NONE', #5685, #13239 ) ;
#13549 = CARTESIAN_POINT ( 'NONE',  ( -168.0489871616337325, -175.3837268820161057, -32.84887689123905119 ) ) ;
#13550 = EDGE_CURVE ( 'NONE', #13353, #22103, #27737, .T. ) ;
#13552 = EDGE_CURVE ( 'NONE', #22586, #17429, #30019, .T. ) ;
#13551 = CARTESIAN_POINT ( 'NONE',  ( -330.4913330509368166, -156.6043281241916816, -48.84008046109114076 ) ) ;
#13553 = ORIENTED_EDGE ( 'NONE', *, *, #22747, .F. ) ;
#13554 = LINE ( 'NONE', #49829, #49355 ) ;
#13555 = ORIENTED_EDGE ( 'NONE', *, *, #9284, .T. ) ;
#13556 = APPLICATION_CONTEXT ( 'automotive_design' ) ;
#13557 = ORIENTED_EDGE ( 'NONE', *, *, #30832, .T. ) ;
#13558 = DIRECTION ( 'NONE',  ( -1.000000000000000000, -0.000000000000000000, -0.000000000000000000 ) ) ;
#13559 = CARTESIAN_POINT ( 'NONE',  ( -88.23625491228467865, -177.1207230881787780, 118.5089480183148254 ) ) ;
#13560 = ORIENTED_EDGE ( 'NONE', *, *, #3448, .T. ) ;
#13561 = VECTOR ( 'NONE', #16163, 999.9999999999998863 ) ;
#13562 = DIRECTION ( 'NONE',  ( -0.000000000000000000, 0.9927088740980556381, 0.1205366802553095307 ) ) ;
#13563 = LINE ( 'NONE', #21191, #21334 ) ;
#13564 = PLANE ( 'NONE',  #27899 ) ;
#13565 = VECTOR ( 'NONE', #2260, 1000.000000000000000 ) ;
#13566 = CARTESIAN_POINT ( 'NONE',  ( -339.1964088526558498, -123.5000000000000284, 0.000000000000000000 ) ) ;
#13567 = AXIS2_PLACEMENT_3D ( 'NONE', #21071, #1092, #21337 ) ;
#13568 = DIRECTION ( 'NONE',  ( 1.000000000000000000, 1.050884489711663158E-17, 8.654812430365575371E-17 ) ) ;
#13569 = FACE_BOUND ( 'NONE', #19373, .T. ) ;
#13570 = ORIENTED_EDGE ( 'NONE', *, *, #6016, .T. ) ;
#13571 = EDGE_CURVE ( 'NONE', #32376, #5586, #27631, .T. ) ;
#13572 = CARTESIAN_POINT ( 'NONE',  ( -47.51449116960048968, -193.5000000000000000, -0.2635871660690578544 ) ) ;
#13573 = ORIENTED_EDGE ( 'NONE', *, *, #14342, .T. ) ;
#13574 = ORIENTED_EDGE ( 'NONE', *, *, #6041, .F. ) ;
#13575 = DIRECTION ( 'NONE',  ( -0.000000000000000000, 1.000000000000000000, -0.000000000000000000 ) ) ;
#13576 = ORIENTED_EDGE ( 'NONE', *, *, #30111, .F. ) ;
#13577 = VECTOR ( 'NONE', #32891, 1000.000000000000000 ) ;
#13578 = EDGE_CURVE ( 'NONE', #1973, #31995, #30524, .T. ) ;
#13579 = DIRECTION ( 'NONE',  ( 0.000000000000000000, 0.000000000000000000, 1.000000000000000000 ) ) ;
#13580 = VECTOR ( 'NONE', #30645, 1000.000000000000000 ) ;
#13581 = DIRECTION ( 'NONE',  ( 0.000000000000000000, -1.000000000000000000, -0.000000000000000000 ) ) ;
#13583 = ORIENTED_EDGE ( 'NONE', *, *, #4402, .T. ) ;
#13582 = CARTESIAN_POINT ( 'NONE',  ( -330.4913330509368166, -167.3305728129748786, -39.49849221029221269 ) ) ;
#13584 = EDGE_CURVE ( 'NONE', #41636, #12238, #38653, .T. ) ;
#13585 = CARTESIAN_POINT ( 'NONE',  ( -9.671950287350391307, -183.6283474603465606, -118.8234112238815499 ) ) ;
#13586 = ORIENTED_EDGE ( 'NONE', *, *, #13978, .T. ) ;
#13587 = EDGE_LOOP ( 'NONE', ( #40309, #11978, #34632, #36777 ) ) ;
#13588 = ORIENTED_EDGE ( 'NONE', *, *, #47967, .F. ) ;
#13589 = CARTESIAN_POINT ( 'NONE',  ( -48.18706998087187543, -189.7472609257535510, -0.9564009842765152092 ) ) ;
#13590 = CARTESIAN_POINT ( 'NONE',  ( -47.92047998570519951, -177.1207230881787780, -0.8294056854501942189 ) ) ;
#13591 = ORIENTED_EDGE ( 'NONE', *, *, #28788, .F. ) ;
#13592 = DIRECTION ( 'NONE',  ( 0.7765238627180393038, 0.000000000000000000, 0.6300878435817147682 ) ) ;
#13593 = DIRECTION ( 'NONE',  ( 0.000000000000000000, 1.410908427127803051E-14, -1.000000000000000000 ) ) ;
#13594 = LINE ( 'NONE', #4954, #13769 ) ;
#13595 = AXIS2_PLACEMENT_3D ( 'NONE', #37606, #49177, #21314 ) ;
#13596 = ORIENTED_EDGE ( 'NONE', *, *, #34108, .T. ) ;
#13597 = AXIS2_PLACEMENT_3D ( 'NONE', #4855, #28991, #44522 ) ;
#13598 = VECTOR ( 'NONE', #28370, 1000.000000000000000 ) ;
#13599 = EDGE_CURVE ( 'NONE', #8154, #29294, #5603, .T. ) ;
#13600 = CARTESIAN_POINT ( 'NONE',  ( -170.0000000000000284, -123.5000000000000284, -45.63467731922664683 ) ) ;
#13601 = DIRECTION ( 'NONE',  ( -1.000000000000000000, 0.000000000000000000, -0.000000000000000000 ) ) ;
#13602 = ORIENTED_EDGE ( 'NONE', *, *, #20807, .T. ) ;
#13604 = EDGE_LOOP ( 'NONE', ( #5347, #38768, #49800, #12529 ) ) ;
#13603 = LINE ( 'NONE', #30152, #32345 ) ;
#13605 = ORIENTED_EDGE ( 'NONE', *, *, #32772, .T. ) ;
#13606 = ORIENTED_EDGE ( 'NONE', *, *, #6593, .T. ) ;
#13607 = DIRECTION ( 'NONE',  ( -1.000000000000000000, 0.000000000000000000, 0.000000000000000000 ) ) ;
#13608 = CARTESIAN_POINT ( 'NONE',  ( -339.1964088526558498, -156.6043281241916816, -48.84008046109114076 ) ) ;
#13609 = ORIENTED_EDGE ( 'NONE', *, *, #4906, .T. ) ;
#13610 = CYLINDRICAL_SURFACE ( 'NONE', #6167, 125.0000000000000000 ) ;
#13611 = ADVANCED_FACE ( 'NONE', ( #33946 ), #14516, .T. ) ;
#13612 = CARTESIAN_POINT ( 'NONE',  ( -173.0003472773501301, -189.7472609257535510, 10.93003379476953896 ) ) ;
#13613 = EDGE_LOOP ( 'NONE', ( #16565, #29025, #14364, #19222 ) ) ;
#13614 = EDGE_CURVE ( 'NONE', #46248, #9912, #26069, .T. ) ;
#13615 = CARTESIAN_POINT ( 'NONE',  ( -332.3517673607765914, -136.2687678316390532, 58.62557946887775273 ) ) ;
#13616 = ORIENTED_EDGE ( 'NONE', *, *, #34591, .T. ) ;
#13617 = VECTOR ( 'NONE', #41233, 1000.000000000000114 ) ;
#13618 = ORIENTED_EDGE ( 'NONE', *, *, #28215, .F. ) ;
#13619 = DIRECTION ( 'NONE',  ( 0.000000000000000000, 9.598803233738333010E-14, 1.000000000000000000 ) ) ;
#13620 = VECTOR ( 'NONE', #25207, 999.9999999999998863 ) ;
#13621 = EDGE_CURVE ( 'NONE', #47039, #32136, #6368, .T. ) ;
#13623 = CIRCLE ( 'NONE', #42986, 60.00000000000000000 ) ;
#13622 = CARTESIAN_POINT ( 'NONE',  ( 14.72514937628683640, -189.7472609257535510, -106.6827995071083706 ) ) ;
#13624 = CARTESIAN_POINT ( 'NONE',  ( -49.29161362951452929, -183.6283474603465606, -0.5829794791144748967 ) ) ;
#13625 = LINE ( 'NONE', #25970, #21534 ) ;
#13626 = ORIENTED_EDGE ( 'NONE', *, *, #35004, .F. ) ;
#13627 = CARTESIAN_POINT ( 'NONE',  ( -365.0160704661291788, -93.50000000000001421, -51.54700538379269403 ) ) ;
#13628 = LINE ( 'NONE', #41750, #25592 ) ;
#13629 = ITEM_DEFINED_TRANSFORMATION ( 'NONE', 'NONE', #5778,  #31742 ) ;
#13630 = CARTESIAN_POINT ( 'NONE',  ( -330.4913330509368166, -83.33976666099020747, -44.57752413667996194 ) ) ;
#13631 = DIRECTION ( 'NONE',  ( -0.8455960035018311727, 0.000000000000000000, 0.5338233779647826305 ) ) ;
#13632 = ORIENTED_EDGE ( 'NONE', *, *, #28284, .T. ) ;
#13633 = LINE ( 'NONE', #12845, #22154 ) ;
#13634 = DIRECTION ( 'NONE',  ( -0.000000000000000000, 1.000000000000000000, -0.000000000000000000 ) ) ;
#13635 = DIRECTION ( 'NONE',  ( -0.9720229140804139689, 0.000000000000000000, 0.2348860457809708036 ) ) ;
#13636 = ORIENTED_EDGE ( 'NONE', *, *, #21463, .T. ) ;
#13637 = VERTEX_POINT ( 'NONE', #46573 ) ;
#13638 = EDGE_CURVE ( 'NONE', #5249, #35097, #26328, .T. ) ;
#13639 = AXIS2_PLACEMENT_3D ( 'NONE', #7364, #12313, #24413 ) ;
#13640 = CARTESIAN_POINT ( 'NONE',  ( -169.6719064342497632, -183.6283474603465606, 30.61552143554992256 ) ) ;
#13641 = CARTESIAN_POINT ( 'NONE',  ( 40.29886924377099433, 30.00000000000000355, -46.21030057994576623 ) ) ;
#13642 = ORIENTED_EDGE ( 'NONE', *, *, #47140, .F. ) ;
#13643 = CARTESIAN_POINT ( 'NONE',  ( -98.71382891444399377, -193.5000000000000000, -114.4616734920523555 ) ) ;
#13644 = ORIENTED_EDGE ( 'NONE', *, *, #25660, .T. ) ;
#13645 = VECTOR ( 'NONE', #24436, 1000.000000000000000 ) ;
#13646 = FACE_OUTER_BOUND ( 'NONE', #12537, .T. ) ;
#13647 = FACE_OUTER_BOUND ( 'NONE', #24347, .T. ) ;
#13648 = DIRECTION ( 'NONE',  ( 0.000000000000000000, 0.000000000000000000, -1.000000000000000000 ) ) ;
#13649 = DIRECTION ( 'NONE',  ( 0.000000000000000000, 0.000000000000000000, 1.000000000000000000 ) ) ;
#13650 = LINE ( 'NONE', #17358, #29157 ) ;
#13651 = DIRECTION ( 'NONE',  ( -0.8757349421956310831, 0.000000000000000000, -0.4827922027307550712 ) ) ;
#13652 = AXIS2_PLACEMENT_3D ( 'NONE', #9983, #2067, #13649 ) ;
#13653 = ORIENTED_EDGE ( 'NONE', *, *, #43262, .T. ) ;
#13654 = AXIS2_PLACEMENT_3D ( 'NONE', #5100, #24284, #33197 ) ;
#13655 = LINE ( 'NONE', #12872, #19746 ) ;
#13656 = ORIENTED_EDGE ( 'NONE', *, *, #17988, .F. ) ;
#13657 = CARTESIAN_POINT ( 'NONE',  ( -339.1964088526558498, -167.3305728129742249, 39.49849221029288060 ) ) ;
#13658 = VECTOR ( 'NONE', #47768, 1000.000000000000114 ) ;
#13659 = VECTOR ( 'NONE', #4551, 1000.000000000000114 ) ;
#13660 = EDGE_LOOP ( 'NONE', ( #3303, #41834, #49728, #24493 ) ) ;
#13661 = CARTESIAN_POINT ( 'NONE',  ( -180.0000000000000568, -123.5000000000000284, 41.63467731922665394 ) ) ;
#13662 = ADVANCED_FACE ( 'NONE', ( #51289 ), #3198, .F. ) ;
#13663 = VERTEX_POINT ( 'NONE', #35754 ) ;
#13664 = EDGE_CURVE ( 'NONE', #43748, #19848, #32775, .T. ) ;
#13665 = AXIS2_PLACEMENT_3D ( 'NONE', #22577, #10463, #19142 ) ;
#13666 = DIRECTION ( 'NONE',  ( 0.000000000000000000, 0.9709418174260519008, -0.2393156642875582940 ) ) ;
#13667 = PLANE ( 'NONE',  #3071 ) ;
#13668 = ORIENTED_EDGE ( 'NONE', *, *, #37586, .F. ) ;
#13671 = ORIENTED_EDGE ( 'NONE', *, *, #7691, .T. ) ;
#13670 = CARTESIAN_POINT ( 'NONE',  ( 52.75081385575904136, -193.5000000000000000, 71.61357856150600298 ) ) ;
#13669 = CARTESIAN_POINT ( 'NONE',  ( -330.4913330509368166, -157.1712093821534211, -49.66134974749665076 ) ) ;
#13672 = CARTESIAN_POINT ( 'NONE',  ( -332.3517673607765914, -64.50000000000000000, -2.632288850093980503 ) ) ;
#13673 = EDGE_LOOP ( 'NONE', ( #38678, #41141, #40067, #8335 ) ) ;
#13674 = CARTESIAN_POINT ( 'NONE',  ( -137.2624501260119985, -193.5000000000000000, 87.99159897727967916 ) ) ;
#13675 = VECTOR ( 'NONE', #8064, 1000.000000000000000 ) ;
#13676 = ORIENTED_EDGE ( 'NONE', *, *, #41659, .T. ) ;
#13677 = EDGE_CURVE ( 'NONE', #15110, #36975, #26055, .T. ) ;
#13678 = LINE ( 'NONE', #21833, #20859 ) ;
#13681 = ORIENTED_EDGE ( 'NONE', *, *, #10878, .T. ) ;
#13680 = CARTESIAN_POINT ( 'NONE',  ( -58.29063029684667896, -177.1207230881787780, 124.6143426664034735 ) ) ;
#13679 = LINE ( 'NONE', #25250, #35853 ) ;
#13682 = ORIENTED_EDGE ( 'NONE', *, *, #38410, .F. ) ;
#13683 = EDGE_CURVE ( 'NONE', #22697, #18236, #58, .T. ) ;
#13684 = VECTOR ( 'NONE', #1161, 1000.000000000000000 ) ;
#13685 = DIRECTION ( 'NONE',  ( 0.000000000000000000, 0.000000000000000000, 1.000000000000000000 ) ) ;
#13686 = DIRECTION ( 'NONE',  ( 0.000000000000000000, 0.000000000000000000, -1.000000000000000000 ) ) ;
#13687 = EDGE_CURVE ( 'NONE', #16507, #1774, #23926, .T. ) ;
#13688 = DIRECTION ( 'NONE',  ( 0.000000000000000000, 0.000000000000000000, -1.000000000000000000 ) ) ;
#13689 = VERTEX_POINT ( 'NONE', #47344 ) ;
#13690 = DIRECTION ( 'NONE',  ( 0.2059786187411021818, 0.000000000000000000, -0.9785564922995032555 ) ) ;
#13691 = LINE ( 'NONE', #46031, #8126 ) ;
#13692 = CARTESIAN_POINT ( 'NONE',  ( -92.78132261338707565, -193.5000000000000000, -116.8859077982276773 ) ) ;
#13693 = DIRECTION ( 'NONE',  ( -0.000000000000000000, 1.000000000000000000, -0.000000000000000000 ) ) ;
#13694 = ORIENTED_EDGE ( 'NONE', *, *, #22622, .T. ) ;
#13695 = AXIS2_PLACEMENT_3D ( 'NONE', #40759, #48928, #20277 ) ;
#13696 = DIRECTION ( 'NONE',  ( -0.000000000000000000, 1.000000000000000000, -0.000000000000000000 ) ) ;
#13697 = VECTOR ( 'NONE', #27014, 1000.000000000000000 ) ;
#13698 = CARTESIAN_POINT ( 'NONE',  ( -332.3517673607765914, -165.9166037625627439, 41.09453333279358134 ) ) ;
#13699 = PLANE ( 'NONE',  #33825 ) ;
#13700 = ORIENTED_EDGE ( 'NONE', *, *, #27233, .F. ) ;
#13701 = AXIS2_PLACEMENT_3D ( 'NONE', #45516, #50500, #14495 ) ;
#13702 = DIRECTION ( 'NONE',  ( 0.9027978299657446470, 0.000000000000000000, -0.4300652022765183435 ) ) ;
#13703 = FACE_OUTER_BOUND ( 'NONE', #4577, .T. ) ;
#13704 = DIRECTION ( 'NONE',  ( 0.000000000000000000, -0.000000000000000000, -1.000000000000000000 ) ) ;
#13705 = CARTESIAN_POINT ( 'NONE',  ( -330.4913330509368166, -180.9052250602809693, -13.63415328425256945 ) ) ;
#13706 = CIRCLE ( 'NONE', #23790, 60.00000000000000000 ) ;
#13707 = DIRECTION ( 'NONE',  ( 0.000000000000000000, 0.000000000000000000, 1.000000000000000000 ) ) ;
#13708 = DIRECTION ( 'NONE',  ( -0.000000000000000000, 1.000000000000000000, -0.000000000000000000 ) ) ;
#13709 = DIRECTION ( 'NONE',  ( -0.8757349421956310831, 0.000000000000000000, -0.4827922027307550712 ) ) ;
#13711 = ORIENTED_EDGE ( 'NONE', *, *, #12114, .T. ) ;
#13710 = FACE_OUTER_BOUND ( 'NONE', #25567, .T. ) ;
#13712 = VECTOR ( 'NONE', #42585, 1000.000000000000000 ) ;
#13713 = ORIENTED_EDGE ( 'NONE', *, *, #3514, .F. ) ;
#13714 = CARTESIAN_POINT ( 'NONE',  ( -172.1341525481709880, -193.5000000000000000, 18.28755301364337527 ) ) ;
#13715 = VECTOR ( 'NONE', #13716, 1000.000000000000227 ) ;
#13716 = DIRECTION ( 'NONE',  ( -0.000000000000000000, -0.1205366802553268363, -0.9927088740980534176 ) ) ;
#13718 = ORIENTED_EDGE ( 'NONE', *, *, #23233, .F. ) ;
#13717 = CARTESIAN_POINT ( 'NONE',  ( -66.64622755927948106, -193.5000000000000000, 123.6727797384707515 ) ) ;
#13719 = ORIENTED_EDGE ( 'NONE', *, *, #20608, .F. ) ;
#13720 = ORIENTED_EDGE ( 'NONE', *, *, #48437, .F. ) ;
#13721 = CYLINDRICAL_SURFACE ( 'NONE', #33453, 5.000000000000001776 ) ;
#13722 = EDGE_CURVE ( 'NONE', #33271, #49077, #39943, .T. ) ;
#13723 = EDGE_CURVE ( 'NONE', #36786, #38315, #15281, .T. ) ;
#13724 = EDGE_CURVE ( 'NONE', #22066, #47404, #31040, .T. ) ;
#13725 = CARTESIAN_POINT ( 'NONE',  ( -339.1964088526558498, -123.5000000000000284, 0.000000000000000000 ) ) ;
#13726 = CARTESIAN_POINT ( 'NONE',  ( -159.0901268547125653, -183.6283474603465606, 58.22548115875957109 ) ) ;
#13728 = ORIENTED_EDGE ( 'NONE', *, *, #36196, .T. ) ;
#13727 = CIRCLE ( 'NONE', #38890, 125.0000000000000000 ) ;
#13729 = ADVANCED_FACE ( 'NONE', ( #34991 ), #39682, .T. ) ;
#13730 = CARTESIAN_POINT ( 'NONE',  ( -48.36085358058748085, -193.5000000000000000, -0.9929810960135100339 ) ) ;
#13732 = EDGE_LOOP ( 'NONE', ( #15123, #32280, #19041, #373 ) ) ;
#13731 = PLANE ( 'NONE',  #25797 ) ;
#13733 = AXIS2_PLACEMENT_3D ( 'NONE', #412, #48540, #4368 ) ;
#13734 = EDGE_CURVE ( 'NONE', #25410, #48442, #22724, .T. ) ;
#13735 = ADVANCED_FACE ( 'NONE', ( #11837 ), #47864, .F. ) ;
#13736 = CARTESIAN_POINT ( 'NONE',  ( -69.77312546433408613, -175.3837268820161057, 123.1729094355499967 ) ) ;
#13737 = VERTEX_POINT ( 'NONE', #31297 ) ;
#13738 = PLANE ( 'NONE',  #32228 ) ;
#13739 = ORIENTED_EDGE ( 'NONE', *, *, #5725, .T. ) ;
#13740 = CARTESIAN_POINT ( 'NONE',  ( -48.47912675150885065, -183.6283474603465606, 6.938893903907228378E-15 ) ) ;
#13741 = EDGE_CURVE ( 'NONE', #43244, #5084, #7646, .T. ) ;
#13742 = CYLINDRICAL_SURFACE ( 'NONE', #12894, 125.0000000000000000 ) ;
#13743 = CARTESIAN_POINT ( 'NONE',  ( -13.05859477122062273, -175.3837268820161057, -118.8334608768479796 ) ) ;
#13744 = ADVANCED_FACE ( 'NONE', ( #36024 ), #27353, .F. ) ;
#13745 = EDGE_LOOP ( 'NONE', ( #20924, #49304 ) ) ;
#13746 = EDGE_CURVE ( 'NONE', #27241, #16769, #11063, .T. ) ;
#13747 = ORIENTED_EDGE ( 'NONE', *, *, #19651, .F. ) ;
#13748 = DIRECTION ( 'NONE',  ( 1.000000000000000000, -0.000000000000000000, -0.000000000000000000 ) ) ;
#13749 = ADVANCED_FACE ( 'NONE', ( #23432 ), #3437, .F. ) ;
#13750 = DIRECTION ( 'NONE',  ( 0.000000000000000000, 0.000000000000000000, 1.000000000000000000 ) ) ;
#13751 = VERTEX_POINT ( 'NONE', #35492 ) ;
#13752 = DIRECTION ( 'NONE',  ( -0.000000000000000000, 1.000000000000000000, -0.000000000000000000 ) ) ;
#13753 = AXIS2_PLACEMENT_3D ( 'NONE', #8071, #173, #20409 ) ;
#13754 = ADVANCED_FACE ( 'NONE', ( #51541 ), #15539, .T. ) ;
#13755 = ORIENTED_EDGE ( 'NONE', *, *, #13916, .F. ) ;
#13756 = PLANE ( 'NONE',  #32603 ) ;
#13758 = CIRCLE ( 'NONE', #40591, 125.0000000000000000 ) ;
#13757 = DIRECTION ( 'NONE',  ( 0.000000000000000000, 0.000000000000000000, 1.000000000000000000 ) ) ;
#13759 = ORIENTED_EDGE ( 'NONE', *, *, #35320, .T. ) ;
#13760 = LINE ( 'NONE', #34247, #22433 ) ;
#13761 = VERTEX_POINT ( 'NONE', #8169 ) ;
#13762 = FACE_OUTER_BOUND ( 'NONE', #42865, .T. ) ;
#13763 = CARTESIAN_POINT ( 'NONE',  ( -105.7090724259148118, -175.3837268820161057, 111.1293539894142839 ) ) ;
#13764 = CARTESIAN_POINT ( 'NONE',  ( -180.0000000000000568, -130.6726371812771959, -60.00000000000000711 ) ) ;
#13765 = ORIENTED_EDGE ( 'NONE', *, *, #42268, .F. ) ;
#13766 = DIRECTION ( 'NONE',  ( 0.000000000000000000, -1.000000000000000000, 0.000000000000000000 ) ) ;
#13767 = CARTESIAN_POINT ( 'NONE',  ( 60.00000000000001421, 0.000000000000000000, 0.000000000000000000 ) ) ;
#13768 = CARTESIAN_POINT ( 'NONE',  ( 58.48829670243886625, -193.5000000000000000, -64.67588669375805921 ) ) ;
#13769 = VECTOR ( 'NONE', #9925, 1000.000000000000000 ) ;
#13770 = CARTESIAN_POINT ( 'NONE',  ( 76.21810084846656252, -183.6283474603465606, -8.694908215727984668 ) ) ;
#13771 = EDGE_CURVE ( 'NONE', #26852, #39115, #16310, .T. ) ;
#13772 = VERTEX_POINT ( 'NONE', #40728 ) ;
#13773 = PLANE ( 'NONE',  #3597 ) ;
#13774 = ORIENTED_EDGE ( 'NONE', *, *, #28314, .T. ) ;
#13775 = PLANE ( 'NONE',  #49634 ) ;
#13777 = EDGE_LOOP ( 'NONE', ( #34667, #8601, #8450, #3873 ) ) ;
#13776 = CARTESIAN_POINT ( 'NONE',  ( -339.1964088526558498, -64.50000000000000000, -0.5000000000000457412 ) ) ;
#13778 = ORIENTED_EDGE ( 'NONE', *, *, #18279, .T. ) ;
#13779 = ADVANCED_FACE ( 'NONE', ( #1314 ), #5278, .F. ) ;
#13780 = CYLINDRICAL_SURFACE ( 'NONE', #235, 20.00000000000000000 ) ;
#13781 = ORIENTED_EDGE ( 'NONE', *, *, #15348, .F. ) ;
#13782 = DIRECTION ( 'NONE',  ( 0.000000000000000000, 1.000000000000000000, 0.000000000000000000 ) ) ;
#13783 = ORIENTED_EDGE ( 'NONE', *, *, #31167, .F. ) ;
#13784 = DIRECTION ( 'NONE',  ( 0.000000000000000000, 0.000000000000000000, -1.000000000000000000 ) ) ;
#13785 = CARTESIAN_POINT ( 'NONE',  ( -336.3521761649654422, -158.3591674452439122, -47.62880233550485087 ) ) ;
#13786 = AXIS2_PLACEMENT_3D ( 'NONE', #27942, #41580, #50008 ) ;
#13787 = CIRCLE ( 'NONE', #29720, 60.00000000000000000 ) ;
#13788 = EDGE_CURVE ( 'NONE', #41973, #27368, #12880, .T. ) ;
#13789 = ADVANCED_FACE ( 'NONE', ( #36527 ), #40468, .T. ) ;
#13790 = EDGE_CURVE ( 'NONE', #23116, #14590, #32598, .T. ) ;
#13791 = DIRECTION ( 'NONE',  ( 1.000000000000000000, -0.000000000000000000, -0.000000000000000000 ) ) ;
#13792 = DIRECTION ( 'NONE',  ( -0.000000000000000000, -0.2393156642875482742, 0.9709418174260544543 ) ) ;
#13793 = EDGE_LOOP ( 'NONE', ( #1963, #40748, #14602, #29411 ) ) ;
#13794 = EDGE_LOOP ( 'NONE', ( #51810, #4944, #5868, #45662 ) ) ;
#13795 = AXIS2_PLACEMENT_3D ( 'NONE', #19327, #22745, #39289 ) ;
#13796 = ADVANCED_FACE ( 'NONE', ( #28116 ), #44166, .F. ) ;
#13797 = ORIENTED_EDGE ( 'NONE', *, *, #32558, .T. ) ;
#13798 = LINE ( 'NONE', #10626, #12350 ) ;
#13799 = CARTESIAN_POINT ( 'NONE',  ( -157.8637630444124795, -193.5000000000000000, -60.49794494914009135 ) ) ;
#13800 = EDGE_CURVE ( 'NONE', #17216, #13387, #25238, .T. ) ;
#13801 = CARTESIAN_POINT ( 'NONE',  ( -112.1919339979530150, -189.7472609257535510, 107.5438431188761825 ) ) ;
#13802 = DIRECTION ( 'NONE',  ( 0.7378332790417189146, 0.000000000000000000, 0.6749830015182196608 ) ) ;
#13803 = ORIENTED_EDGE ( 'NONE', *, *, #5757, .T. ) ;
#13804 = PRODUCT_DEFINITION_CONTEXT ( 'detailed design', #30352, 'design' ) ;
#13805 = ADVANCED_FACE ( 'NONE', ( #8684 ), #36272, .F. ) ;
#13806 = VECTOR ( 'NONE', #28769, 1000.000000000000000 ) ;
#13807 = ORIENTED_EDGE ( 'NONE', *, *, #21333, .T. ) ;
#13809 = ORIENTED_EDGE ( 'NONE', *, *, #42407, .F. ) ;
#13808 = FACE_OUTER_BOUND ( 'NONE', #5065, .T. ) ;
#13810 = VERTEX_POINT ( 'NONE', #41251 ) ;
#13811 = EDGE_CURVE ( 'NONE', #44417, #39056, #44960, .T. ) ;
#13812 = FACE_OUTER_BOUND ( 'NONE', #2327, .T. ) ;
#13813 = PLANE ( 'NONE',  #39226 ) ;
#13814 = EDGE_CURVE ( 'NONE', #45414, #34872, #21295, .T. ) ;
#13815 = CARTESIAN_POINT ( 'NONE',  ( -93.85419746441394295, -193.5000000000000000, 115.4006183233324805 ) ) ;
#13816 = DIRECTION ( 'NONE',  ( -0.000000000000000000, 1.000000000000000000, 1.346129392433909288E-16 ) ) ;
#13817 = EDGE_LOOP ( 'NONE', ( #46826, #9716, #21865, #13210 ) ) ;
#13818 = DIRECTION ( 'NONE',  ( -1.000000000000000000, -0.000000000000000000, 0.000000000000000000 ) ) ;
#13819 = VERTEX_POINT ( 'NONE', #36806 ) ;
#13820 = EDGE_CURVE ( 'NONE', #4093, #11150, #32849, .T. ) ;
#13821 = ORIENTED_EDGE ( 'NONE', *, *, #38469, .T. ) ;
#13822 = DIRECTION ( 'NONE',  ( 0.000000000000000000, 0.000000000000000000, 1.000000000000000000 ) ) ;
#13823 = SURFACE_SIDE_STYLE ('',( #29058 ) ) ;
#13824 = FACE_OUTER_BOUND ( 'NONE', #27949, .T. ) ;
#13825 = ORIENTED_EDGE ( 'NONE', *, *, #6628, .T. ) ;
#13826 = AXIS2_PLACEMENT_3D ( 'NONE', #36536, #534, #27361 ) ;
#13827 = VECTOR ( 'NONE', #31794, 999.9999999999998863 ) ;
#13828 = CARTESIAN_POINT ( 'NONE',  ( -238.7407812814481076, -213.5000000000000000, -9.999999999999987566 ) ) ;
#13829 = CARTESIAN_POINT ( 'NONE',  ( -0.3054481938615516423, -193.5000000000000000, 115.3442529744090450 ) ) ;
#13830 = DIRECTION ( 'NONE',  ( 0.000000000000000000, 0.000000000000000000, -1.000000000000000000 ) ) ;
#13831 = DIRECTION ( 'NONE',  ( 0.000000000000000000, -0.000000000000000000, 1.000000000000000000 ) ) ;
#13832 = AXIS2_PLACEMENT_3D ( 'NONE', #10916, #26933, #3023 ) ;
#13833 = EDGE_CURVE ( 'NONE', #12420, #45870, #20585, .T. ) ;
#13834 = PLANE ( 'NONE',  #46296 ) ;
#13835 = DIRECTION ( 'NONE',  ( -0.000000000000000000, -0.4647231720437695057, -0.8854560256532093554 ) ) ;
#13836 = ORIENTED_EDGE ( 'NONE', *, *, #35560, .F. ) ;
#13837 = AXIS2_PLACEMENT_3D ( 'NONE', #33890, #13931, #49437 ) ;
#13838 = CARTESIAN_POINT ( 'NONE',  ( -180.0000000000000568, -123.5000000000000284, -20.00000000000002132 ) ) ;
#13839 = VERTEX_POINT ( 'NONE', #12617 ) ;
#13840 = ORIENTED_EDGE ( 'NONE', *, *, #44337, .T. ) ;
#13841 = DIRECTION ( 'NONE',  ( -0.2348860457809911206, 0.000000000000000000, 0.9720229140804089729 ) ) ;
#13842 = VECTOR ( 'NONE', #33702, 1000.000000000000000 ) ;
#13843 = VERTEX_POINT ( 'NONE', #803 ) ;
#13844 = PRODUCT ( 'Tool Retaining Set Screws', 'Tool Retaining Set Screws', '', ( #24948 ) ) ;
#13845 = DIRECTION ( 'NONE',  ( 0.000000000000000000, -1.000000000000000000, 0.000000000000000000 ) ) ;
#13846 = DIRECTION ( 'NONE',  ( -0.1182731709213523247, 0.000000000000000000, -0.9929810960135185827 ) ) ;
#13848 = ORIENTED_EDGE ( 'NONE', *, *, #45895, .F. ) ;
#13847 = DIRECTION ( 'NONE',  ( -0.000000000000000000, 1.000000000000000000, -0.000000000000000000 ) ) ;
#13849 = EDGE_CURVE ( 'NONE', #36957, #44616, #273, .T. ) ;
#13850 = EDGE_CURVE ( 'NONE', #39091, #49365, #22276, .T. ) ;
#13851 = CARTESIAN_POINT ( 'NONE',  ( -305.0000000000000568, -164.4944191672036311, -43.81161486573634534 ) ) ;
#13852 = CARTESIAN_POINT ( 'NONE',  ( -336.3521761649654422, -111.9361751271348879, -57.91551518289410438 ) ) ;
#13853 = ORIENTED_EDGE ( 'NONE', *, *, #3538, .F. ) ;
#13854 = ORIENTED_EDGE ( 'NONE', *, *, #587, .T. ) ;
#13855 = ORIENTED_EDGE ( 'NONE', *, *, #28113, .F. ) ;
#13856 = LINE ( 'NONE', #21224, #2428 ) ;
#13857 = CARTESIAN_POINT ( 'NONE',  ( 49.10711742958949344, -189.7472609257535510, 78.11481899503480975 ) ) ;
#13858 = VECTOR ( 'NONE', #2046, 1000.000000000000000 ) ;
#13859 = FACE_OUTER_BOUND ( 'NONE', #38407, .T. ) ;
#13860 = VECTOR ( 'NONE', #1776, 1000.000000000000000 ) ;
#13861 = CARTESIAN_POINT ( 'NONE',  ( -340.0000000000000568, -168.5000000000000284, 0.000000000000000000 ) ) ;
#13862 = DIRECTION ( 'NONE',  ( -0.000000000000000000, 0.4647231720437789981, 0.8854560256532044704 ) ) ;
#13863 = ORIENTED_EDGE ( 'NONE', *, *, #24102, .T. ) ;
#13864 = CIRCLE ( 'NONE', #49960, 124.9999999999999858 ) ;
#13865 = VECTOR ( 'NONE', #5782, 999.9999999999998863 ) ;
#13866 = DIRECTION ( 'NONE',  ( 0.7765238627180482966, 0.000000000000000000, -0.6300878435817038881 ) ) ;
#13867 = ORIENTED_EDGE ( 'NONE', *, *, #4016, .F. ) ;
#13869 = ORIENTED_EDGE ( 'NONE', *, *, #40425, .F. ) ;
#13868 = DIRECTION ( 'NONE',  ( 0.02963332782254913048, 0.000000000000000000, 0.9995608365087946812 ) ) ;
#13870 = VERTEX_POINT ( 'NONE', #8422 ) ;
#13872 = EDGE_CURVE ( 'NONE', #31730, #45161, #24449, .T. ) ;
#13871 = AXIS2_PLACEMENT_3D ( 'NONE', #46263, #46011, #25241 ) ;
#13873 = ORIENTED_EDGE ( 'NONE', *, *, #7630, .F. ) ;
#13874 = CARTESIAN_POINT ( 'NONE',  ( -336.3521761649654422, -123.5000000000000284, 0.000000000000000000 ) ) ;
#13875 = LINE ( 'NONE', #7216, #9655 ) ;
#13876 = VECTOR ( 'NONE', #21147, 1000.000000000000000 ) ;
#13877 = EDGE_LOOP ( 'NONE', ( #9569, #45667, #24764, #6638 ) ) ;
#13878 = DIRECTION ( 'NONE',  ( 0.000000000000000000, 0.000000000000000000, 1.000000000000000000 ) ) ;
#13879 = DIRECTION ( 'NONE',  ( 0.000000000000000000, -1.000000000000000000, 0.000000000000000000 ) ) ;
#13880 = ORIENTED_EDGE ( 'NONE', *, *, #11541, .F. ) ;
#13881 = CARTESIAN_POINT ( 'NONE',  ( -332.3517673607765914, -123.5000000000000284, 0.000000000000000000 ) ) ;
#13882 = AXIS2_PLACEMENT_3D ( 'NONE', #1596, #26262, #2089 ) ;
#13883 = EDGE_LOOP ( 'NONE', ( #41043, #32424, #38076, #20000 ) ) ;
#13884 = EDGE_CURVE ( 'NONE', #1575, #11111, #1267, .T. ) ;
#13885 = VECTOR ( 'NONE', #46008, 1000.000000000000000 ) ;
#13886 = VERTEX_POINT ( 'NONE', #40997 ) ;
#13887 = DIRECTION ( 'NONE',  ( -0.9473263538541946138, 0.000000000000000000, 0.3202698538628279690 ) ) ;
#13888 = LINE ( 'NONE', #42508, #1236 ) ;
#13889 = DIRECTION ( 'NONE',  ( -0.000000000000000000, 1.000000000000000000, -0.000000000000000000 ) ) ;
#13890 = FACE_OUTER_BOUND ( 'NONE', #39215, .T. ) ;
#13891 = ORIENTED_EDGE ( 'NONE', *, *, #50713, .T. ) ;
#13892 = FACE_OUTER_BOUND ( 'NONE', #36566, .T. ) ;
#13893 = CARTESIAN_POINT ( 'NONE',  ( -48.02249751411513756, -193.5000000000000000, -0.8896570909947397743 ) ) ;
#13894 = CARTESIAN_POINT ( 'NONE',  ( -49.38192458147459263, -177.1207230881787780, -0.4300652022765235616 ) ) ;
#13895 = CARTESIAN_POINT ( 'NONE',  ( -330.4913330509368166, -109.6270296344164308, -58.37414404713478433 ) ) ;
#13896 = VERTEX_POINT ( 'NONE', #34153 ) ;
#13897 = CYLINDRICAL_SURFACE ( 'NONE', #7845, 125.0000000000000000 ) ;
#13898 = CARTESIAN_POINT ( 'NONE',  ( -332.3517673607765914, -66.84438072661991725, -16.67542351306652648 ) ) ;
#13899 = DIRECTION ( 'NONE',  ( -1.000000000000000000, 0.000000000000000000, 0.000000000000000000 ) ) ;
#13900 = VERTEX_POINT ( 'NONE', #6047 ) ;
#13901 = AXIS2_PLACEMENT_3D ( 'NONE', #11347, #26352, #22423 ) ;
#13902 = DIRECTION ( 'NONE',  ( 0.000000000000000000, -1.000000000000000000, 0.000000000000000000 ) ) ;
#13903 = VECTOR ( 'NONE', #43144, 1000.000000000000000 ) ;
#13904 = VECTOR ( 'NONE', #13445, 1000.000000000000000 ) ;
#13905 = CARTESIAN_POINT ( 'NONE',  ( -180.0000000000000568, -123.5000000000000284, 41.63467731922665394 ) ) ;
#13906 = CARTESIAN_POINT ( 'NONE',  ( -105.4063847101409692, -175.3837268820161057, -111.2847127925096231 ) ) ;
#13907 = EDGE_LOOP ( 'NONE', ( #35196, #46135, #46115, #41747 ) ) ;
#13908 = DIRECTION ( 'NONE',  ( -0.000000000000000000, 1.000000000000000000, -0.000000000000000000 ) ) ;
#13909 = VERTEX_POINT ( 'NONE', #41510 ) ;
#13910 = CARTESIAN_POINT ( 'NONE',  ( -48.47912675150885065, -183.6283474603465606, 6.938893903907228378E-15 ) ) ;
#13911 = DIRECTION ( 'NONE',  ( 0.000000000000000000, -1.000000000000000000, -1.156482317317871232E-16 ) ) ;
#13912 = CIRCLE ( 'NONE', #43270, 125.0000000000000000 ) ;
#13913 = CARTESIAN_POINT ( 'NONE',  ( 60.00000000000001421, 20.00000000000000000, -60.00000000000000711 ) ) ;
#13914 = AXIS2_PLACEMENT_3D ( 'NONE', #9370, #45380, #25396 ) ;
#13915 = CARTESIAN_POINT ( 'NONE',  ( 75.04604393171727850, -193.5000000000000000, -10.84123789944574234 ) ) ;
#13916 = EDGE_CURVE ( 'NONE', #23163, #7887, #42550, .T. ) ;
#13917 = VECTOR ( 'NONE', #24220, 1000.000000000000000 ) ;
#13918 = DIRECTION ( 'NONE',  ( 1.000000000000000000, -0.000000000000000000, -0.000000000000000000 ) ) ;
#13919 = ORIENTED_EDGE ( 'NONE', *, *, #48451, .F. ) ;
#13920 = DIRECTION ( 'NONE',  ( 0.000000000000000000, -0.000000000000000000, 1.000000000000000000 ) ) ;
#13921 = ORIENTED_EDGE ( 'NONE', *, *, #16048, .T. ) ;
#13922 = CIRCLE ( 'NONE', #28150, 60.00000000000000000 ) ;
#13923 = PLANE ( 'NONE',  #9111 ) ;
#13924 = ORIENTED_EDGE ( 'NONE', *, *, #25578, .T. ) ;
#13925 = CARTESIAN_POINT ( 'NONE',  ( -64.08700758308647494, -193.5000000000000000, -124.0217483183786840 ) ) ;
#13926 = ORIENTED_EDGE ( 'NONE', *, *, #35612, .T. ) ;
#13927 = LINE ( 'NONE', #29950, #46883 ) ;
#13928 = FACE_OUTER_BOUND ( 'NONE', #35056, .T. ) ;
#13929 = ORIENTED_EDGE ( 'NONE', *, *, #40966, .T. ) ;
#13932 = ORIENTED_EDGE ( 'NONE', *, *, #3241, .F. ) ;
#13931 = DIRECTION ( 'NONE',  ( -0.9842305779475992722, 0.000000000000000000, 0.1768902751225592818 ) ) ;
#13930 = DIRECTION ( 'NONE',  ( 0.000000000000000000, 1.000000000000000000, 0.000000000000000000 ) ) ;
#13933 = VECTOR ( 'NONE', #11284, 1000.000000000000227 ) ;
#13934 = EDGE_CURVE ( 'NONE', #11778, #28008, #9995, .T. ) ;
#13935 = DIRECTION ( 'NONE',  ( 0.5338233779647948429, 0.000000000000000000, -0.8455960035018234011 ) ) ;
#13936 = AXIS2_PLACEMENT_3D ( 'NONE', #33653, #550, #13688 ) ;
#13937 = VERTEX_POINT ( 'NONE', #29425 ) ;
#13938 = FACE_OUTER_BOUND ( 'NONE', #26179, .T. ) ;
#13939 = ORIENTED_EDGE ( 'NONE', *, *, #13302, .T. ) ;
#13940 = CIRCLE ( 'NONE', #9736, 125.0000000000000000 ) ;
#13941 = DIRECTION ( 'NONE',  ( 1.000000000000000000, -4.051632851310755856E-17, -7.719741424018455803E-17 ) ) ;
#13944 = EDGE_LOOP ( 'NONE', ( #30602, #14018, #28509, #37379 ) ) ;
#13943 = CARTESIAN_POINT ( 'NONE',  ( -330.4913330509368166, -175.5095439275173419, 27.86139516340933042 ) ) ;
#13942 = CARTESIAN_POINT ( 'NONE',  ( -336.3521761649654422, -123.5000000000000284, 0.000000000000000000 ) ) ;
#13945 = ORIENTED_EDGE ( 'NONE', *, *, #11825, .T. ) ;
#13946 = DIRECTION ( 'NONE',  ( -0.000000000000000000, 1.000000000000000000, -0.000000000000000000 ) ) ;
#13947 = VERTEX_POINT ( 'NONE', #18645 ) ;
#13948 = FACE_OUTER_BOUND ( 'NONE', #11923, .T. ) ;
#13949 = CARTESIAN_POINT ( 'NONE',  ( 0.000000000000000000, -102.5783116644897888, 55.16595831843925879 ) ) ;
#13950 = ORIENTED_EDGE ( 'NONE', *, *, #5431, .F. ) ;
#13951 = AXIS2_PLACEMENT_3D ( 'NONE', #8965, #815, #44449 ) ;
#13952 = DIRECTION ( 'NONE',  ( 1.043714542225393381E-14, -0.000000000000000000, 1.000000000000000000 ) ) ;
#13953 = SURFACE_STYLE_USAGE ( .BOTH. , #1073 ) ;
#13954 = DIRECTION ( 'NONE',  ( -0.000000000000000000, 1.000000000000000000, -0.000000000000000000 ) ) ;
#13955 = DIRECTION ( 'NONE',  ( -0.7765238627180349740, 0.000000000000000000, -0.6300878435817203194 ) ) ;
#13956 = ORIENTED_EDGE ( 'NONE', *, *, #17602, .T. ) ;
#13957 = VECTOR ( 'NONE', #39389, 1000.000000000000000 ) ;
#13958 = DIRECTION ( 'NONE',  ( -0.000000000000000000, 1.000000000000000000, -0.000000000000000000 ) ) ;
#13959 = CARTESIAN_POINT ( 'NONE',  ( -330.4913330509368166, -167.3305728129743102, 39.49849221029282376 ) ) ;
#13960 = AXIS2_PLACEMENT_3D ( 'NONE', #43225, #34811, #35089 ) ;
#13961 = DIRECTION ( 'NONE',  ( -0.4677363560876381943, 0.000000000000000000, -0.8838680338115290080 ) ) ;
#13962 = VERTEX_POINT ( 'NONE', #6301 ) ;
#13963 = LINE ( 'NONE', #9251, #13904 ) ;
#13964 = CARTESIAN_POINT ( 'NONE',  ( -339.1964088526558498, -178.4886558749180949, 21.38919645685277970 ) ) ;
#13965 = CARTESIAN_POINT ( 'NONE',  ( -48.47912675150885065, -183.6283474603465606, 6.938893903907228378E-15 ) ) ;
#13966 = EDGE_CURVE ( 'NONE', #16290, #12249, #14702, .T. ) ;
#13967 = LINE ( 'NONE', #5315, #36700 ) ;
#13968 = CARTESIAN_POINT ( 'NONE',  ( 73.03012110230136500, -193.5000000000000000, 24.72869175143111420 ) ) ;
#13969 = ADVANCED_FACE ( 'NONE', ( #13928 ), #6571, .T. ) ;
#13970 = VECTOR ( 'NONE', #31732, 1000.000000000000000 ) ;
#13971 = AXIS2_PLACEMENT_3D ( 'NONE', #7118, #43109, #23154 ) ;
#13972 = DIRECTION ( 'NONE',  ( 0.9890401873221644768, 0.000000000000000000, -0.1476465640024779702 ) ) ;
#13973 = DIRECTION ( 'NONE',  ( -0.000000000000000000, 1.000000000000000000, -0.000000000000000000 ) ) ;
#13975 = ORIENTED_EDGE ( 'NONE', *, *, #17246, .F. ) ;
#13974 = DIRECTION ( 'NONE',  ( 0.000000000000000000, 0.000000000000000000, 1.000000000000000000 ) ) ;
#13976 = VECTOR ( 'NONE', #43092, 1000.000000000000000 ) ;
#13977 = ORIENTED_EDGE ( 'NONE', *, *, #12754, .F. ) ;
#13978 = EDGE_CURVE ( 'NONE', #39444, #39193, #34826, .T. ) ;
#13979 = EDGE_CURVE ( 'NONE', #19422, #34734, #29951, .T. ) ;
#13980 = PLANE ( 'NONE',  #16234 ) ;
#13982 = ORIENTED_EDGE ( 'NONE', *, *, #49749, .T. ) ;
#13981 = LINE ( 'NONE', #30009, #11914 ) ;
#13983 = VECTOR ( 'NONE', #17959, 1000.000000000000000 ) ;
#13984 = ORIENTED_EDGE ( 'NONE', *, *, #5737, .F. ) ;
#13985 = EDGE_CURVE ( 'NONE', #39919, #31214, #10237, .T. ) ;
#13986 = CIRCLE ( 'NONE', #28221, 16.00000000000000000 ) ;
#13987 = EDGE_LOOP ( 'NONE', ( #20426, #22401, #46762, #41062 ) ) ;
#13988 = DIRECTION ( 'NONE',  ( 0.000000000000000000, 0.000000000000000000, 1.000000000000000000 ) ) ;
#13989 = VECTOR ( 'NONE', #2057, 1000.000000000000000 ) ;
#13990 = AXIS2_PLACEMENT_3D ( 'NONE', #9047, #20332, #44520 ) ;
#13992 = AXIS2_PLACEMENT_3D ( 'NONE', #49019, #36668, #40587 ) ;
#13991 = CARTESIAN_POINT ( 'NONE',  ( -154.6193097927903182, -189.7472609257535510, -66.02470404298122730 ) ) ;
#13993 = CARTESIAN_POINT ( 'NONE',  ( -170.5806857741408180, -177.1207230881787780, -21.61797988633146872 ) ) ;
#13994 = ORIENTED_EDGE ( 'NONE', *, *, #12434, .F. ) ;
#13995 = AXIS2_PLACEMENT_3D ( 'NONE', #40224, #15826, #44448 ) ;
#13996 = DIRECTION ( 'NONE',  ( 0.000000000000000000, -1.000000000000000000, 0.000000000000000000 ) ) ;
#13997 = DIRECTION ( 'NONE',  ( -0.000000000000000000, 1.000000000000000000, -0.000000000000000000 ) ) ;
#13999 = EDGE_LOOP ( 'NONE', ( #8584, #23369, #40528, #20372 ) ) ;
#13998 = DIRECTION ( 'NONE',  ( 0.000000000000000000, -0.000000000000000000, 1.000000000000000000 ) ) ;
#14000 = EDGE_CURVE ( 'NONE', #32000, #4695, #34951, .T. ) ;
#14001 = CARTESIAN_POINT ( 'NONE',  ( -336.3521761649654422, -101.0520950768976149, 54.58714071513087873 ) ) ;
#14002 = ORIENTED_EDGE ( 'NONE', *, *, #26895, .T. ) ;
#14003 = CYLINDRICAL_SURFACE ( 'NONE', #33098, 15.24495751795539000 ) ;
#14004 = ORIENTED_EDGE ( 'NONE', *, *, #39321, .F. ) ;
#14005 = VECTOR ( 'NONE', #3818, 1000.000000000000114 ) ;
#14006 = CARTESIAN_POINT ( 'NONE',  ( -336.3521761649654422, -93.75055682584159911, 51.01861988938794923 ) ) ;
#14007 = DIRECTION ( 'NONE',  ( 1.000000000000000000, -0.000000000000000000, -0.000000000000000000 ) ) ;
#14008 = PLANE ( 'NONE',  #39153 ) ;
#14009 = ORIENTED_EDGE ( 'NONE', *, *, #48592, .T. ) ;
#14010 = CIRCLE ( 'NONE', #14847, 60.00000000000000000 ) ;
#14011 = ORIENTED_EDGE ( 'NONE', *, *, #32944, .F. ) ;
#14012 = DIRECTION ( 'NONE',  ( 0.000000000000000000, 1.346129392433909288E-16, -1.000000000000000000 ) ) ;
#14013 = AXIS2_PLACEMENT_3D ( 'NONE', #31334, #38700, #38452 ) ;
#14014 = DIRECTION ( 'NONE',  ( -0.6068001458186002006, 0.000000000000000000, 0.7948544414133481562 ) ) ;
#14015 = ORIENTED_EDGE ( 'NONE', *, *, #14509, .F. ) ;
#14016 = DIRECTION ( 'NONE',  ( -0.000000000000000000, -1.000000000000000000, -0.000000000000000000 ) ) ;
#14017 = AXIS2_PLACEMENT_3D ( 'NONE', #4022, #4536, #51337 ) ;
#14018 = ORIENTED_EDGE ( 'NONE', *, *, #24005, .F. ) ;
#14019 = CARTESIAN_POINT ( 'NONE',  ( -99.62791064391784346, -193.5000000000000000, -114.0561348912352173 ) ) ;
#14020 = DIRECTION ( 'NONE',  ( -0.000000000000000000, 1.000000000000000000, -0.000000000000000000 ) ) ;
#14021 = ORIENTED_EDGE ( 'NONE', *, *, #46435, .T. ) ;
#14022 = CARTESIAN_POINT ( 'NONE',  ( 68.79964045138289919, -177.1207230881787780, 43.25148278810711133 ) ) ;
#14023 = ORIENTED_EDGE ( 'NONE', *, *, #27253, .F. ) ;
#14024 = VECTOR ( 'NONE', #39703, 1000.000000000000000 ) ;
#14025 = DIRECTION ( 'NONE',  ( 0.000000000000000000, 0.000000000000000000, -1.000000000000000000 ) ) ;
#14026 = CARTESIAN_POINT ( 'NONE',  ( -32.98951909085346301, -193.5000000000000000, 123.0287672223652891 ) ) ;
#14027 = CIRCLE ( 'NONE', #43392, 125.0000000000000000 ) ;
#14028 = LINE ( 'NONE', #42126, #45505 ) ;
#14029 = VERTEX_POINT ( 'NONE', #22594 ) ;
#14030 = AXIS2_PLACEMENT_3D ( 'NONE', #36283, #8178, #47874 ) ;
#14031 = VECTOR ( 'NONE', #41030, 1000.000000000000114 ) ;
#14032 = DIRECTION ( 'NONE',  ( -0.000000000000000000, 1.000000000000000000, -0.000000000000000000 ) ) ;
#14033 = ADVANCED_FACE ( 'NONE', ( #18394 ), #38083, .F. ) ;
#14034 = CARTESIAN_POINT ( 'NONE',  ( 37.29583330861160562, -189.7472609257535510, -89.54698061029594669 ) ) ;
#14035 = DIRECTION ( 'NONE',  ( 0.000000000000000000, 0.000000000000000000, 1.000000000000000000 ) ) ;
#14036 = ADVANCED_FACE ( 'NONE', ( #30461 ), #14198, .F. ) ;
#14037 = STYLED_ITEM ( 'NONE', ( #12901 ), #18528 ) ;
#14038 = DIRECTION ( 'NONE',  ( 0.7378332790417239107, 0.000000000000000000, 0.6749830015182142207 ) ) ;
#14039 = ORIENTED_EDGE ( 'NONE', *, *, #45031, .F. ) ;
#14041 = VECTOR ( 'NONE', #8118, 1000.000000000000000 ) ;
#14040 = DIRECTION ( 'NONE',  ( -0.000000000000000000, -0.000000000000000000, 1.000000000000000000 ) ) ;
#14042 = ORIENTED_EDGE ( 'NONE', *, *, #49179, .F. ) ;
#14043 = LINE ( 'NONE', #17203, #50384 ) ;
#14045 = ORIENTED_EDGE ( 'NONE', *, *, #45769, .F. ) ;
#14044 = DIRECTION ( 'NONE',  ( 0.7765238627180393038, 0.000000000000000000, 0.6300878435817147682 ) ) ;
#14046 = ORIENTED_EDGE ( 'NONE', *, *, #26880, .F. ) ;
#14047 = DIRECTION ( 'NONE',  ( 0.000000000000000000, 1.000000000000000000, -0.000000000000000000 ) ) ;
#14048 = EDGE_CURVE ( 'NONE', #9666, #8625, #2128, .T. ) ;
#14049 = ADVANCED_FACE ( 'NONE', ( #49674 ), #13667, .F. ) ;
#14050 = FACE_OUTER_BOUND ( 'NONE', #14288, .T. ) ;
#14051 = CIRCLE ( 'NONE', #9019, 4.999999999999997335 ) ;
#14052 = AXIS2_PLACEMENT_3D ( 'NONE', #9506, #41547, #2125 ) ;
#14053 = EDGE_LOOP ( 'NONE', ( #2528, #15558, #19753, #26899 ) ) ;
#14054 = EDGE_CURVE ( 'NONE', #51208, #44162, #26257, .T. ) ;
#14055 = CARTESIAN_POINT ( 'NONE',  ( -172.3334410065085933, -177.1207230881787780, -6.025661128238047226 ) ) ;
#14056 = ORIENTED_EDGE ( 'NONE', *, *, #259, .F. ) ;
#14057 = DIRECTION ( 'NONE',  ( 0.000000000000000000, 0.000000000000000000, -1.000000000000000000 ) ) ;
#14058 = CARTESIAN_POINT ( 'NONE',  ( -48.47912675150885065, -177.1207230881787780, 6.938893903907228378E-15 ) ) ;
#14059 = AXIS2_PLACEMENT_3D ( 'NONE', #6288, #3563, #51669 ) ;
#14060 = EDGE_CURVE ( 'NONE', #30477, #6939, #14452, .T. ) ;
#14061 = CARTESIAN_POINT ( 'NONE',  ( -339.1964088526558498, -122.9999999999993747, 59.00000000000002132 ) ) ;
#14062 = FACE_OUTER_BOUND ( 'NONE', #28, .T. ) ;
#14063 = ORIENTED_EDGE ( 'NONE', *, *, #4059, .T. ) ;
#14064 = ORIENTED_EDGE ( 'NONE', *, *, #42836, .T. ) ;
#14065 = ORIENTED_EDGE ( 'NONE', *, *, #31357, .F. ) ;
#14066 = DIRECTION ( 'NONE',  ( 0.000000000000000000, 1.000000000000000000, 0.000000000000000000 ) ) ;
#14067 = DIRECTION ( 'NONE',  ( -0.000000000000000000, 1.000000000000000000, -0.000000000000000000 ) ) ;
#14068 = CIRCLE ( 'NONE', #27471, 125.0000000000000000 ) ;
#14069 = AXIS2_PLACEMENT_3D ( 'NONE', #21092, #1111, #17159 ) ;
#14070 = AXIS2_PLACEMENT_3D ( 'NONE', #35380, #7020, #43015 ) ;
#14071 = LINE ( 'NONE', #1454, #29558 ) ;
#14072 = CARTESIAN_POINT ( 'NONE',  ( -162.9896759831413249, -177.1207230881787780, -50.12318939043961308 ) ) ;
#14073 = VERTEX_POINT ( 'NONE', #41790 ) ;
#14074 = VECTOR ( 'NONE', #48609, 999.9999999999998863 ) ;
#14075 = AXIS2_PLACEMENT_3D ( 'NONE', #28117, #19722, #35755 ) ;
#14076 = ORIENTED_EDGE ( 'NONE', *, *, #4263, .F. ) ;
#14078 = ORIENTED_EDGE ( 'NONE', *, *, #14000, .T. ) ;
#14077 = CARTESIAN_POINT ( 'NONE',  ( -336.3521761649654422, -73.44864141332200802, 31.34948880313848107 ) ) ;
#14079 = DIRECTION ( 'NONE',  ( -0.000000000000000000, 0.5680647467311656929, 0.8229838658936495799 ) ) ;
#14080 = CARTESIAN_POINT ( 'NONE',  ( -46.00000000000000711, 20.00000000000000000, -51.00000000000000000 ) ) ;
#14081 = LINE ( 'NONE', #2250, #14494 ) ;
#14082 = PLANE ( 'NONE',  #30148 ) ;
#14083 = EDGE_LOOP ( 'NONE', ( #27054, #19455, #3727, #7281 ) ) ;
#14084 = DIRECTION ( 'NONE',  ( 0.000000000000000000, -0.5680647467311457088, 0.8229838658936633466 ) ) ;
#14085 = ORIENTED_EDGE ( 'NONE', *, *, #22640, .F. ) ;
#14086 = EDGE_CURVE ( 'NONE', #44743, #26606, #38214, .T. ) ;
#14087 = ORIENTED_EDGE ( 'NONE', *, *, #10136, .T. ) ;
#14088 = DIRECTION ( 'NONE',  ( 0.9720229140804089729, 0.000000000000000000, 0.2348860457809911206 ) ) ;
#14089 = AXIS2_PLACEMENT_3D ( 'NONE', #12442, #43481, #8245 ) ;
#14090 = AXIS2_PLACEMENT_3D ( 'NONE', #17886, #33899, #6060 ) ;
#14091 = FACE_OUTER_BOUND ( 'NONE', #36190, .T. ) ;
#14092 = EDGE_LOOP ( 'NONE', ( #41357, #49937, #24539, #11069 ) ) ;
#14093 = CIRCLE ( 'NONE', #25865, 125.0000000000000000 ) ;
#14094 = EDGE_CURVE ( 'NONE', #34425, #34216, #2610, .T. ) ;
#14095 = CARTESIAN_POINT ( 'NONE',  ( -156.2577088867455473, -177.1207230881787780, -63.31490529818420754 ) ) ;
#14096 = EDGE_CURVE ( 'NONE', #51653, #26682, #32447, .T. ) ;
#14097 = PLANE ( 'NONE',  #2861 ) ;
#14098 = DIRECTION ( 'NONE',  ( 0.000000000000000000, -1.000000000000000000, 0.000000000000000000 ) ) ;
#14099 = ADVANCED_FACE ( 'NONE', ( #27800 ), #42808, .T. ) ;
#14100 = LINE ( 'NONE', #9626, #51790 ) ;
#14101 = EDGE_CURVE ( 'NONE', #22800, #29344, #39157, .T. ) ;
#14102 = LINE ( 'NONE', #10395, #9368 ) ;
#14103 = ORIENTED_EDGE ( 'NONE', *, *, #35216, .T. ) ;
#14104 = AXIS2_PLACEMENT_3D ( 'NONE', #387, #15668, #31682 ) ;
#14105 = EDGE_CURVE ( 'NONE', #17063, #1035, #14973, .T. ) ;
#14106 = CARTESIAN_POINT ( 'NONE',  ( -339.1964088526558498, -63.87926739338324467, 6.735595255825790773 ) ) ;
#14107 = ORIENTED_EDGE ( 'NONE', *, *, #10571, .F. ) ;
#14108 = EDGE_LOOP ( 'NONE', ( #29264, #38167, #50837, #36684 ) ) ;
#14109 = DIRECTION ( 'NONE',  ( 0.000000000000000000, 0.000000000000000000, -1.000000000000000000 ) ) ;
#14110 = EDGE_CURVE ( 'NONE', #17428, #1806, #7340, .T. ) ;
#14111 = ORIENTED_EDGE ( 'NONE', *, *, #28881, .F. ) ;
#14112 = EDGE_CURVE ( 'NONE', #13304, #47014, #19163, .T. ) ;
#14113 = VECTOR ( 'NONE', #48659, 1000.000000000000227 ) ;
#14114 = DIRECTION ( 'NONE',  ( -0.000000000000000000, 1.000000000000000000, -0.000000000000000000 ) ) ;
#14115 = EDGE_CURVE ( 'NONE', #28621, #37366, #35430, .T. ) ;
#14116 = DIRECTION ( 'NONE',  ( 0.6068001458185945385, 0.000000000000000000, -0.7948544414133523750 ) ) ;
#14118 = ORIENTED_EDGE ( 'NONE', *, *, #18313, .F. ) ;
#14117 = DIRECTION ( 'NONE',  ( 0.000000000000000000, 0.000000000000000000, -1.000000000000000000 ) ) ;
#14119 = FACE_OUTER_BOUND ( 'NONE', #8687, .T. ) ;
#14120 = ADVANCED_FACE ( 'NONE', ( #46766 ), #23368, .F. ) ;
#14121 = LINE ( 'NONE', #41704, #14307 ) ;
#14122 = LINE ( 'NONE', #26439, #50051 ) ;
#14123 = ORIENTED_EDGE ( 'NONE', *, *, #33253, .F. ) ;
#14124 = EDGE_LOOP ( 'NONE', ( #34654, #43783, #27098, #25702 ) ) ;
#14125 = EDGE_CURVE ( 'NONE', #32017, #44417, #51231, .T. ) ;
#14126 = ORIENTED_EDGE ( 'NONE', *, *, #41272, .T. ) ;
#14127 = CARTESIAN_POINT ( 'NONE',  ( 31.28129687248616619, -177.1207230881787780, 96.24590808611479531 ) ) ;
#14128 = AXIS2_PLACEMENT_3D ( 'NONE', #45561, #1667, #33968 ) ;
#14129 = DIRECTION ( 'NONE',  ( 0.9995608365087942371, 0.000000000000000000, 0.02963332782256331357 ) ) ;
#14130 = AXIS2_PLACEMENT_3D ( 'NONE', #30938, #43019, #23053 ) ;
#14131 = VECTOR ( 'NONE', #51288, 1000.000000000000000 ) ;
#14132 = CARTESIAN_POINT ( 'NONE',  ( -332.3517673607765914, -123.5000000000000284, 0.000000000000000000 ) ) ;
#14133 = DIRECTION ( 'NONE',  ( -0.2920567706369833760, 0.000000000000000000, 0.9564009842765202052 ) ) ;
#14134 = DIRECTION ( 'NONE',  ( -0.000000000000000000, 1.000000000000000000, -0.000000000000000000 ) ) ;
#14135 = ORIENTED_EDGE ( 'NONE', *, *, #21040, .F. ) ;
#14136 = AXIS2_PLACEMENT_3D ( 'NONE', #25545, #36860, #25290 ) ;
#14137 = ADVANCED_FACE ( 'NONE', ( #47287 ), #18895, .F. ) ;
#14138 = ADVANCED_FACE ( 'NONE', ( #31232 ), #51744, .F. ) ;
#14139 = CARTESIAN_POINT ( 'NONE',  ( -47.63353074800703268, -183.6283474603465606, 0.5338233779648018373 ) ) ;
#14140 = ORIENTED_EDGE ( 'NONE', *, *, #27084, .T. ) ;
#14142 = ORIENTED_EDGE ( 'NONE', *, *, #48504, .F. ) ;
#14141 = DIRECTION ( 'NONE',  ( 0.000000000000000000, 1.000000000000000000, 0.000000000000000000 ) ) ;
#14143 = VECTOR ( 'NONE', #27281, 1000.000000000000000 ) ;
#14144 = ORIENTED_EDGE ( 'NONE', *, *, #25133, .F. ) ;
#14145 = CARTESIAN_POINT ( 'NONE',  ( -169.2746641285359317, -189.7472609257535510, -32.14713283941908628 ) ) ;
#14146 = ORIENTED_EDGE ( 'NONE', *, *, #17032, .T. ) ;
#14147 = CARTESIAN_POINT ( 'NONE',  ( -32.87124591993210743, -189.7472609257535510, 124.0217483183788261 ) ) ;
#14148 = VERTEX_POINT ( 'NONE', #2864 ) ;
#14149 = FACE_OUTER_BOUND ( 'NONE', #31369, .T. ) ;
#14150 = CYLINDRICAL_SURFACE ( 'NONE', #8284, 4.999999999999997335 ) ;
#14151 = ORIENTED_EDGE ( 'NONE', *, *, #36153, .F. ) ;
#14152 = PLANE ( 'NONE',  #29194 ) ;
#14153 = VERTEX_POINT ( 'NONE', #3635 ) ;
#14154 = VECTOR ( 'NONE', #4437, 1000.000000000000000 ) ;
#14155 = ORIENTED_EDGE ( 'NONE', *, *, #16851, .T. ) ;
#14156 = CARTESIAN_POINT ( 'NONE',  ( -170.9669310976187830, -189.7472609257535510, -24.93467037017131105 ) ) ;
#14157 = CARTESIAN_POINT ( 'NONE',  ( 27.23560471289044571, -193.5000000000000000, 99.45993886622845537 ) ) ;
#14158 = CARTESIAN_POINT ( 'NONE',  ( -339.1964088526558498, -95.17484985463171654, -52.89315522109019696 ) ) ;
#14159 = LINE ( 'NONE', #1014, #17344 ) ;
#14160 = ORIENTED_EDGE ( 'NONE', *, *, #3512, .F. ) ;
#14161 = CARTESIAN_POINT ( 'NONE',  ( 74.31448861501726810, -193.5000000000000000, -23.38221600314288651 ) ) ;
#14162 = LINE ( 'NONE', #34874, #27274 ) ;
#14163 = EDGE_CURVE ( 'NONE', #28107, #2431, #39880, .T. ) ;
#14164 = EDGE_CURVE ( 'NONE', #7125, #17289, #7161, .T. ) ;
#14165 = LINE ( 'NONE', #17074, #29685 ) ;
#14166 = CARTESIAN_POINT ( 'NONE',  ( -330.4913330509368166, -74.40671499923438148, -34.49419324804681253 ) ) ;
#14167 = EDGE_LOOP ( 'NONE', ( #44213, #51520, #35331, #29645 ) ) ;
#14168 = LINE ( 'NONE', #30186, #7039 ) ;
#14169 = PLANE ( 'NONE',  #27345 ) ;
#14170 = EDGE_CURVE ( 'NONE', #21107, #15488, #11524, .T. ) ;
#14171 = EDGE_CURVE ( 'NONE', #26317, #26852, #5606, .T. ) ;
#14172 = DIRECTION ( 'NONE',  ( 0.000000000000000000, 1.000000000000000000, -0.000000000000000000 ) ) ;
#14173 = AXIS2_PLACEMENT_3D ( 'NONE', #51260, #31797, #15247 ) ;
#14174 = ORIENTED_EDGE ( 'NONE', *, *, #33184, .T. ) ;
#14175 = VECTOR ( 'NONE', #34801, 1000.000000000000114 ) ;
#14176 = AXIS2_PLACEMENT_3D ( 'NONE', #10236, #18894, #50204 ) ;
#14177 = DIRECTION ( 'NONE',  ( 0.000000000000000000, 0.000000000000000000, -1.000000000000000000 ) ) ;
#14178 = PRESENTATION_LAYER_ASSIGNMENT (  '', '', ( #36817 ) ) ;
#14179 = DIRECTION ( 'NONE',  ( 0.9027978299657387629, 0.000000000000000000, 0.4300652022765304450 ) ) ;
#14180 = ORIENTED_EDGE ( 'NONE', *, *, #21696, .T. ) ;
#14181 = CYLINDRICAL_SURFACE ( 'NONE', #31284, 125.0000000000000000 ) ;
#14182 = ORIENTED_EDGE ( 'NONE', *, *, #27234, .T. ) ;
#14183 = AXIS2_PLACEMENT_3D ( 'NONE', #28573, #48833, #44615 ) ;
#14184 = CARTESIAN_POINT ( 'NONE',  ( -330.0000000000000568, -123.5000000000000284, 0.000000000000000000 ) ) ;
#14185 = CARTESIAN_POINT ( 'NONE',  ( -171.9128728525929262, -189.7472609257535510, 11.83705339977325011 ) ) ;
#14186 = CARTESIAN_POINT ( 'NONE',  ( 35.67816836544800907, -177.1207230881787780, -92.42591454022745268 ) ) ;
#14187 = LINE ( 'NONE', #13915, #26651 ) ;
#14188 = CARTESIAN_POINT ( 'NONE',  ( -336.3521761649654422, -123.5000000000000284, 0.000000000000000000 ) ) ;
#14189 = ORIENTED_EDGE ( 'NONE', *, *, #22742, .F. ) ;
#14190 = EDGE_CURVE ( 'NONE', #37305, #2972, #30979, .T. ) ;
#14191 = AXIS2_PLACEMENT_3D ( 'NONE', #8319, #11982, #15956 ) ;
#14192 = DIRECTION ( 'NONE',  ( -0.000000000000000000, 0.6631226582408039638, 0.7485107481710934207 ) ) ;
#14193 = VERTEX_POINT ( 'NONE', #27028 ) ;
#14194 = LINE ( 'NONE', #42025, #29208 ) ;
#14195 = ORIENTED_EDGE ( 'NONE', *, *, #15475, .F. ) ;
#14196 = LINE ( 'NONE', #6297, #5819 ) ;
#14197 = DIRECTION ( 'NONE',  ( -0.000000000000000000, 0.000000000000000000, 1.000000000000000000 ) ) ;
#14198 = PLANE ( 'NONE',  #9679 ) ;
#14199 = ORIENTED_EDGE ( 'NONE', *, *, #195, .F. ) ;
#14202 = ORIENTED_EDGE ( 'NONE', *, *, #22622, .F. ) ;
#14201 = CARTESIAN_POINT ( 'NONE',  ( -7.223120065443619175, -177.1207230881787780, 117.9955164924470523 ) ) ;
#14200 = CARTESIAN_POINT ( 'NONE',  ( -170.8336150310144887, -175.3837268820161057, 25.58083653558494319 ) ) ;
#14203 = DIRECTION ( 'NONE',  ( 0.000000000000000000, -0.000000000000000000, -1.000000000000000000 ) ) ;
#14204 = VERTEX_POINT ( 'NONE', #43068 ) ;
#14205 = CARTESIAN_POINT ( 'NONE',  ( 70.91428087927182844, -189.7472609257535510, -33.48461921608517855 ) ) ;
#14206 = CIRCLE ( 'NONE', #11675, 60.00000000000000000 ) ;
#14207 = EDGE_LOOP ( 'NONE', ( #2417, #9207, #22009, #5045 ) ) ;
#14208 = CARTESIAN_POINT ( 'NONE',  ( -332.3517673607765914, -67.40061919120938683, 18.46045550523129819 ) ) ;
#14211 = VERTEX_POINT ( 'NONE', #23105 ) ;
#14210 = CYLINDRICAL_SURFACE ( 'NONE', #44136, 125.0000000000000000 ) ;
#14209 = CYLINDRICAL_SURFACE ( 'NONE', #588, 125.0000000000000000 ) ;
#14212 = VERTEX_POINT ( 'NONE', #992 ) ;
#14213 = AXIS2_PLACEMENT_3D ( 'NONE', #47208, #11435, #50891 ) ;
#14214 = LINE ( 'NONE', #46274, #12248 ) ;
#14215 = VERTEX_POINT ( 'NONE', #8103 ) ;
#14216 = CARTESIAN_POINT ( 'NONE',  ( -332.3517673607765914, -168.7445418633863596, -37.90245108779149064 ) ) ;
#14217 = DIRECTION ( 'NONE',  ( -0.9646355819083556327, 0.000000000000000000, -0.2635871660690782825 ) ) ;
#14218 = ORIENTED_EDGE ( 'NONE', *, *, #1130, .F. ) ;
#14219 = FACE_OUTER_BOUND ( 'NONE', #11680, .T. ) ;
#14220 = CARTESIAN_POINT ( 'NONE',  ( -336.3521761649654422, -173.5513585866778214, -31.34948880313881503 ) ) ;
#14221 = DIRECTION ( 'NONE',  ( 0.000000000000000000, -0.000000000000000000, 1.000000000000000000 ) ) ;
#14222 = CARTESIAN_POINT ( 'NONE',  ( -336.3521761649654422, -80.42027357919624819, -40.34602258462219027 ) ) ;
#14223 = LINE ( 'NONE', #18159, #5623 ) ;
#14224 = ORIENTED_EDGE ( 'NONE', *, *, #24584, .T. ) ;
#14225 = ADVANCED_FACE ( 'NONE', ( #20442 ), #36461, .T. ) ;
#14226 = CARTESIAN_POINT ( 'NONE',  ( -22.62315034598913144, -193.5000000000000000, 121.2748789083720737 ) ) ;
#14227 = CARTESIAN_POINT ( 'NONE',  ( 60.58466639580034752, -175.3837268820161057, -61.07445476073404222 ) ) ;
#14228 = AXIS2_PLACEMENT_3D ( 'NONE', #19812, #5561, #25514 ) ;
#14229 = CARTESIAN_POINT ( 'NONE',  ( 64.44365795514079309, -175.3837268820161057, -53.60452120946194299 ) ) ;
#14230 = ORIENTED_EDGE ( 'NONE', *, *, #20865, .T. ) ;
#14231 = DIRECTION ( 'NONE',  ( -0.000000000000000000, 1.000000000000000000, -0.000000000000000000 ) ) ;
#14232 = DIRECTION ( 'NONE',  ( -0.000000000000000000, 1.000000000000000000, -0.000000000000000000 ) ) ;
#14233 = LINE ( 'NONE', #46045, #882 ) ;
#14234 = DIRECTION ( 'NONE',  ( 0.000000000000000000, -1.000000000000000000, 0.000000000000000000 ) ) ;
#14235 = CARTESIAN_POINT ( 'NONE',  ( 46.00000000000000000, 20.00000000000000000, 0.000000000000000000 ) ) ;
#14236 = AXIS2_PLACEMENT_3D ( 'NONE', #28816, #6220, #29602 ) ;
#14237 = CARTESIAN_POINT ( 'NONE',  ( -47.70260288879080690, -177.1207230881787780, -0.6300878435817026668 ) ) ;
#14238 = EDGE_CURVE ( 'NONE', #32692, #17784, #12812, .T. ) ;
#14239 = DIRECTION ( 'NONE',  ( -0.000000000000000000, 1.000000000000000000, -0.000000000000000000 ) ) ;
#14240 = CARTESIAN_POINT ( 'NONE',  ( -101.0675409952199999, -193.5000000000000000, 113.3995532942341100 ) ) ;
#14241 = AXIS2_PLACEMENT_3D ( 'NONE', #22, #16060, #8168 ) ;
#14242 = VERTEX_POINT ( 'NONE', #8615 ) ;
#14243 = PLANE ( 'NONE',  #15962 ) ;
#14244 = DIRECTION ( 'NONE',  ( 0.000000000000000000, 0.000000000000000000, 1.000000000000000000 ) ) ;
#14246 = VERTEX_POINT ( 'NONE', #20977 ) ;
#14245 = CARTESIAN_POINT ( 'NONE',  ( -330.0000000000000568, -123.5000000000000284, 0.000000000000000000 ) ) ;
#14247 = ORIENTED_EDGE ( 'NONE', *, *, #34821, .T. ) ;
#14248 = ORIENTED_EDGE ( 'NONE', *, *, #800, .F. ) ;
#14249 = PLANE ( 'NONE',  #21707 ) ;
#14250 = EDGE_CURVE ( 'NONE', #24816, #40259, #12169, .T. ) ;
#14251 = CARTESIAN_POINT ( 'NONE',  ( -173.4190745413846457, -193.5000000000000000, -3.874202661594927211 ) ) ;
#14252 = PLANE ( 'NONE',  #50683 ) ;
#14253 = VERTEX_POINT ( 'NONE', #4171 ) ;
#14254 = VECTOR ( 'NONE', #18573, 1000.000000000000000 ) ;
#14255 = CARTESIAN_POINT ( 'NONE',  ( -16.77927958806651887, -183.6283474603465606, -120.9136869416130082 ) ) ;
#14256 = LINE ( 'NONE', #49739, #47898 ) ;
#14259 = VERTEX_POINT ( 'NONE', #24147 ) ;
#14258 = FACE_OUTER_BOUND ( 'NONE', #17031, .T. ) ;
#14257 = DIRECTION ( 'NONE',  ( 0.000000000000000000, 0.000000000000000000, -1.000000000000000000 ) ) ;
#14260 = EDGE_CURVE ( 'NONE', #3183, #2064, #28837, .T. ) ;
#14261 = DIRECTION ( 'NONE',  ( 0.4566292373937200777, 0.000000000000000000, -0.8896570909947436601 ) ) ;
#14262 = ORIENTED_EDGE ( 'NONE', *, *, #5437, .F. ) ;
#14263 = CARTESIAN_POINT ( 'NONE',  ( -48.47912675150885065, -173.5000000000000284, 6.938893903907228378E-15 ) ) ;
#14264 = ORIENTED_EDGE ( 'NONE', *, *, #26783, .F. ) ;
#14265 = CARTESIAN_POINT ( 'NONE',  ( -336.3521761649654422, -181.7525362123217292, 9.724760635742144999 ) ) ;
#14266 = CARTESIAN_POINT ( 'NONE',  ( -72.96029774493612763, -177.1207230881787780, 122.5792489240759551 ) ) ;
#14267 = DIRECTION ( 'NONE',  ( 0.000000000000000000, 0.000000000000000000, 1.000000000000000000 ) ) ;
#14268 = EDGE_CURVE ( 'NONE', #47168, #27526, #48586, .T. ) ;
#14269 = ORIENTED_EDGE ( 'NONE', *, *, #32403, .F. ) ;
#14270 = LINE ( 'NONE', #10322, #46653 ) ;
#14272 = VECTOR ( 'NONE', #14502, 1000.000000000000114 ) ;
#14271 = DIRECTION ( 'NONE',  ( 0.000000000000000000, 1.000000000000000000, 0.000000000000000000 ) ) ;
#14273 = ORIENTED_EDGE ( 'NONE', *, *, #49159, .F. ) ;
#14274 = DIRECTION ( 'NONE',  ( -0.000000000000000000, 1.000000000000000000, 0.000000000000000000 ) ) ;
#14275 = DIRECTION ( 'NONE',  ( -0.000000000000000000, 1.000000000000000000, -0.000000000000000000 ) ) ;
#14276 = ORIENTED_EDGE ( 'NONE', *, *, #34047, .F. ) ;
#14277 = ADVANCED_FACE ( 'NONE', ( #20186 ), #12563, .F. ) ;
#14278 = DIRECTION ( 'NONE',  ( 0.000000000000000000, 0.000000000000000000, 1.000000000000000000 ) ) ;
#14279 = EDGE_CURVE ( 'NONE', #12905, #39518, #48313, .T. ) ;
#14280 = DIRECTION ( 'NONE',  ( 0.000000000000000000, 1.000000000000000000, -3.491481338843133355E-15 ) ) ;
#14281 = PRODUCT ( 'Sliding track', 'Sliding track', '', ( #16277 ) ) ;
#14282 = ORIENTED_EDGE ( 'NONE', *, *, #13790, .T. ) ;
#14283 = DIRECTION ( 'NONE',  ( -0.000000000000000000, -0.2393156642875615969, -0.9709418174260511236 ) ) ;
#14284 = ORIENTED_EDGE ( 'NONE', *, *, #13541, .T. ) ;
#14285 = EDGE_CURVE ( 'NONE', #4817, #23416, #36210, .T. ) ;
#14286 = LINE ( 'NONE', #33982, #13022 ) ;
#14287 = DIRECTION ( 'NONE',  ( 1.000000000000000000, -0.000000000000000000, 0.000000000000000000 ) ) ;
#14288 = EDGE_LOOP ( 'NONE', ( #33198, #8658 ) ) ;
#14289 = DIRECTION ( 'NONE',  ( 0.000000000000000000, -1.000000000000000000, 0.000000000000000000 ) ) ;
#14290 = DIRECTION ( 'NONE',  ( 0.000000000000000000, 0.000000000000000000, 1.000000000000000000 ) ) ;
#14291 = FACE_OUTER_BOUND ( 'NONE', #11206, .T. ) ;
#14292 = AXIS2_PLACEMENT_3D ( 'NONE', #5340, #20307, #45294 ) ;
#14293 = VERTEX_POINT ( 'NONE', #24646 ) ;
#14294 = VECTOR ( 'NONE', #49269, 1000.000000000000000 ) ;
#14295 = FACE_OUTER_BOUND ( 'NONE', #48062, .T. ) ;
#14296 = VERTEX_POINT ( 'NONE', #13082 ) ;
#14297 = DIRECTION ( 'NONE',  ( -1.000000000000000000, 0.000000000000000000, -0.000000000000000000 ) ) ;
#14298 = EDGE_CURVE ( 'NONE', #33552, #6834, #48048, .T. ) ;
#14299 = DIRECTION ( 'NONE',  ( -0.000000000000000000, 0.000000000000000000, 1.000000000000000000 ) ) ;
#14301 = ORIENTED_EDGE ( 'NONE', *, *, #43060, .F. ) ;
#14300 = CARTESIAN_POINT ( 'NONE',  ( -48.13092511607445090, -193.5000000000000000, -0.9374196611341135688 ) ) ;
#14302 = ORIENTED_EDGE ( 'NONE', *, *, #48751, .F. ) ;
#14303 = CARTESIAN_POINT ( 'NONE',  ( -75.48985759771373694, -193.5000000000000000, -122.0467960216648606 ) ) ;
#14304 = EDGE_CURVE ( 'NONE', #34791, #19790, #36996, .T. ) ;
#14305 = DIRECTION ( 'NONE',  ( 0.000000000000000000, 1.000000000000000000, 0.000000000000000000 ) ) ;
#14306 = EDGE_LOOP ( 'NONE', ( #9048, #45523, #22142, #46659 ) ) ;
#14307 = VECTOR ( 'NONE', #25419, 1000.000000000000000 ) ;
#14308 = DIRECTION ( 'NONE',  ( 0.000000000000000000, 1.000000000000000000, 0.000000000000000000 ) ) ;
#14309 = VERTEX_POINT ( 'NONE', #36745 ) ;
#14310 = CARTESIAN_POINT ( 'NONE',  ( -12.10142301649613827, -175.3837268820161057, -118.5439281552630746 ) ) ;
#14311 = DIRECTION ( 'NONE',  ( 0.9646355819083614058, 0.000000000000000000, -0.2635871660690581320 ) ) ;
#14312 = CARTESIAN_POINT ( 'NONE',  ( -332.3517673607765914, -123.5000000000000284, 0.000000000000000000 ) ) ;
#14313 = CARTESIAN_POINT ( 'NONE',  ( -127.0132498732365889, -193.5000000000000000, 97.24912084693261249 ) ) ;
#14314 = VERTEX_POINT ( 'NONE', #40401 ) ;
#14315 = ORIENTED_EDGE ( 'NONE', *, *, #34957, .F. ) ;
#14316 = EDGE_LOOP ( 'NONE', ( #30080, #8241, #22985, #36858 ) ) ;
#14317 = PLANE ( 'NONE',  #33342 ) ;
#14318 = CARTESIAN_POINT ( 'NONE',  ( -114.1105527140175155, -177.1207230881787780, 106.3838142112217611 ) ) ;
#14319 = LINE ( 'NONE', #29306, #24529 ) ;
#14320 = PLANE ( 'NONE',  #32245 ) ;
#14321 = ORIENTED_EDGE ( 'NONE', *, *, #2522, .F. ) ;
#14322 = EDGE_CURVE ( 'NONE', #23058, #17439, #743, .T. ) ;
#14323 = UNCERTAINTY_MEASURE_WITH_UNIT (LENGTH_MEASURE( 1.000000000000000082E-05 ), #38381, 'distance_accuracy_value', 'NONE');
#14324 = EDGE_CURVE ( 'NONE', #26117, #15950, #25180, .T. ) ;
#14325 = FACE_OUTER_BOUND ( 'NONE', #3276, .T. ) ;
#14326 = VECTOR ( 'NONE', #45795, 1000.000000000000000 ) ;
#14327 = VECTOR ( 'NONE', #18233, 1000.000000000000000 ) ;
#14328 = EDGE_LOOP ( 'NONE', ( #30565, #25282, #34102, #17928 ) ) ;
#14329 = EDGE_LOOP ( 'NONE', ( #25019, #17401, #37000, #47201 ) ) ;
#14330 = DIRECTION ( 'NONE',  ( -0.000000000000000000, 1.000000000000000000, -0.000000000000000000 ) ) ;
#14331 = LINE ( 'NONE', #3525, #51866 ) ;
#14332 = DIRECTION ( 'NONE',  ( 0.000000000000000000, 0.000000000000000000, 1.000000000000000000 ) ) ;
#14333 = DIRECTION ( 'NONE',  ( -1.000000000000000000, 0.000000000000000000, 0.000000000000000000 ) ) ;
#14334 = LINE ( 'NONE', #49827, #1577 ) ;
#14335 = ORIENTED_EDGE ( 'NONE', *, *, #10062, .T. ) ;
#14336 = EDGE_CURVE ( 'NONE', #45141, #15701, #29850, .T. ) ;
#14337 = CARTESIAN_POINT ( 'NONE',  ( 71.87891646118019651, -193.5000000000000000, -33.74820638215424395 ) ) ;
#14338 = EDGE_LOOP ( 'NONE', ( #44953, #37118, #47559, #19551 ) ) ;
#14339 = ADVANCED_FACE ( 'NONE', ( #8880 ), #24917, .T. ) ;
#14340 = ORIENTED_EDGE ( 'NONE', *, *, #39930, .T. ) ;
#14341 = CARTESIAN_POINT ( 'NONE',  ( -336.3521761649654422, -77.59233547837267508, 37.15394033962009246 ) ) ;
#14342 = EDGE_CURVE ( 'NONE', #25441, #10943, #4958, .T. ) ;
#14343 = VECTOR ( 'NONE', #49551, 1000.000000000000000 ) ;
#14344 = CARTESIAN_POINT ( 'NONE',  ( -48.47912675150885065, -177.1207230881787780, 6.938893903907228378E-15 ) ) ;
#14345 = ORIENTED_EDGE ( 'NONE', *, *, #45609, .F. ) ;
#14346 = EDGE_CURVE ( 'NONE', #13514, #18828, #5216, .T. ) ;
#14347 = LINE ( 'NONE', #34054, #26544 ) ;
#14348 = PLANE ( 'NONE',  #48195 ) ;
#14349 = LINE ( 'NONE', #10392, #17301 ) ;
#14350 = DIRECTION ( 'NONE',  ( -1.000000000000000000, 0.000000000000000000, 0.000000000000000000 ) ) ;
#14351 = CARTESIAN_POINT ( 'NONE',  ( -142.2007120195389405, -183.6283474603465606, 81.19354792697799894 ) ) ;
#14352 = ORIENTED_EDGE ( 'NONE', *, *, #39480, .F. ) ;
#14353 = LINE ( 'NONE', #43504, #33059 ) ;
#14354 = ORIENTED_EDGE ( 'NONE', *, *, #11242, .F. ) ;
#14355 = CIRCLE ( 'NONE', #43721, 124.9999999999999858 ) ;
#14356 = ORIENTED_EDGE ( 'NONE', *, *, #33503, .F. ) ;
#14357 = DIRECTION ( 'NONE',  ( 0.000000000000000000, -1.000000000000000000, 0.000000000000000000 ) ) ;
#14358 = VERTEX_POINT ( 'NONE', #3001 ) ;
#14359 = AXIS2_PLACEMENT_3D ( 'NONE', #37625, #42325, #26560 ) ;
#14360 = DIRECTION ( 'NONE',  ( 0.000000000000000000, 0.000000000000000000, -1.000000000000000000 ) ) ;
#14361 = ORIENTED_EDGE ( 'NONE', *, *, #11119, .T. ) ;
#14362 = DIRECTION ( 'NONE',  ( 1.000000000000000000, -0.000000000000000000, -0.000000000000000000 ) ) ;
#14363 = CARTESIAN_POINT ( 'NONE',  ( -336.3521761649654422, -149.4733471526596134, 53.00046796564699036 ) ) ;
#14364 = ORIENTED_EDGE ( 'NONE', *, *, #20088, .F. ) ;
#14365 = FACE_OUTER_BOUND ( 'NONE', #45629, .T. ) ;
#14366 = CARTESIAN_POINT ( 'NONE',  ( -167.8725343822893308, -175.3837268820161057, 33.48461921608600278 ) ) ;
#14367 = CARTESIAN_POINT ( 'NONE',  ( -150.5215542367829471, -189.7472609257535510, -72.19655804061974891 ) ) ;
#14368 = ORIENTED_EDGE ( 'NONE', *, *, #14390, .T. ) ;
#14369 = EDGE_LOOP ( 'NONE', ( #13869, #27468, #38682, #3519 ) ) ;
#14370 = EDGE_LOOP ( 'NONE', ( #19562, #14335, #20704, #11055 ) ) ;
#14371 = LINE ( 'NONE', #39042, #23399 ) ;
#14372 = LINE ( 'NONE', #19101, #38591 ) ;
#14373 = VECTOR ( 'NONE', #42683, 1000.000000000000114 ) ;
#14374 = EDGE_CURVE ( 'NONE', #51005, #885, #37518, .T. ) ;
#14375 = CARTESIAN_POINT ( 'NONE',  ( -336.3521761649654422, -80.37812621821328207, -41.71934804796994456 ) ) ;
#14376 = LINE ( 'NONE', #51177, #5194 ) ;
#14377 = CARTESIAN_POINT ( 'NONE',  ( -48.47912675150885065, -175.3837268820161057, 6.938893903907228378E-15 ) ) ;
#14378 = EDGE_LOOP ( 'NONE', ( #37693, #48654, #15338, #45853 ) ) ;
#14379 = EDGE_CURVE ( 'NONE', #23944, #3885, #48311, .T. ) ;
#14380 = EDGE_CURVE ( 'NONE', #11828, #7505, #18122, .T. ) ;
#14381 = ADVANCED_FACE ( 'NONE', ( #17566 ), #31116, .F. ) ;
#14382 = EDGE_CURVE ( 'NONE', #48981, #43364, #5532, .T. ) ;
#14383 = PLANE ( 'NONE',  #29073 ) ;
#14384 = VERTEX_POINT ( 'NONE', #38991 ) ;
#14386 = ORIENTED_EDGE ( 'NONE', *, *, #28558, .F. ) ;
#14385 = CARTESIAN_POINT ( 'NONE',  ( -142.9772358822569629, -177.1207230881787780, 81.82363577055969017 ) ) ;
#14387 = VERTEX_POINT ( 'NONE', #10634 ) ;
#14388 = EDGE_CURVE ( 'NONE', #45944, #17630, #19043, .T. ) ;
#14389 = CARTESIAN_POINT ( 'NONE',  ( 11.61413489515541997, -183.6283474603465606, -109.6074810615842381 ) ) ;
#14390 = EDGE_CURVE ( 'NONE', #38746, #45026, #23152, .T. ) ;
#14391 = ORIENTED_EDGE ( 'NONE', *, *, #14413, .T. ) ;
#14392 = DIRECTION ( 'NONE',  ( 1.000000000000000000, -0.000000000000000000, -0.000000000000000000 ) ) ;
#14393 = VECTOR ( 'NONE', #10661, 1000.000000000000000 ) ;
#14394 = ORIENTED_EDGE ( 'NONE', *, *, #50887, .T. ) ;
#14395 = FACE_OUTER_BOUND ( 'NONE', #50647, .T. ) ;
#14396 = DIRECTION ( 'NONE',  ( 0.000000000000000000, 0.000000000000000000, 1.000000000000000000 ) ) ;
#14397 = ORIENTED_EDGE ( 'NONE', *, *, #52036, .F. ) ;
#14398 = EDGE_CURVE ( 'NONE', #28486, #23944, #5740, .T. ) ;
#14399 = DIRECTION ( 'NONE',  ( 0.2348860457809707758, 0.000000000000000000, 0.9720229140804138579 ) ) ;
#14400 = VECTOR ( 'NONE', #4914, 1000.000000000000114 ) ;
#14401 = ORIENTED_EDGE ( 'NONE', *, *, #30458, .F. ) ;
#14402 = EDGE_CURVE ( 'NONE', #18133, #40906, #8878, .T. ) ;
#14403 = CIRCLE ( 'NONE', #22762, 125.0000000000000000 ) ;
#14404 = ORIENTED_EDGE ( 'NONE', *, *, #14054, .T. ) ;
#14405 = CARTESIAN_POINT ( 'NONE',  ( -151.5051191635538146, -193.5000000000000000, -69.00559874123520387 ) ) ;
#14406 = DIRECTION ( 'NONE',  ( 0.9960498426152171181, 0.000000000000000000, -0.08879589532293157006 ) ) ;
#14407 = ADVANCED_FACE ( 'NONE', ( #30868 ), #37771, .F. ) ;
#14408 = LINE ( 'NONE', #46218, #37079 ) ;
#14409 = LINE ( 'NONE', #7993, #18190 ) ;
#14410 = ORIENTED_EDGE ( 'NONE', *, *, #32061, .T. ) ;
#14411 = CARTESIAN_POINT ( 'NONE',  ( -1.771278280434267272, -177.1207230881787780, -115.9455772817710226 ) ) ;
#14412 = LINE ( 'NONE', #42513, #23938 ) ;
#14413 = EDGE_CURVE ( 'NONE', #3228, #11975, #5476, .T. ) ;
#14414 = ITEM_DEFINED_TRANSFORMATION ( 'NONE', 'NONE', #51091,  #31742 ) ;
#14415 = DIRECTION ( 'NONE',  ( 0.8757349421956345248, 0.000000000000000000, 0.4827922027307490205 ) ) ;
#14416 = CARTESIAN_POINT ( 'NONE',  ( -332.3517673607765914, -93.75055682584159911, 51.01861988938794923 ) ) ;
#14417 = VERTEX_POINT ( 'NONE', #18777 ) ;
#14418 = DIRECTION ( 'NONE',  ( 0.000000000000000000, 1.000000000000000000, 0.000000000000000000 ) ) ;
#14419 = CYLINDRICAL_SURFACE ( 'NONE', #518, 124.9999999999999858 ) ;
#14420 = AXIS2_PLACEMENT_3D ( 'NONE', #21270, #25985, #17346 ) ;
#14421 = EDGE_CURVE ( 'NONE', #2171, #41684, #33321, .T. ) ;
#14422 = CARTESIAN_POINT ( 'NONE',  ( -75.48985759771373694, -193.5000000000000000, -122.0467960216648606 ) ) ;
#14423 = ORIENTED_EDGE ( 'NONE', *, *, #16107, .T. ) ;
#14424 = AXIS2_PLACEMENT_3D ( 'NONE', #9401, #9656, #13593 ) ;
#14425 = LINE ( 'NONE', #10460, #11296 ) ;
#14426 = DIRECTION ( 'NONE',  ( -0.4300652022765304450, 0.000000000000000000, 0.9027978299657387629 ) ) ;
#14427 = ORIENTED_EDGE ( 'NONE', *, *, #47868, .T. ) ;
#14428 = DIRECTION ( 'NONE',  ( 0.000000000000000000, 1.000000000000000000, 0.000000000000000000 ) ) ;
#14429 = EDGE_LOOP ( 'NONE', ( #21958, #30085, #45470, #16901 ) ) ;
#14430 = EDGE_CURVE ( 'NONE', #39637, #28728, #33189, .T. ) ;
#14431 = PLANE ( 'NONE',  #9175 ) ;
#14432 = CARTESIAN_POINT ( 'NONE',  ( -3.104056038602969636, -177.1207230881787780, -115.4006183233321536 ) ) ;
#14433 = CARTESIAN_POINT ( 'NONE',  ( -305.0000000000000568, -123.5000000000000284, -20.00000000000001066 ) ) ;
#14434 = AXIS2_PLACEMENT_3D ( 'NONE', #12633, #48395, #51829 ) ;
#14435 = CARTESIAN_POINT ( 'NONE',  ( -336.3521761649654422, -126.1322888500942270, -59.00000000000001421 ) ) ;
#14436 = AXIS2_PLACEMENT_3D ( 'NONE', #44582, #49050, #48549 ) ;
#14437 = PLANE ( 'NONE',  #23495 ) ;
#14438 = ORIENTED_EDGE ( 'NONE', *, *, #27691, .T. ) ;
#14439 = VECTOR ( 'NONE', #23968, 1000.000000000000000 ) ;
#14440 = CYLINDRICAL_SURFACE ( 'NONE', #3813, 4.999999999999997335 ) ;
#14441 = ORIENTED_EDGE ( 'NONE', *, *, #43976, .F. ) ;
#14442 = EDGE_CURVE ( 'NONE', #31192, #41489, #26471, .T. ) ;
#14443 = CARTESIAN_POINT ( 'NONE',  ( -336.3521761649654422, -140.4009141470556870, -57.57047073799078873 ) ) ;
#14444 = ORIENTED_EDGE ( 'NONE', *, *, #7325, .T. ) ;
#14445 = DIRECTION ( 'NONE',  ( 0.000000000000000000, -0.000000000000000000, -1.000000000000000000 ) ) ;
#14446 = EDGE_CURVE ( 'NONE', #232, #51884, #10894, .T. ) ;
#14447 = EDGE_CURVE ( 'NONE', #21989, #31290, #9409, .T. ) ;
#14448 = EDGE_CURVE ( 'NONE', #35821, #10145, #47496, .T. ) ;
#14449 = AXIS2_PLACEMENT_3D ( 'NONE', #14300, #38192, #1691 ) ;
#14450 = ADVANCED_FACE ( 'NONE', ( #6705 ), #22722, .F. ) ;
#14451 = DIRECTION ( 'NONE',  ( -1.000000000000000000, 0.000000000000000000, -0.000000000000000000 ) ) ;
#14452 = LINE ( 'NONE', #25756, #28108 ) ;
#14453 = EDGE_LOOP ( 'NONE', ( #6161, #48211, #10993, #4800 ) ) ;
#14456 = EDGE_LOOP ( 'NONE', ( #27565, #34564 ) ) ;
#14455 = LINE ( 'NONE', #30982, #5481 ) ;
#14454 = DIRECTION ( 'NONE',  ( 0.000000000000000000, 0.000000000000000000, 1.000000000000000000 ) ) ;
#14457 = AXIS2_PLACEMENT_3D ( 'NONE', #41560, #17427, #49727 ) ;
#14458 = VECTOR ( 'NONE', #13006, 1000.000000000000000 ) ;
#14459 = PLANE ( 'NONE',  #13039 ) ;
#14460 = ORIENTED_EDGE ( 'NONE', *, *, #34658, .F. ) ;
#14461 = CARTESIAN_POINT ( 'NONE',  ( -305.0000000000000568, -111.7106844931459761, -58.83036664750484590 ) ) ;
#14462 = VERTEX_POINT ( 'NONE', #7209 ) ;
#14463 = CARTESIAN_POINT ( 'NONE',  ( -48.02249751411513756, -175.3837268820161057, -0.8896570909947397743 ) ) ;
#14466 = EDGE_LOOP ( 'NONE', ( #1231, #3427, #49212, #20497 ) ) ;
#14465 = DIRECTION ( 'NONE',  ( 0.000000000000000000, -0.000000000000000000, 1.000000000000000000 ) ) ;
#14464 = PLANE ( 'NONE',  #31652 ) ;
#14467 = ORIENTED_EDGE ( 'NONE', *, *, #25595, .F. ) ;
#14468 = CARTESIAN_POINT ( 'NONE',  ( 47.91692961953209107, -175.3837268820161057, -77.99872144864700374 ) ) ;
#14469 = VERTEX_POINT ( 'NONE', #23249 ) ;
#14470 = FACE_OUTER_BOUND ( 'NONE', #49496, .T. ) ;
#14471 = CARTESIAN_POINT ( 'NONE',  ( -116.2964108826154188, -183.6283474603465606, -105.0038855142073402 ) ) ;
#14472 = EDGE_CURVE ( 'NONE', #32376, #30580, #15362, .T. ) ;
#14473 = ORIENTED_EDGE ( 'NONE', *, *, #25390, .T. ) ;
#14474 = LINE ( 'NONE', #38375, #2034 ) ;
#14475 = CARTESIAN_POINT ( 'NONE',  ( -25.72842157752850056, -175.3837268820161057, 121.8950816227734606 ) ) ;
#14476 = PLANE ( 'NONE',  #26574 ) ;
#14477 = LINE ( 'NONE', #41813, #49532 ) ;
#14478 = VECTOR ( 'NONE', #29382, 1000.000000000000114 ) ;
#14479 = DIRECTION ( 'NONE',  ( -0.02963332782257007553, 0.000000000000000000, 0.9995608365087941261 ) ) ;
#14480 = EDGE_CURVE ( 'NONE', #49617, #19338, #46641, .T. ) ;
#14481 = VERTEX_POINT ( 'NONE', #36092 ) ;
#14482 = DIRECTION ( 'NONE',  ( 0.000000000000000000, 0.000000000000000000, -1.000000000000000000 ) ) ;
#14483 = CARTESIAN_POINT ( 'NONE',  ( -332.3517673607765914, -180.1556192733800117, 16.67542351306693149 ) ) ;
#14484 = EDGE_CURVE ( 'NONE', #35254, #31290, #2993, .T. ) ;
#14485 = AXIS2_PLACEMENT_3D ( 'NONE', #8997, #45520, #25033 ) ;
#14486 = PLANE ( 'NONE',  #7795 ) ;
#14487 = ORIENTED_EDGE ( 'NONE', *, *, #45099, .T. ) ;
#14488 = DIRECTION ( 'NONE',  ( -0.000000000000000000, 1.000000000000000000, -0.000000000000000000 ) ) ;
#14489 = CARTESIAN_POINT ( 'NONE',  ( -151.9915035862630646, -177.1207230881787780, 70.07273251429431582 ) ) ;
#14490 = DIRECTION ( 'NONE',  ( -0.5586467658036476935, 0.000000000000000000, -0.8294056854502049880 ) ) ;
#14491 = CARTESIAN_POINT ( 'NONE',  ( -170.2790847791494855, -177.1207230881787780, -28.10285082451569494 ) ) ;
#14492 = ORIENTED_EDGE ( 'NONE', *, *, #27666, .F. ) ;
#14493 = AXIS2_PLACEMENT_3D ( 'NONE', #43887, #44147, #12866 ) ;
#14494 = VECTOR ( 'NONE', #25897, 1000.000000000000000 ) ;
#14495 = DIRECTION ( 'NONE',  ( 0.000000000000000000, -0.000000000000000000, -1.000000000000000000 ) ) ;
#14496 = VECTOR ( 'NONE', #45701, 1000.000000000000000 ) ;
#14497 = VECTOR ( 'NONE', #44241, 1000.000000000000000 ) ;
#14498 = LINE ( 'NONE', #42599, #25348 ) ;
#14499 = CARTESIAN_POINT ( 'NONE',  ( -8.169009709621407822, -177.1207230881787780, 118.3219948448695504 ) ) ;
#14500 = LINE ( 'NONE', #51032, #5266 ) ;
#14501 = ORIENTED_EDGE ( 'NONE', *, *, #45334, .T. ) ;
#14502 = DIRECTION ( 'NONE',  ( -0.6528221181905280446, 0.000000000000000000, 0.7575112421616145841 ) ) ;
#14503 = CARTESIAN_POINT ( 'NONE',  ( -49.42645310536303782, -177.1207230881787780, -0.3202698538628417357 ) ) ;
#14504 = EDGE_LOOP ( 'NONE', ( #25439, #47748, #44519, #2033 ) ) ;
#14505 = ORIENTED_EDGE ( 'NONE', *, *, #24103, .T. ) ;
#14506 = ORIENTED_EDGE ( 'NONE', *, *, #50726, .T. ) ;
#14507 = DIRECTION ( 'NONE',  ( 0.9720229140804123036, 0.000000000000000000, -0.2348860457809775759 ) ) ;
#14508 = AXIS2_PLACEMENT_3D ( 'NONE', #32493, #40614, #41152 ) ;
#14509 = EDGE_CURVE ( 'NONE', #26098, #7181, #13922, .T. ) ;
#14510 = EDGE_CURVE ( 'NONE', #19179, #20432, #40278, .T. ) ;
#14511 = FACE_OUTER_BOUND ( 'NONE', #44415, .T. ) ;
#14512 = FACE_OUTER_BOUND ( 'NONE', #32389, .T. ) ;
#14513 = ORIENTED_EDGE ( 'NONE', *, *, #15402, .F. ) ;
#14514 = VECTOR ( 'NONE', #13973, 1000.000000000000000 ) ;
#14515 = LINE ( 'NONE', #27090, #43492 ) ;
#14516 = PLANE ( 'NONE',  #16018 ) ;
#14519 = ORIENTED_EDGE ( 'NONE', *, *, #44887, .T. ) ;
#14518 = CARTESIAN_POINT ( 'NONE',  ( -336.3521761649654422, -173.5513585866778214, -31.34948880313881503 ) ) ;
#14517 = DIRECTION ( 'NONE',  ( -0.000000000000000000, 1.000000000000000000, -0.000000000000000000 ) ) ;
#14520 = CARTESIAN_POINT ( 'NONE',  ( -48.65601702663143868, -193.5000000000000000, 0.9842305779476024918 ) ) ;
#14521 = VERTEX_POINT ( 'NONE', #23499 ) ;
#14522 = LINE ( 'NONE', #26592, #38974 ) ;
#14523 = ORIENTED_EDGE ( 'NONE', *, *, #51071, .F. ) ;
#14524 = DIRECTION ( 'NONE',  ( 0.000000000000000000, 1.000000000000000000, 0.000000000000000000 ) ) ;
#14525 = CARTESIAN_POINT ( 'NONE',  ( 43.18784210722336780, -189.7472609257535510, -84.98333260264752198 ) ) ;
#14526 = PLANE ( 'NONE',  #37470 ) ;
#14527 = CIRCLE ( 'NONE', #43879, 125.0000000000000000 ) ;
#14528 = AXIS2_PLACEMENT_3D ( 'NONE', #17855, #1298, #45993 ) ;
#14529 = AXIS2_PLACEMENT_3D ( 'NONE', #31924, #47962, #7754 ) ;
#14530 = EDGE_LOOP ( 'NONE', ( #4810, #50780, #36365, #35468 ) ) ;
#14531 = VECTOR ( 'NONE', #15083, 1000.000000000000000 ) ;
#14532 = FACE_OUTER_BOUND ( 'NONE', #31807, .T. ) ;
#14533 = CARTESIAN_POINT ( 'NONE',  ( 57.61256176024322428, -193.5000000000000000, -64.19309449102732401 ) ) ;
#14534 = EDGE_LOOP ( 'NONE', ( #15913, #47480 ) ) ;
#14535 = EDGE_CURVE ( 'NONE', #49769, #6620, #50840, .T. ) ;
#14536 = DIRECTION ( 'NONE',  ( 0.000000000000000000, 0.000000000000000000, -1.000000000000000000 ) ) ;
#14537 = DIRECTION ( 'NONE',  ( 0.000000000000000000, 0.000000000000000000, 1.000000000000000000 ) ) ;
#14538 = EDGE_LOOP ( 'NONE', ( #12305, #25554, #11118, #27180 ) ) ;
#14539 = DIRECTION ( 'NONE',  ( 0.000000000000000000, 0.000000000000000000, 1.000000000000000000 ) ) ;
#14540 = CLOSED_SHELL ( 'NONE', ( #26600, #22889, #17432, #9243, #24067, #20478, #44637, #7014, #18969, #1952, #31723, #1501, #2691, #22480, #4851, #43630, #49599, #28438, #31811, #25525, #8330, #44454, #24460, #3789, #4661, #9767, #33319, #16052, #49049, #36568, #30013, #25813, #38141, #12415, #13458, #11486, #33301, #42080, #16354, #26548, #9163, #46801, #21140, #24285, #29391, #43921, #6404, #39523, #30098, #9765, #37012, #46639, #418, #9594, #44955, #6962, #20082, #7116, #25296, #26635, #32646, #11807, #8491, #48180, #40069, #5326, #20813, #25543, #15460, #38172, #23811, #2845, #10694, #30536, #5128, #19559, #19961, #39052, #44880, #17456, #49337, #40292, #35929, #50078, #28482, #44309, #13611, #44944, #27268, #14138, #42524, #25031, #34660, #1753, #13059, #47582, #36927, #36861, #26642, #10515, #49493, #1793, #36207, #15699, #35862, #22473, #23521, #39620, #7566, #40466, #2852, #9285, #19044, #2177, #25861, #41430, #35687, #9577, #44019, #21941, #22316, #48403, #47500, #26527, #712, #5594, #10883, #562, #17927, #37899, #48519, #45580, #16958, #39127, #47222, #597, #11457, #13789, #35372, #28076, #11028, #9640, #31651, #46254, #13735, #46367, #1808, #34323, #12094, #12472, #24126, #42706, #35876, #34312, #36386, #39638, #36882, #18912, #3072, #4874, #15718, #15579, #20126, #1196, #9187, #20164, #3886, #19595, #49976, #18689, #8155, #7660, #29458, #23407, #16720, #21130, #32993, #1727, #2256, #40699, #36032, #42396, #29642, #8796, #192, #32251, #43326, #19893, #5283, #15994, #15722, #18276, #26967, #22686, #35566, #48150, #20661, #45442, #39896, #51285, #33235, #16953, #309, #5368, #48085, #27895, #5501, #35921, #33088, #14947, #17826, #3412, #11532, #26321, #49293, #35373, #21524, #25052, #28571, #611, #44304, #43579, #22342, #6103, #39462, #44376, #35604, #44472, #27197, #36728, #19841, #16066, #48790, #35167, #45902, #7282, #19274, #51394, #3111, #37516, #4976, #38007, #23248, #2459, #32720, #32770, #29731, #12710, #9283, #41921, #12476, #30254, #7092, #30061, #37746, #42499, #1220, #32591, #41426, #44870, #51845, #32994, #38347, #14791, #42328, #40832, #16673, #1212, #24299, #17906, #18886, #932, #33387, #25039, #19218, #23722, #6249, #13284, #46988, #24762, #21752, #28539, #42188, #17129, #36302, #40884, #8827, #13451, #42680, #4301, #40646, #9458, #1944, #20975, #43291, #15081, #20793, #4792, #42658, #6690, #43152, #12117, #13389, #2636, #29794, #30160, #38527, #24638, #18337, #26488, #16108, #45340, #33252, #22229, #33441, #39176, #50864, #2513, #24340, #33411, #8550, #47486, #34556, #43541, #253, #31034, #3238, #42765, #8267, #24972, #6334, #34839, #16356, #5976, #12037, #15341, #31478, #44240, #26141, #46164, #6617, #31169, #43518, #30802, #52021, #13309, #28979, #14099, #43637, #9898, #19082, #15741, #15395, #27841, #19901, #41154, #45531, #22148, #26670, #33207, #39948, #26008, #44824, #30194, #14407, #19837, #26006, #29395, #6616, #27772, #8205, #31472, #47756, #25907, #24698, #9083, #8926, #29436, #42197, #49868, #44446, #50757, #3841, #4466, #23568, #25308, #46291, #40595, #33698, #28495, #29435, #23738, #8917, #17, #17184, #24427, #2809, #37148, #26883, #45318, #3193, #7059, #19256, #16585, #2194, #26163, #29484, #29146, #9376, #34280, #41228, #38959, #16658, #37049, #40420, #22160, #43865, #51486, #15582, #11815, #4084, #38220, #9723, #16963, #20368, #33461, #22761, #48182, #9832, #38160, #42017, #13461, #3752, #29276, #20299, #5099, #30788, #36886, #32701, #29707, #34833, #4238, #42084, #8780, #51088, #45873, #43397, #16774, #27847, #47513, #31424, #50201, #39981, #30642, #41594, #20545, #45258, #5677, #45427, #11523, #46213, #40577, #24826, #35334, #48984, #50009, #17946, #49474, #27787, #12751, #35496, #22744, #13060, #13729, #33939, #47082, #34195, #29885, #14843, #17316, #17332, #26552, #47476, #32899, #20851, #5386, #38852, #46286, #17901, #12105, #25903, #21433, #17487, #17966, #34988, #25357, #32072, #37102, #11673, #5899, #46050, #33012, #34717, #29508, #24309, #43622, #7083, #25600, #37108, #26063, #12519, #47144, #17372, #43687, #5044, #31942, #16058, #13128, #14225, #50141, #40448, #15165, #21212, #29323, #3168, #13473, #13009, #45799, #3351, #40122, #21234, #35534, #18599, #27826, #43118, #9941, #8028, #51664, #15112, #15060, #48011, #21435, #40139, #50066, #28013, #20741, #37218, #48101, #43511, #3761, #30528, #25937, #30744, #23045, #8486, #27134, #7022, #35497, #32071, #16361, #35974, #6531, #44461, #44954, #39502, #36504, #37748, #17554, #45981, #44826, #25199, #50061, #30394, #11412, #22765, #50492, #46847, #26973, #18390, #18592, #49470, #33958, #43141, #3215, #4187, #34332, #23412, #48574, #50105, #51240, #1260, #34345, #34775, #16223, #50718, #22784, #36205, #32137, #23396, #12253, #34036, #37002, #39036, #22826, #28205, #16939, #1287, #1526, #6036, #24761, #33365, #36322, #29144, #14718, #41008, #33849, #51507, #48991, #6678, #4479, #11101, #27264, #16298, #31289, #19604, #7328, #1146, #25214, #45932, #41162, #3819, #21294, #7043, #37469, #46436, #31960, #1306, #34314, #31782, #682, #28253, #25291, #51955, #51470, #35277, #51299, #46684, #46552, #41363, #19016, #43349, #51026, #30441, #44918, #27216, #29394, #31916, #47798, #13492, #38185, #33883, #22101, #40965, #42010, #10387, #41026, #9875, #28835, #18180, #2529, #7760, #38763, #41247, #36743, #32665, #16501, #15733, #9055, #48764, #18489, #21658, #6116, #15217, #15054, #35213, #37542, #48545, #39400, #39415, #9253, #4088, #30509, #18580, #11170, #28726, #44740, #3691, #20923, #3389, #35549, #26091, #12345, #21851, #44771, #20627, #7373, #31845, #9491, #12889, #5453, #11699, #37886, #4223, #28178, #40070, #47855, #26185, #43617, #45537, #35421, #40395, #2472, #10600, #50704, #24872, #31795, #36559, #14691, #28898, #46667, #29030, #46064, #35105, #18663, #51521, #23430, #50689, #11104, #39459, #48818, #22459, #1390, #270, #37808, #4434, #4775, #37282, #47553, #6413, #18196, #47956, #51016, #25641, #1512, #8948, #26799, #10771, #50411, #21213, #9524, #29806, #4517, #15067, #12483, #546, #38467, #43528, #8324, #1131, #51995, #26299, #40276, #32066, #25417, #43327, #10836, #29658, #18179, #236, #763, #6267, #49766, #21184, #41317, #15166, #15328, #39838, #20124, #30613, #42044, #15480, #16126, #16652, #29683, #18755, #21804, #24486, #16937, #16289, #52032, #27956, #6471, #42639, #11352, #17910, #6689, #7187, #35342, #30935, #14277, #14632, #45617, #33650, #10612, #41448, #11067, #51416, #25989, #31413, #5768, #29515, #40649, #44874, #49909, #3358, #42772, #37192, #27667, #27261, #47753, #50695, #46916, #9239, #13316, #45532, #37222, #35924, #40337, #10171, #50406, #5137, #38547, #46557, #39460, #8445, #702, #7211, #7811, #5387, #23036, #29812, #43683, #50301, #6871, #28145, #11157, #7247, #36928, #47152, #16311, #1442, #22945, #38588, #45626, #19464, #30198, #51980, #26304, #15216, #11817, #7323, #37989, #4647, #30174, #22759, #36859, #44161, #5887, #2908, #49815, #27625, #31456, #15696, #23308, #32830, #18311, #27916, #561, #45487, #1570, #18013, #36114, #21055, #31983, #35281, #2482, #34739, #22095, #21390, #45543, #1638, #35847, #27587, #45560, #19229, #12944, #9885, #2862, #37401, #13079, #4795, #29239, #11545, #11409, #13088, #42066, #7738, #33938, #2144, #1764, #17298, #22449, #37163, #41103, #43034, #7736, #15422, #34688, #30444, #48629, #5198, #33259, #11835, #44726, #35209, #21818, #47200, #12834, #18603, #2830, #24961, #47589, #9312, #51348, #49115, #23923, #44596, #8978, #14743, #1655, #28190, #41393, #42613, #44121, #12950, #25848, #46999, #15942, #36907, #46845, #31647, #35783, #37449, #46779, #1640, #36692, #6131, #37288, #25644, #29684, #29501, #8501, #5829, #8876, #16584, #7320, #16932, #10178, #36782, #25358, #23056, #3755, #9428, #44932, #10255, #41953, #17668, #27630, #35623, #7753, #25293, #3701, #16695, #41221, #39984, #15047, #39360, #10407, #15355, #27066, #36216, #4728, #38605, #1721, #28606, #48679, #45623, #12474, #44957, #40706, #35147, #5614, #4675, #10291, #31418, #32505, #18245, #19773, #39744, #6021, #9056, #1070, #42956, #48972, #34909, #16715, #10903, #21455, #26271, #23869, #37373, #41067, #10625, #23471, #2711, #8279, #21436, #33093, #33122, #26672, #51379, #50740, #12772, #33393, #50652, #43811, #37213, #38990, #28998, #28665, #49710, #613, #27537, #3333, #20722, #49684, #40763, #28518, #42200, #35026, #25317, #47924, #42967, #51356, #27495, #22752, #37255, #17794, #15337, #16562, #13230, #23445, #3454, #27119, #26958, #39239, #6378, #42336, #51585, #26064, #26298, #3124, #48603, #51675, #10289, #26901, #16182, #36545, #14450, #7573 ) ) ;
#14541 = DIRECTION ( 'NONE',  ( 0.000000000000000000, -0.7485107481711046340, -0.6631226582407911962 ) ) ;
#14542 = EDGE_CURVE ( 'NONE', #3584, #6218, #39070, .T. ) ;
#14543 = ORIENTED_EDGE ( 'NONE', *, *, #21289, .T. ) ;
#14544 = CARTESIAN_POINT ( 'NONE',  ( -339.1964088526558498, -64.86990808808704401, 6.615309698014191220 ) ) ;
#14545 = ORIENTED_EDGE ( 'NONE', *, *, #25607, .F. ) ;
#14546 = CARTESIAN_POINT ( 'NONE',  ( -332.3517673607765914, -93.31268025388605736, 51.85292399224828586 ) ) ;
#14547 = CARTESIAN_POINT ( 'NONE',  ( -330.4913330509368166, -171.7720157143604069, -33.92731199008473197 ) ) ;
#14548 = VERTEX_POINT ( 'NONE', #48193 ) ;
#14549 = AXIS2_PLACEMENT_3D ( 'NONE', #51509, #30491, #14482 ) ;
#14550 = DIRECTION ( 'NONE',  ( 0.000000000000000000, -0.8660254037844354880, -0.5000000000000054401 ) ) ;
#14551 = LINE ( 'NONE', #38699, #49092 ) ;
#14552 = DIRECTION ( 'NONE',  ( 0.000000000000000000, -0.000000000000000000, -1.000000000000000000 ) ) ;
#14553 = AXIS2_PLACEMENT_3D ( 'NONE', #3489, #35541, #40257 ) ;
#14554 = EDGE_LOOP ( 'NONE', ( #19755, #1634, #48038, #40314 ) ) ;
#14555 = LINE ( 'NONE', #42132, #17051 ) ;
#14556 = ORIENTED_EDGE ( 'NONE', *, *, #2601, .T. ) ;
#14557 = FACE_OUTER_BOUND ( 'NONE', #40527, .T. ) ;
#14558 = DIRECTION ( 'NONE',  ( 0.9995608365087944591, 0.000000000000000000, -0.02963332782255633305 ) ) ;
#14560 = VERTEX_POINT ( 'NONE', #43978 ) ;
#14559 = DIRECTION ( 'NONE',  ( 0.9646355819083594074, 0.000000000000000000, -0.2635871660690647933 ) ) ;
#14561 = ORIENTED_EDGE ( 'NONE', *, *, #18087, .T. ) ;
#14562 = LINE ( 'NONE', #46890, #45089 ) ;
#14563 = VECTOR ( 'NONE', #37910, 1000.000000000000114 ) ;
#14564 = EDGE_CURVE ( 'NONE', #36416, #31403, #19547, .T. ) ;
#14565 = PLANE ( 'NONE',  #12847 ) ;
#14566 = AXIS2_PLACEMENT_3D ( 'NONE', #941, #44835, #158 ) ;
#14567 = ORIENTED_EDGE ( 'NONE', *, *, #20200, .T. ) ;
#14568 = CARTESIAN_POINT ( 'NONE',  ( 71.15591247552653442, -183.6283474603465606, 36.22785377504035154 ) ) ;
#14569 = ORIENTED_EDGE ( 'NONE', *, *, #3479, .T. ) ;
#14570 = DIRECTION ( 'NONE',  ( 0.000000000000000000, -1.000000000000000000, -0.000000000000000000 ) ) ;
#14571 = CARTESIAN_POINT ( 'NONE',  ( -140.5933766095837427, -189.7472609257535510, -84.49831343337066869 ) ) ;
#14572 = EDGE_CURVE ( 'NONE', #2925, #32843, #11664, .T. ) ;
#14573 = AXIS2_PLACEMENT_3D ( 'NONE', #5714, #21729, #2001 ) ;
#14574 = DIRECTION ( 'NONE',  ( -0.000000000000000000, 1.000000000000000000, -0.000000000000000000 ) ) ;
#14575 = CYLINDRICAL_SURFACE ( 'NONE', #37499, 15.24495751795539000 ) ;
#14576 = EDGE_LOOP ( 'NONE', ( #43871, #44823, #14315, #13945 ) ) ;
#14577 = ORIENTED_EDGE ( 'NONE', *, *, #50340, .T. ) ;
#14578 = VERTEX_POINT ( 'NONE', #35567 ) ;
#14579 = LINE ( 'NONE', #23239, #18269 ) ;
#14580 = LINE ( 'NONE', #2489, #38621 ) ;
#14581 = EDGE_CURVE ( 'NONE', #22734, #23787, #19307, .T. ) ;
#14582 = DIRECTION ( 'NONE',  ( 0.1476465640024851034, 0.000000000000000000, -0.9890401873221634776 ) ) ;
#14583 = DIRECTION ( 'NONE',  ( 0.000000000000000000, 1.000000000000000000, 0.000000000000000000 ) ) ;
#14584 = ORIENTED_EDGE ( 'NONE', *, *, #41744, .T. ) ;
#14585 = EDGE_CURVE ( 'NONE', #29842, #3318, #7974, .T. ) ;
#14586 = DIRECTION ( 'NONE',  ( 0.000000000000000000, 0.000000000000000000, -1.000000000000000000 ) ) ;
#14587 = LINE ( 'NONE', #11665, #39106 ) ;
#14588 = VECTOR ( 'NONE', #15189, 1000.000000000000114 ) ;
#14589 = VERTEX_POINT ( 'NONE', #4047 ) ;
#14590 = VERTEX_POINT ( 'NONE', #43722 ) ;
#14591 = LINE ( 'NONE', #43206, #34223 ) ;
#14592 = ADVANCED_FACE ( 'NONE', ( #28456 ), #7723, .F. ) ;
#14593 = CARTESIAN_POINT ( 'NONE',  ( -332.3517673607765914, -86.34605966037949543, -45.90766452162698386 ) ) ;
#14594 = DIRECTION ( 'NONE',  ( 0.1182731709213660498, 0.000000000000000000, -0.9929810960135169173 ) ) ;
#14595 = FACE_OUTER_BOUND ( 'NONE', #5392, .T. ) ;
#14596 = VERTEX_POINT ( 'NONE', #3776 ) ;
#14597 = DIRECTION ( 'NONE',  ( -0.000000000000000000, 1.000000000000000000, 0.000000000000000000 ) ) ;
#14598 = AXIS2_PLACEMENT_3D ( 'NONE', #46066, #29742, #50514 ) ;
#14599 = ORIENTED_EDGE ( 'NONE', *, *, #30745, .T. ) ;
#14600 = CARTESIAN_POINT ( 'NONE',  ( 30.05499637021956971, -183.6283474603465606, -97.24912084693207248 ) ) ;
#14601 = PLANE ( 'NONE',  #19448 ) ;
#14602 = ORIENTED_EDGE ( 'NONE', *, *, #30115, .F. ) ;
#14603 = CARTESIAN_POINT ( 'NONE',  ( -94.78385179329475818, -183.6283474603465606, 115.0304316645283080 ) ) ;
#14604 = CARTESIAN_POINT ( 'NONE',  ( -332.3517673607765914, -123.5000000000000284, 0.000000000000000000 ) ) ;
#14605 = DIRECTION ( 'NONE',  ( 8.659560562354930393E-17, 0.7071067811865479058, -0.7071067811865472397 ) ) ;
#14606 = FACE_OUTER_BOUND ( 'NONE', #5364, .T. ) ;
#14607 = LINE ( 'NONE', #38761, #5989 ) ;
#14608 = ORIENTED_EDGE ( 'NONE', *, *, #20518, .F. ) ;
#14609 = LINE ( 'NONE', #51154, #47439 ) ;
#14610 = EDGE_LOOP ( 'NONE', ( #41634, #45156, #8301, #23020 ) ) ;
#14611 = VECTOR ( 'NONE', #47770, 1000.000000000000000 ) ;
#14612 = EDGE_CURVE ( 'NONE', #7467, #37183, #8019, .T. ) ;
#14613 = AXIS2_PLACEMENT_3D ( 'NONE', #31511, #12318, #8386 ) ;
#14614 = EDGE_CURVE ( 'NONE', #14148, #43465, #19799, .T. ) ;
#14615 = EDGE_LOOP ( 'NONE', ( #24632, #12311, #42686, #44929 ) ) ;
#14616 = DIRECTION ( 'NONE',  ( -0.9646355819083556327, 0.000000000000000000, -0.2635871660690782825 ) ) ;
#14617 = ORIENTED_EDGE ( 'NONE', *, *, #14898, .F. ) ;
#14618 = CIRCLE ( 'NONE', #43980, 125.0000000000000000 ) ;
#14619 = EDGE_CURVE ( 'NONE', #26773, #34920, #39266, .T. ) ;
#14620 = LINE ( 'NONE', #43240, #15107 ) ;
#14621 = ORIENTED_EDGE ( 'NONE', *, *, #28865, .F. ) ;
#14622 = FACE_OUTER_BOUND ( 'NONE', #16055, .T. ) ;
#14623 = CARTESIAN_POINT ( 'NONE',  ( -150.1390659022305840, -193.5000000000000000, 72.73415134496005408 ) ) ;
#14624 = ORIENTED_EDGE ( 'NONE', *, *, #19784, .T. ) ;
#14625 = CARTESIAN_POINT ( 'NONE',  ( -171.2727421180348415, -183.6283474603465606, 23.38221600314377113 ) ) ;
#14626 = EDGE_CURVE ( 'NONE', #24680, #40690, #31892, .T. ) ;
#14628 = VECTOR ( 'NONE', #4111, 1000.000000000000000 ) ;
#14627 = CARTESIAN_POINT ( 'NONE',  ( -59.16959496120701090, -193.5000000000000000, 123.5388265266452237 ) ) ;
#14629 = CARTESIAN_POINT ( 'NONE',  ( -48.47912675150885065, -189.7472609257535510, -0.9999999999999931166 ) ) ;
#14630 = VERTEX_POINT ( 'NONE', #24007 ) ;
#14631 = VERTEX_POINT ( 'NONE', #45302 ) ;
#14632 = ADVANCED_FACE ( 'NONE', ( #21364 ), #44503, .T. ) ;
#14633 = EDGE_CURVE ( 'NONE', #39640, #49743, #28971, .T. ) ;
#14634 = VERTEX_POINT ( 'NONE', #9029 ) ;
#14635 = LINE ( 'NONE', #12185, #41016 ) ;
#14636 = CARTESIAN_POINT ( 'NONE',  ( 75.17589904515342880, -193.5000000000000000, -18.28755301364250130 ) ) ;
#14637 = EDGE_CURVE ( 'NONE', #15465, #16147, #29249, .T. ) ;
#14638 = DIRECTION ( 'NONE',  ( 0.000000000000000000, 0.000000000000000000, -1.000000000000000000 ) ) ;
#14639 = DIRECTION ( 'NONE',  ( 0.000000000000000000, -0.2393156642875652051, -0.9709418174260502354 ) ) ;
#14640 = PLANE ( 'NONE',  #46520 ) ;
#14641 = ORIENTED_EDGE ( 'NONE', *, *, #31100, .F. ) ;
#14642 = DIRECTION ( 'NONE',  ( -0.000000000000000000, 1.000000000000000000, 0.000000000000000000 ) ) ;
#14643 = ORIENTED_EDGE ( 'NONE', *, *, #32441, .F. ) ;
#14645 = ORIENTED_EDGE ( 'NONE', *, *, #35188, .T. ) ;
#14644 = CYLINDRICAL_SURFACE ( 'NONE', #47445, 10.00000000000000000 ) ;
#14646 = EDGE_LOOP ( 'NONE', ( #7806, #7044, #46949, #21977 ) ) ;
#14647 = CARTESIAN_POINT ( 'NONE',  ( -339.1964088526558498, -96.52406086224443982, -52.47426709956138069 ) ) ;
#14648 = EDGE_LOOP ( 'NONE', ( #47360, #41721, #35106, #34538 ) ) ;
#14649 = CARTESIAN_POINT ( 'NONE',  ( -48.93575598890255662, -189.7472609257535510, -0.8896570909947461026 ) ) ;
#14650 = VECTOR ( 'NONE', #42816, 1000.000000000000000 ) ;
#14651 = DIRECTION ( 'NONE',  ( 0.000000000000000000, 1.000000000000000000, -0.000000000000000000 ) ) ;
#14652 = CARTESIAN_POINT ( 'NONE',  ( -48.47912675150885065, -173.5000000000000284, 125.0000000000000000 ) ) ;
#14653 = ORIENTED_EDGE ( 'NONE', *, *, #807, .T. ) ;
#14654 = DIRECTION ( 'NONE',  ( 0.000000000000000000, -1.000000000000000000, 0.000000000000000000 ) ) ;
#14655 = ORIENTED_EDGE ( 'NONE', *, *, #35582, .T. ) ;
#14656 = AXIS2_PLACEMENT_3D ( 'NONE', #6667, #18234, #42129 ) ;
#14657 = ORIENTED_EDGE ( 'NONE', *, *, #19979, .T. ) ;
#14658 = CARTESIAN_POINT ( 'NONE',  ( -130.7087404384255080, -175.3837268820161057, -94.14505102712755047 ) ) ;
#14659 = LINE ( 'NONE', #26738, #26409 ) ;
#14660 = FACE_OUTER_BOUND ( 'NONE', #31373, .T. ) ;
#14661 = LINE ( 'NONE', #20085, #49258 ) ;
#14662 = VERTEX_POINT ( 'NONE', #49751 ) ;
#14663 = LINE ( 'NONE', #34873, #45865 ) ;
#14664 = CARTESIAN_POINT ( 'NONE',  ( -161.2555905272864152, -189.7472609257535510, -53.91167979418494838 ) ) ;
#14665 = LINE ( 'NONE', #7041, #36398 ) ;
#14666 = DIRECTION ( 'NONE',  ( 0.000000000000000000, 0.5680647467311658039, 0.8229838658936494689 ) ) ;
#14667 = VERTEX_POINT ( 'NONE', #33187 ) ;
#14668 = AXIS2_PLACEMENT_3D ( 'NONE', #51609, #7968, #7720 ) ;
#14669 = DIRECTION ( 'NONE',  ( -0.000000000000000000, 1.000000000000000000, -0.000000000000000000 ) ) ;
#14670 = LINE ( 'NONE', #13898, #38260 ) ;
#14671 = DIRECTION ( 'NONE',  ( 0.000000000000000000, -1.000000000000000000, 0.000000000000000000 ) ) ;
#14672 = ORIENTED_EDGE ( 'NONE', *, *, #46778, .F. ) ;
#14673 = EDGE_CURVE ( 'NONE', #38136, #35121, #37388, .T. ) ;
#14674 = DIRECTION ( 'NONE',  ( 0.000000000000000000, 0.000000000000000000, -1.000000000000000000 ) ) ;
#14675 = EDGE_CURVE ( 'NONE', #28774, #17068, #1661, .T. ) ;
#14676 = ORIENTED_EDGE ( 'NONE', *, *, #26949, .F. ) ;
#14677 = EDGE_CURVE ( 'NONE', #48253, #43006, #21102, .T. ) ;
#14678 = PLANE ( 'NONE',  #41339 ) ;
#14679 = ORIENTED_EDGE ( 'NONE', *, *, #6762, .F. ) ;
#14680 = CARTESIAN_POINT ( 'NONE',  ( -47.53180039765465636, -193.5000000000000000, -0.3202698538628280800 ) ) ;
#14681 = AXIS2_PLACEMENT_3D ( 'NONE', #15182, #35141, #10968 ) ;
#14682 = PLANE ( 'NONE',  #23684 ) ;
#14683 = CARTESIAN_POINT ( 'NONE',  ( 40.30419662299490113, -177.1207230881787780, -87.99159897727903967 ) ) ;
#14684 = EDGE_CURVE ( 'NONE', #9853, #5202, #42422, .T. ) ;
#14685 = CIRCLE ( 'NONE', #11326, 125.0000000000000000 ) ;
#14686 = CARTESIAN_POINT ( 'NONE',  ( 75.60865171534661044, -183.6283474603465606, -15.07392567185467236 ) ) ;
#14687 = EDGE_CURVE ( 'NONE', #10667, #21060, #17447, .T. ) ;
#14688 = CARTESIAN_POINT ( 'NONE',  ( -330.4913330509368166, -71.49045607248250178, -27.86139516340898581 ) ) ;
#14689 = ORIENTED_EDGE ( 'NONE', *, *, #45842, .T. ) ;
#14690 = AXIS2_PLACEMENT_3D ( 'NONE', #15198, #35666, #19642 ) ;
#14691 = ADVANCED_FACE ( 'NONE', ( #20583 ), #49233, .T. ) ;
#14692 = DIRECTION ( 'NONE',  ( -1.000000000000000000, 1.258058860540606954E-15, 1.036104688092335102E-14 ) ) ;
#14693 = ORIENTED_EDGE ( 'NONE', *, *, #32654, .T. ) ;
#14694 = DIRECTION ( 'NONE',  ( 0.000000000000000000, 0.000000000000000000, 1.000000000000000000 ) ) ;
#14695 = EDGE_CURVE ( 'NONE', #16038, #37674, #12686, .T. ) ;
#14696 = ORIENTED_EDGE ( 'NONE', *, *, #30751, .F. ) ;
#14697 = AXIS2_PLACEMENT_3D ( 'NONE', #48316, #40161, #28584 ) ;
#14698 = DIRECTION ( 'NONE',  ( 1.000000000000000000, -0.000000000000000000, -0.000000000000000000 ) ) ;
#14699 = AXIS2_PLACEMENT_3D ( 'NONE', #38202, #13782, #37700 ) ;
#14700 = EDGE_CURVE ( 'NONE', #6669, #27166, #45550, .T. ) ;
#14701 = CIRCLE ( 'NONE', #1264, 125.0000000000000000 ) ;
#14702 = CIRCLE ( 'NONE', #41551, 125.0000000000000000 ) ;
#14703 = DIRECTION ( 'NONE',  ( -0.6965510290630033685, 0.000000000000000000, 0.7175072570443249420 ) ) ;
#14704 = PRODUCT_DEFINITION_SHAPE ( 'NONE', 'NONE',  #47283 ) ;
#14705 = CARTESIAN_POINT ( 'NONE',  ( -48.47912675150885065, -175.3837268820161057, 6.938893903907228378E-15 ) ) ;
#14706 = ORIENTED_EDGE ( 'NONE', *, *, #30628, .F. ) ;
#14709 = VERTEX_POINT ( 'NONE', #1120 ) ;
#14708 = CARTESIAN_POINT ( 'NONE',  ( -336.3521761649654422, -180.1556192733800117, 16.67542351306693149 ) ) ;
#14707 = DIRECTION ( 'NONE',  ( -0.3482016354343866471, 0.000000000000000000, -0.9374196611341253371 ) ) ;
#14710 = DIRECTION ( 'NONE',  ( -0.000000000000000000, 1.000000000000000000, 0.000000000000000000 ) ) ;
#14711 = ORIENTED_EDGE ( 'NONE', *, *, #9942, .T. ) ;
#14712 = CARTESIAN_POINT ( 'NONE',  ( -172.1341525481709880, -175.3837268820161057, 18.28755301364337527 ) ) ;
#14713 = VERTEX_POINT ( 'NONE', #41072 ) ;
#14714 = PLANE ( 'NONE',  #4922 ) ;
#14717 = ORIENTED_EDGE ( 'NONE', *, *, #32888, .T. ) ;
#14716 = PLANE ( 'NONE',  #50189 ) ;
#14715 = DIRECTION ( 'NONE',  ( 0.4300652022765245608, 0.000000000000000000, -0.9027978299657416494 ) ) ;
#14718 = ADVANCED_FACE ( 'NONE', ( #13483 ), #13742, .T. ) ;
#14719 = ORIENTED_EDGE ( 'NONE', *, *, #22775, .F. ) ;
#14720 = LINE ( 'NONE', #22339, #51733 ) ;
#14721 = ORIENTED_EDGE ( 'NONE', *, *, #48807, .F. ) ;
#14722 = DIRECTION ( 'NONE',  ( -0.9473263538541876194, 0.000000000000000000, -0.3202698538628486746 ) ) ;
#14723 = AXIS2_PLACEMENT_3D ( 'NONE', #46039, #50487, #19196 ) ;
#14724 = CARTESIAN_POINT ( 'NONE',  ( 46.01898237923984425, -183.6283474603465606, -81.82363577055903647 ) ) ;
#14725 = VERTEX_POINT ( 'NONE', #33467 ) ;
#14726 = CARTESIAN_POINT ( 'NONE',  ( -48.47912675150885065, -188.5000000000000284, -14.99999999999999289 ) ) ;
#14727 = DIRECTION ( 'NONE',  ( -0.000000000000000000, 0.000000000000000000, 1.000000000000000000 ) ) ;
#14728 = CARTESIAN_POINT ( 'NONE',  ( -332.3517673607765914, -123.5000000000000284, 0.000000000000000000 ) ) ;
#14729 = FACE_OUTER_BOUND ( 'NONE', #26441, .T. ) ;
#14730 = VECTOR ( 'NONE', #1124, 1000.000000000000000 ) ;
#14731 = DIRECTION ( 'NONE',  ( 0.000000000000000000, 0.000000000000000000, 1.000000000000000000 ) ) ;
#14732 = CIRCLE ( 'NONE', #39907, 125.0000000000000000 ) ;
#14733 = ORIENTED_EDGE ( 'NONE', *, *, #8570, .T. ) ;
#14734 = DIRECTION ( 'NONE',  ( 0.8757349421956412971, 0.000000000000000000, -0.4827922027307366970 ) ) ;
#14736 = AXIS2_PLACEMENT_3D ( 'NONE', #41421, #25408, #17537 ) ;
#14735 = LINE ( 'NONE', #26551, #34844 ) ;
#14737 = EDGE_CURVE ( 'NONE', #33172, #45478, #615, .T. ) ;
#14738 = CARTESIAN_POINT ( 'NONE',  ( -14.28570516517293676, -183.6283474603465606, 120.2323164553486663 ) ) ;
#14739 = ORIENTED_EDGE ( 'NONE', *, *, #32211, .T. ) ;
#14740 = DIRECTION ( 'NONE',  ( -1.000000000000000000, -0.000000000000000000, -0.000000000000000000 ) ) ;
#14741 = DIRECTION ( 'NONE',  ( -0.000000000000000000, 1.000000000000000000, -0.000000000000000000 ) ) ;
#14742 = AXIS2_PLACEMENT_3D ( 'NONE', #21758, #25436, #29889 ) ;
#14743 = ADVANCED_FACE ( 'NONE', ( #37124 ), #25558, .T. ) ;
#14744 = CARTESIAN_POINT ( 'NONE',  ( 33.09766481721658238, -189.7472609257535510, 93.38753978496653474 ) ) ;
#14745 = ADVANCED_FACE ( 'NONE', ( #28709 ), #8749, .T. ) ;
#14746 = CARTESIAN_POINT ( 'NONE',  ( -120.2975302769383177, -183.6283474603465606, 102.3089288139533863 ) ) ;
#14747 = EDGE_CURVE ( 'NONE', #29477, #12246, #869, .T. ) ;
#14748 = EDGE_CURVE ( 'NONE', #41150, #6819, #6887, .T. ) ;
#14749 = ORIENTED_EDGE ( 'NONE', *, *, #29495, .T. ) ;
#14750 = VECTOR ( 'NONE', #3642, 1000.000000000000000 ) ;
#14751 = EDGE_CURVE ( 'NONE', #47404, #34424, #46079, .T. ) ;
#14752 = AXIS2_PLACEMENT_3D ( 'NONE', #7477, #32149, #36350 ) ;
#14753 = DIRECTION ( 'NONE',  ( -0.000000000000000000, -0.9709418174260534551, -0.2393156642875516327 ) ) ;
#14754 = EDGE_CURVE ( 'NONE', #20769, #36975, #6128, .T. ) ;
#14755 = CARTESIAN_POINT ( 'NONE',  ( -48.47912675150885065, -175.3837268820161057, 6.938893903907228378E-15 ) ) ;
#14756 = DIRECTION ( 'NONE',  ( 0.000000000000000000, -1.000000000000000000, -0.000000000000000000 ) ) ;
#14757 = DIRECTION ( 'NONE',  ( 0.6068001458185945385, 0.000000000000000000, -0.7948544414133523750 ) ) ;
#14758 = EDGE_LOOP ( 'NONE', ( #48712, #49267, #49566, #15520 ) ) ;
#14759 = EDGE_CURVE ( 'NONE', #38746, #51182, #9801, .T. ) ;
#14760 = CARTESIAN_POINT ( 'NONE',  ( -138.3705904895685705, -177.1207230881787780, -86.85922373029296750 ) ) ;
#14761 = ADVANCED_FACE ( 'NONE', ( #46849 ), #27141, .T. ) ;
#14762 = CARTESIAN_POINT ( 'NONE',  ( -91.84482189527190599, -189.7472609257535510, -117.2365833888816553 ) ) ;
#14763 = VERTEX_POINT ( 'NONE', #10064 ) ;
#14764 = ORIENTED_EDGE ( 'NONE', *, *, #45781, .F. ) ;
#14765 = VECTOR ( 'NONE', #12588, 1000.000000000000000 ) ;
#14766 = EDGE_CURVE ( 'NONE', #45352, #22881, #25828, .T. ) ;
#14767 = VERTEX_POINT ( 'NONE', #2678 ) ;
#14768 = LINE ( 'NONE', #15275, #40975 ) ;
#14769 = AXIS2_PLACEMENT_3D ( 'NONE', #30805, #47359, #30287 ) ;
#14770 = AXIS2_PLACEMENT_3D ( 'NONE', #50805, #35522, #30823 ) ;
#14771 = EDGE_CURVE ( 'NONE', #23058, #32062, #40565, .T. ) ;
#14772 = CARTESIAN_POINT ( 'NONE',  ( 69.14211578623219623, -193.5000000000000000, 42.31126686685117733 ) ) ;
#14773 = LINE ( 'NONE', #28052, #27179 ) ;
#14774 = VERTEX_POINT ( 'NONE', #21892 ) ;
#14775 = EDGE_CURVE ( 'NONE', #11672, #9277, #1907, .T. ) ;
#14776 = DIRECTION ( 'NONE',  ( -8.718379230999707126E-17, -0.9709418174260493473, 0.2393156642875685913 ) ) ;
#14777 = DIRECTION ( 'NONE',  ( 0.000000000000000000, 0.000000000000000000, -1.000000000000000000 ) ) ;
#14780 = VERTEX_POINT ( 'NONE', #17950 ) ;
#14779 = FACE_OUTER_BOUND ( 'NONE', #11744, .T. ) ;
#14778 = DIRECTION ( 'NONE',  ( 0.000000000000000000, 0.000000000000000000, 1.000000000000000000 ) ) ;
#14781 = AXIS2_PLACEMENT_3D ( 'NONE', #26932, #2512, #42448 ) ;
#14782 = FACE_OUTER_BOUND ( 'NONE', #9944, .T. ) ;
#14783 = ORIENTED_EDGE ( 'NONE', *, *, #50050, .F. ) ;
#14784 = PLANE ( 'NONE',  #15514 ) ;
#14785 = VERTEX_POINT ( 'NONE', #22917 ) ;
#14786 = CARTESIAN_POINT ( 'NONE',  ( -32.87124591993210743, -175.3837268820161057, 124.0217483183788119 ) ) ;
#14787 = VECTOR ( 'NONE', #7910, 1000.000000000000000 ) ;
#14788 = CARTESIAN_POINT ( 'NONE',  ( -170.0000000000000284, -115.7896721143442278, 18.45401972188388839 ) ) ;
#14789 = EDGE_CURVE ( 'NONE', #3419, #45115, #18719, .T. ) ;
#14790 = EDGE_LOOP ( 'NONE', ( #11945, #2496, #39432, #44904 ) ) ;
#14791 = ADVANCED_FACE ( 'NONE', ( #29757 ), #51058, .T. ) ;
#14792 = VECTOR ( 'NONE', #47436, 1000.000000000000000 ) ;
#14793 = ORIENTED_EDGE ( 'NONE', *, *, #36819, .F. ) ;
#14794 = DIRECTION ( 'NONE',  ( -0.000000000000000000, 1.000000000000000000, -0.000000000000000000 ) ) ;
#14795 = DIRECTION ( 'NONE',  ( 1.000000000000000000, 0.000000000000000000, -0.000000000000000000 ) ) ;
#14796 = ORIENTED_EDGE ( 'NONE', *, *, #2542, .T. ) ;
#14797 = DIRECTION ( 'NONE',  ( 0.000000000000000000, 0.000000000000000000, 1.000000000000000000 ) ) ;
#14798 = DIRECTION ( 'NONE',  ( 0.9374196611341183427, 0.000000000000000000, 0.3482016354344059095 ) ) ;
#14799 = ORIENTED_EDGE ( 'NONE', *, *, #6101, .T. ) ;
#14800 = DIRECTION ( 'NONE',  ( -0.000000000000000000, 1.000000000000000000, -0.000000000000000000 ) ) ;
#14801 = CARTESIAN_POINT ( 'NONE',  ( -336.3521761649654422, -120.8677111499054320, 59.00000000000000000 ) ) ;
#14802 = ORIENTED_EDGE ( 'NONE', *, *, #31656, .T. ) ;
#14803 = CYLINDRICAL_SURFACE ( 'NONE', #50951, 4.999999999999997335 ) ;
#14804 = ORIENTED_EDGE ( 'NONE', *, *, #47522, .F. ) ;
#14805 = CIRCLE ( 'NONE', #50888, 125.0000000000000000 ) ;
#14806 = AXIS2_PLACEMENT_3D ( 'NONE', #8572, #4378, #40890 ) ;
#14807 = LINE ( 'NONE', #11097, #46621 ) ;
#14808 = CARTESIAN_POINT ( 'NONE',  ( -332.3517673607765914, -182.5000000000000568, 2.632288850093980503 ) ) ;
#14809 = ORIENTED_EDGE ( 'NONE', *, *, #30380, .F. ) ;
#14810 = CIRCLE ( 'NONE', #15627, 125.0000000000000000 ) ;
#14811 = AXIS2_PLACEMENT_3D ( 'NONE', #15512, #12594, #47837 ) ;
#14812 = EDGE_CURVE ( 'NONE', #22921, #15605, #46585, .T. ) ;
#14813 = CARTESIAN_POINT ( 'NONE',  ( -47.64924157374594671, -189.7472609257535510, 124.9972451320097377 ) ) ;
#14814 = DIRECTION ( 'NONE',  ( 0.000000000000000000, 3.491481338843133355E-15, 1.000000000000000000 ) ) ;
#14815 = CARTESIAN_POINT ( 'NONE',  ( -336.3521761649654422, -176.5004679656469477, -25.97334715265976612 ) ) ;
#14816 = EDGE_CURVE ( 'NONE', #27018, #1163, #6383, .T. ) ;
#14817 = ORIENTED_EDGE ( 'NONE', *, *, #34010, .F. ) ;
#14818 = DIRECTION ( 'NONE',  ( 0.9151456172430210145, 0.000000000000000000, -0.4031234292879665171 ) ) ;
#14819 = ADVANCED_FACE ( 'NONE', ( #30800 ), #10569, .F. ) ;
#14820 = VECTOR ( 'NONE', #30876, 1000.000000000000000 ) ;
#14821 = AXIS2_PLACEMENT_3D ( 'NONE', #49273, #13266, #9576 ) ;
#14822 = FACE_BOUND ( 'NONE', #35495, .T. ) ;
#14823 = DIRECTION ( 'NONE',  ( 0.000000000000000000, 0.000000000000000000, 1.000000000000000000 ) ) ;
#14825 = ORIENTED_EDGE ( 'NONE', *, *, #48392, .T. ) ;
#14824 = PLANE ( 'NONE',  #24485 ) ;
#14826 = AXIS2_PLACEMENT_3D ( 'NONE', #23074, #42520, #35664 ) ;
#14827 = CIRCLE ( 'NONE', #24903, 125.0000000000000000 ) ;
#14828 = ORIENTED_EDGE ( 'NONE', *, *, #47338, .F. ) ;
#14829 = DIRECTION ( 'NONE',  ( 0.000000000000000000, -1.000000000000000000, -0.000000000000000000 ) ) ;
#14830 = CIRCLE ( 'NONE', #2207, 125.0000000000000000 ) ;
#14831 = VECTOR ( 'NONE', #23185, 1000.000000000000000 ) ;
#14832 = DIRECTION ( 'NONE',  ( 0.000000000000000000, -0.7485107481711046340, -0.6631226582407911962 ) ) ;
#14833 = ORIENTED_EDGE ( 'NONE', *, *, #23580, .F. ) ;
#14834 = CARTESIAN_POINT ( 'NONE',  ( -330.4913330509368166, -123.5000000000000284, 0.000000000000000000 ) ) ;
#14835 = EDGE_CURVE ( 'NONE', #39207, #7752, #42106, .T. ) ;
#14836 = ORIENTED_EDGE ( 'NONE', *, *, #32944, .T. ) ;
#14837 = FACE_OUTER_BOUND ( 'NONE', #28437, .T. ) ;
#14838 = DIRECTION ( 'NONE',  ( 0.2635871660690581320, 0.000000000000000000, 0.9646355819083614058 ) ) ;
#14839 = FACE_OUTER_BOUND ( 'NONE', #38059, .T. ) ;
#14840 = DIRECTION ( 'NONE',  ( 0.000000000000000000, -0.9927088740980538617, 0.1205366802553232974 ) ) ;
#14841 = ORIENTED_EDGE ( 'NONE', *, *, #42916, .T. ) ;
#14842 = ORIENTED_EDGE ( 'NONE', *, *, #36257, .F. ) ;
#14843 = ADVANCED_FACE ( 'NONE', ( #2938 ), #50276, .T. ) ;
#14844 = ORIENTED_EDGE ( 'NONE', *, *, #27114, .F. ) ;
#14845 = DIRECTION ( 'NONE',  ( 0.000000000000000000, -1.000000000000000000, 0.000000000000000000 ) ) ;
#14846 = LINE ( 'NONE', #45863, #8419 ) ;
#14847 = AXIS2_PLACEMENT_3D ( 'NONE', #42844, #29527, #21916 ) ;
#14848 = DIRECTION ( 'NONE',  ( -0.000000000000000000, 0.8229838658936634577, 0.5680647467311457088 ) ) ;
#14849 = CIRCLE ( 'NONE', #33286, 125.0000000000000000 ) ;
#14850 = CARTESIAN_POINT ( 'NONE',  ( -48.47912675150885065, -183.6283474603465606, 6.938893903907228378E-15 ) ) ;
#14851 = DIRECTION ( 'NONE',  ( 0.7175072570443348230, 0.000000000000000000, -0.6965510290629933765 ) ) ;
#14852 = ORIENTED_EDGE ( 'NONE', *, *, #45633, .F. ) ;
#14853 = VECTOR ( 'NONE', #13693, 1000.000000000000000 ) ;
#14854 = UNCERTAINTY_MEASURE_WITH_UNIT (LENGTH_MEASURE( 1.000000000000000082E-05 ), #6843, 'distance_accuracy_value', 'NONE');
#14855 = DIRECTION ( 'NONE',  ( 0.000000000000000000, 1.000000000000000000, -0.000000000000000000 ) ) ;
#14856 = DIRECTION ( 'NONE',  ( -0.9785564922995060311, 0.000000000000000000, 0.2059786187410889424 ) ) ;
#14857 = ORIENTED_EDGE ( 'NONE', *, *, #16642, .T. ) ;
#14858 = ORIENTED_EDGE ( 'NONE', *, *, #34657, .T. ) ;
#14859 = AXIS2_PLACEMENT_3D ( 'NONE', #22417, #1670, #14536 ) ;
#14860 = CARTESIAN_POINT ( 'NONE',  ( 9.518239912201979180, -193.5000000000000000, 110.7307791902283043 ) ) ;
#14861 = CARTESIAN_POINT ( 'NONE',  ( -48.47912675150885065, -177.1207230881787780, 6.938893903907228378E-15 ) ) ;
#14862 = CARTESIAN_POINT ( 'NONE',  ( -111.6834028793037987, -189.7472609257535510, 106.6827995071088395 ) ) ;
#14863 = VECTOR ( 'NONE', #18921, 999.9999999999998863 ) ;
#14864 = DIRECTION ( 'NONE',  ( -1.000000000000000000, 0.000000000000000000, 0.000000000000000000 ) ) ;
#14865 = CIRCLE ( 'NONE', #24081, 125.0000000000000000 ) ;
#14866 = VECTOR ( 'NONE', #27897, 1000.000000000000000 ) ;
#14867 = CARTESIAN_POINT ( 'NONE',  ( -123.0610352593084116, -193.5000000000000000, 99.06333546307732263 ) ) ;
#14868 = CARTESIAN_POINT ( 'NONE',  ( -81.70897914701313880, -193.5000000000000000, -120.5021863277716534 ) ) ;
#14869 = ORIENTED_EDGE ( 'NONE', *, *, #19596, .F. ) ;
#14870 = CARTESIAN_POINT ( 'NONE',  ( -101.9736325116273434, -177.1207230881787780, 112.9749434763330669 ) ) ;
#14871 = AXIS2_PLACEMENT_3D ( 'NONE', #27211, #35620, #43247 ) ;
#14872 = VECTOR ( 'NONE', #39693, 1000.000000000000114 ) ;
#14873 = ORIENTED_EDGE ( 'NONE', *, *, #40757, .T. ) ;
#14874 = DIRECTION ( 'NONE',  ( 0.000000000000000000, 1.000000000000000000, 0.000000000000000000 ) ) ;
#14875 = DIRECTION ( 'NONE',  ( -0.000000000000000000, 1.000000000000000000, -0.000000000000000000 ) ) ;
#14876 = VERTEX_POINT ( 'NONE', #14266 ) ;
#14877 = FACE_OUTER_BOUND ( 'NONE', #15426, .T. ) ;
#14878 = DIRECTION ( 'NONE',  ( 0.000000000000000000, 0.000000000000000000, 1.000000000000000000 ) ) ;
#14879 = DIRECTION ( 'NONE',  ( 0.000000000000000000, 0.000000000000000000, 1.000000000000000000 ) ) ;
#14880 = EDGE_CURVE ( 'NONE', #4103, #7207, #10315, .T. ) ;
#14881 = DIRECTION ( 'NONE',  ( 0.000000000000000000, 0.000000000000000000, 1.000000000000000000 ) ) ;
#14882 = CYLINDRICAL_SURFACE ( 'NONE', #11857, 125.0000000000000000 ) ;
#14883 = ORIENTED_EDGE ( 'NONE', *, *, #10579, .T. ) ;
#14884 = AXIS2_PLACEMENT_3D ( 'NONE', #8817, #15694, #16462 ) ;
#14885 = VECTOR ( 'NONE', #35794, 1000.000000000000114 ) ;
#14886 = CARTESIAN_POINT ( 'NONE',  ( -14.28570516517293676, -183.6283474603465606, 120.2323164553486663 ) ) ;
#14888 = ORIENTED_EDGE ( 'NONE', *, *, #50706, .T. ) ;
#14887 = FACE_OUTER_BOUND ( 'NONE', #31505, .T. ) ;
#14889 = VECTOR ( 'NONE', #35124, 1000.000000000000000 ) ;
#14890 = ORIENTED_EDGE ( 'NONE', *, *, #36455, .F. ) ;
#14891 = DIRECTION ( 'NONE',  ( 0.000000000000000000, -0.000000000000000000, -1.000000000000000000 ) ) ;
#14892 = ORIENTED_EDGE ( 'NONE', *, *, #36509, .T. ) ;
#14893 = AXIS2_PLACEMENT_3D ( 'NONE', #50068, #38215, #42156 ) ;
#14894 = ORIENTED_EDGE ( 'NONE', *, *, #11113, .F. ) ;
#14895 = LINE ( 'NONE', #51411, #39361 ) ;
#14896 = VECTOR ( 'NONE', #38923, 1000.000000000000227 ) ;
#14897 = LINE ( 'NONE', #46683, #48957 ) ;
#14898 = EDGE_CURVE ( 'NONE', #4373, #43725, #2438, .T. ) ;
#14899 = ORIENTED_EDGE ( 'NONE', *, *, #33687, .F. ) ;
#14900 = LINE ( 'NONE', #27731, #49292 ) ;
#14901 = CIRCLE ( 'NONE', #20774, 125.0000000000000000 ) ;
#14902 = LINE ( 'NONE', #11710, #9322 ) ;
#14903 = DIRECTION ( 'NONE',  ( -0.4566292373937077542, 0.000000000000000000, -0.8896570909947499883 ) ) ;
#14904 = ORIENTED_EDGE ( 'NONE', *, *, #10665, .F. ) ;
#14905 = VERTEX_POINT ( 'NONE', #7656 ) ;
#14906 = EDGE_LOOP ( 'NONE', ( #38296, #21244, #47965, #29362 ) ) ;
#14907 = CIRCLE ( 'NONE', #24130, 125.0000000000000000 ) ;
#14908 = DIRECTION ( 'NONE',  ( -0.9785564922995060311, 0.000000000000000000, 0.2059786187410889424 ) ) ;
#14909 = PLANE ( 'NONE',  #9232 ) ;
#14910 = EDGE_CURVE ( 'NONE', #20906, #23116, #8697, .T. ) ;
#14911 = FACE_OUTER_BOUND ( 'NONE', #41488, .T. ) ;
#14912 = DIRECTION ( 'NONE',  ( 0.000000000000000000, 0.000000000000000000, -1.000000000000000000 ) ) ;
#14913 = EDGE_LOOP ( 'NONE', ( #13233, #17200, #42750, #17758 ) ) ;
#14914 = EDGE_CURVE ( 'NONE', #30320, #48811, #31051, .T. ) ;
#14915 = FACE_OUTER_BOUND ( 'NONE', #33317, .T. ) ;
#14916 = VERTEX_POINT ( 'NONE', #32084 ) ;
#14918 = ORIENTED_EDGE ( 'NONE', *, *, #3052, .F. ) ;
#14917 = DIRECTION ( 'NONE',  ( 0.000000000000000000, 0.000000000000000000, -1.000000000000000000 ) ) ;
#14919 = AXIS2_PLACEMENT_3D ( 'NONE', #7484, #32155, #24015 ) ;
#14920 = ORIENTED_EDGE ( 'NONE', *, *, #22815, .F. ) ;
#14921 = CIRCLE ( 'NONE', #44282, 125.0000000000000000 ) ;
#14922 = DIRECTION ( 'NONE',  ( 0.000000000000000000, 0.000000000000000000, -1.000000000000000000 ) ) ;
#14923 = CARTESIAN_POINT ( 'NONE',  ( -49.21696003055057389, -189.7472609257535510, -0.6749830015182127774 ) ) ;
#14924 = AXIS2_PLACEMENT_3D ( 'NONE', #29548, #45347, #49550 ) ;
#14925 = CARTESIAN_POINT ( 'NONE',  ( 46.00000000000000711, -42.50000000000000000, -51.00000000000000000 ) ) ;
#14926 = PLANE ( 'NONE',  #30940 ) ;
#14927 = ORIENTED_EDGE ( 'NONE', *, *, #24844, .T. ) ;
#14928 = CARTESIAN_POINT ( 'NONE',  ( -332.3517673607765914, -69.20050475944881896, 25.52576769896171882 ) ) ;
#14929 = ORIENTED_EDGE ( 'NONE', *, *, #32846, .F. ) ;
#14930 = EDGE_CURVE ( 'NONE', #51182, #40259, #3210, .T. ) ;
#14931 = VERTEX_POINT ( 'NONE', #27874 ) ;
#14932 = DIRECTION ( 'NONE',  ( -0.000000000000000000, 1.000000000000000000, -0.000000000000000000 ) ) ;
#14933 = AXIS2_PLACEMENT_3D ( 'NONE', #29547, #25110, #17493 ) ;
#14934 = LINE ( 'NONE', #3344, #48257 ) ;
#14935 = LINE ( 'NONE', #46989, #42324 ) ;
#14936 = DIRECTION ( 'NONE',  ( 0.05924062789370748011, 0.000000000000000000, 0.9982437317643217956 ) ) ;
#14937 = ORIENTED_EDGE ( 'NONE', *, *, #37810, .F. ) ;
#14938 = AXIS2_PLACEMENT_3D ( 'NONE', #37920, #26346, #41336 ) ;
#14939 = CARTESIAN_POINT ( 'NONE',  ( -330.4913330509368166, -68.51134412508150717, 21.38919645685156112 ) ) ;
#14940 = DIRECTION ( 'NONE',  ( -0.000000000000000000, 1.000000000000000000, -0.000000000000000000 ) ) ;
#14941 = LINE ( 'NONE', #30948, #27997 ) ;
#14942 = CARTESIAN_POINT ( 'NONE',  ( 66.42899531795131907, -183.6283474603465606, 49.20491319441622124 ) ) ;
#14943 = EDGE_CURVE ( 'NONE', #26571, #46931, #7145, .T. ) ;
#14944 = EDGE_LOOP ( 'NONE', ( #12065, #39313, #4981, #9305 ) ) ;
#14945 = LINE ( 'NONE', #30951, #18774 ) ;
#14946 = FACE_OUTER_BOUND ( 'NONE', #50626, .T. ) ;
#14947 = ADVANCED_FACE ( 'NONE', ( #31307 ), #43413, .F. ) ;
#14948 = VECTOR ( 'NONE', #8963, 1000.000000000000114 ) ;
#14949 = CARTESIAN_POINT ( 'NONE',  ( -332.3517673607765914, -69.26746417191145611, -23.38292116578723068 ) ) ;
#14950 = ORIENTED_EDGE ( 'NONE', *, *, #6179, .T. ) ;
#14951 = EDGE_CURVE ( 'NONE', #51603, #35121, #32, .T. ) ;
#14952 = CARTESIAN_POINT ( 'NONE',  ( -339.1964088526558498, -176.3931552210898985, 28.32515014536894071 ) ) ;
#14953 = FACE_OUTER_BOUND ( 'NONE', #33183, .T. ) ;
#14954 = VERTEX_POINT ( 'NONE', #35251 ) ;
#14955 = CARTESIAN_POINT ( 'NONE',  ( 12.99855592850622799, -177.1207230881787780, 108.8370090194295017 ) ) ;
#14956 = VERTEX_POINT ( 'NONE', #16073 ) ;
#14957 = CYLINDRICAL_SURFACE ( 'NONE', #17583, 125.0000000000000000 ) ;
#14958 = VECTOR ( 'NONE', #27758, 1000.000000000000227 ) ;
#14959 = FACE_BOUND ( 'NONE', #42946, .T. ) ;
#14960 = CARTESIAN_POINT ( 'NONE',  ( -112.7586829773731267, -193.5000000000000000, -107.2060569716373379 ) ) ;
#14961 = EDGE_CURVE ( 'NONE', #11472, #19701, #47353, .T. ) ;
#14962 = EDGE_CURVE ( 'NONE', #18957, #5084, #40223, .T. ) ;
#14963 = CIRCLE ( 'NONE', #8225, 124.9999999999999858 ) ;
#14964 = LINE ( 'NONE', #19920, #26044 ) ;
#14965 = VERTEX_POINT ( 'NONE', #19734 ) ;
#14966 = VERTEX_POINT ( 'NONE', #11847 ) ;
#14967 = CARTESIAN_POINT ( 'NONE',  ( 18.49541618049843095, -193.5000000000000000, 105.5434062319798159 ) ) ;
#14968 = AXIS2_PLACEMENT_3D ( 'NONE', #15866, #17101, #23984 ) ;
#14969 = EDGE_LOOP ( 'NONE', ( #41707, #49761, #31013, #46734 ) ) ;
#14970 = LINE ( 'NONE', #38079, #3282 ) ;
#14971 = VECTOR ( 'NONE', #20989, 1000.000000000000114 ) ;
#14972 = LINE ( 'NONE', #2863, #32605 ) ;
#14973 = LINE ( 'NONE', #7836, #7977 ) ;
#14974 = ORIENTED_EDGE ( 'NONE', *, *, #10007, .T. ) ;
#14977 = VERTEX_POINT ( 'NONE', #39446 ) ;
#14976 = LINE ( 'NONE', #46510, #9667 ) ;
#14975 = LINE ( 'NONE', #22843, #10728 ) ;
#14978 = DIRECTION ( 'NONE',  ( -0.000000000000000000, 1.000000000000000000, -0.000000000000000000 ) ) ;
#14979 = ORIENTED_EDGE ( 'NONE', *, *, #46567, .T. ) ;
#14980 = DIRECTION ( 'NONE',  ( -0.2348860457809911206, 0.000000000000000000, 0.9720229140804089729 ) ) ;
#14981 = ORIENTED_EDGE ( 'NONE', *, *, #50403, .T. ) ;
#14982 = ADVANCED_FACE ( 'NONE', ( #19479 ), #47622, .F. ) ;
#14983 = EDGE_CURVE ( 'NONE', #48057, #36746, #48124, .T. ) ;
#14984 = DIRECTION ( 'NONE',  ( -0.000000000000000000, 0.9350162426854194964, 0.3546048870425235200 ) ) ;
#14985 = ORIENTED_EDGE ( 'NONE', *, *, #1586, .T. ) ;
#14988 = ORIENTED_EDGE ( 'NONE', *, *, #50363, .F. ) ;
#14987 = DIRECTION ( 'NONE',  ( -1.000000000000000000, 0.000000000000000000, 0.000000000000000000 ) ) ;
#14986 = DIRECTION ( 'NONE',  ( -0.9027978299657416494, 0.000000000000000000, -0.4300652022765245608 ) ) ;
#14989 = ORIENTED_EDGE ( 'NONE', *, *, #43929, .F. ) ;
#14990 = DIRECTION ( 'NONE',  ( 0.000000000000000000, 0.000000000000000000, 1.000000000000000000 ) ) ;
#14991 = EDGE_LOOP ( 'NONE', ( #565, #14460, #50902, #13323 ) ) ;
#14992 = DIRECTION ( 'NONE',  ( 0.000000000000000000, 0.000000000000000000, -1.000000000000000000 ) ) ;
#14993 = VECTOR ( 'NONE', #50288, 1000.000000000000227 ) ;
#14994 = DIRECTION ( 'NONE',  ( 0.000000000000000000, 0.000000000000000000, 1.000000000000000000 ) ) ;
#14995 = VERTEX_POINT ( 'NONE', #47875 ) ;
#14996 = COLOUR_RGB ( '', 0.31764706, 0.68627451, 0.89019608) ;
#14997 = CARTESIAN_POINT ( 'NONE',  ( 4.558749771216698221, -193.5000000000000000, -112.0852863853379233 ) ) ;
#14998 = DIRECTION ( 'NONE',  ( 0.000000000000000000, -3.469446951953614189E-15, 1.000000000000000000 ) ) ;
#14999 = CARTESIAN_POINT ( 'NONE',  ( -34.51936650669028239, -189.7472609257535510, -124.2180546213278092 ) ) ;
#15000 = AXIS2_PLACEMENT_3D ( 'NONE', #13661, #32847, #13148 ) ;
#15001 = FACE_OUTER_BOUND ( 'NONE', #33878, .T. ) ;
#15002 = ORIENTED_EDGE ( 'NONE', *, *, #21951, .F. ) ;
#15003 = EDGE_CURVE ( 'NONE', #8786, #34048, #15551, .T. ) ;
#15004 = CARTESIAN_POINT ( 'NONE',  ( -330.4913330509368166, -143.9541802141664562, 55.34326076196094135 ) ) ;
#15005 = DIRECTION ( 'NONE',  ( -1.000000000000000000, -0.000000000000000000, 0.000000000000000000 ) ) ;
#15006 = EDGE_CURVE ( 'NONE', #49077, #77, #12097, .T. ) ;
#15007 = DIRECTION ( 'NONE',  ( 0.000000000000000000, 0.000000000000000000, -1.000000000000000000 ) ) ;
#15008 = ORIENTED_EDGE ( 'NONE', *, *, #10535, .T. ) ;
#15009 = VECTOR ( 'NONE', #2547, 1000.000000000000000 ) ;
#15010 = ADVANCED_FACE ( 'NONE', ( #11074 ), #44181, .T. ) ;
#15011 = DIRECTION ( 'NONE',  ( 0.3482016354343995812, 0.000000000000000000, -0.9374196611341205632 ) ) ;
#15012 = DIRECTION ( 'NONE',  ( 0.000000000000000000, -1.000000000000000000, 0.000000000000000000 ) ) ;
#15013 = DIRECTION ( 'NONE',  ( 0.000000000000000000, -0.000000000000000000, 1.000000000000000000 ) ) ;
#15014 = ADVANCED_FACE ( 'NONE', ( #8179 ), #27100, .F. ) ;
#15015 = CARTESIAN_POINT ( 'NONE',  ( -95.37971604807249548, -193.5000000000000000, -114.7887733785763942 ) ) ;
#15016 = CARTESIAN_POINT ( 'NONE',  ( -49.45768324380835423, -189.7472609257535510, -0.2059786187411025149 ) ) ;
#15017 = ORIENTED_EDGE ( 'NONE', *, *, #4969, .F. ) ;
#15018 = AXIS2_PLACEMENT_3D ( 'NONE', #49625, #13879, #41734 ) ;
#15019 = LINE ( 'NONE', #3177, #43840 ) ;
#15020 = DIRECTION ( 'NONE',  ( 0.000000000000000000, 0.9927088740980544168, 0.1205366802553199251 ) ) ;
#15021 = CARTESIAN_POINT ( 'NONE',  ( -70.24606818074167336, -189.7472609257535510, -122.0745693923549169 ) ) ;
#15022 = PLANE ( 'NONE',  #14493 ) ;
#15023 = ORIENTED_EDGE ( 'NONE', *, *, #35582, .F. ) ;
#15024 = CARTESIAN_POINT ( 'NONE',  ( -147.0463339291295881, -183.6283474603465606, 76.87330921200150158 ) ) ;
#15025 = CARTESIAN_POINT ( 'NONE',  ( 75.27070168362158142, -189.7472609257535510, 17.63462396184792169 ) ) ;
#15026 = VERTEX_POINT ( 'NONE', #39958 ) ;
#15027 = CIRCLE ( 'NONE', #35154, 125.0000000000000000 ) ;
#15028 = ORIENTED_EDGE ( 'NONE', *, *, #42462, .F. ) ;
#15029 = CIRCLE ( 'NONE', #39352, 125.0000000000000000 ) ;
#15030 = ORIENTED_EDGE ( 'NONE', *, *, #41015, .F. ) ;
#15031 = DIRECTION ( 'NONE',  ( 0.000000000000000000, 0.9927088740980539727, -0.1205366802553233252 ) ) ;
#15032 = VECTOR ( 'NONE', #51227, 1000.000000000000000 ) ;
#15033 = CYLINDRICAL_SURFACE ( 'NONE', #938, 125.0000000000000000 ) ;
#15034 = ORIENTED_EDGE ( 'NONE', *, *, #15874, .F. ) ;
#15035 = ADVANCED_FACE ( 'NONE', ( #3981 ), #15050, .T. ) ;
#15036 = CARTESIAN_POINT ( 'NONE',  ( 69.72248760683812918, -193.5000000000000000, -37.47770156625421833 ) ) ;
#15037 = DIRECTION ( 'NONE',  ( 0.000000000000000000, 0.000000000000000000, 1.000000000000000000 ) ) ;
#15038 = VECTOR ( 'NONE', #43514, 1000.000000000000000 ) ;
#15041 = ORIENTED_EDGE ( 'NONE', *, *, #41504, .T. ) ;
#15040 = DIRECTION ( 'NONE',  ( 1.043714542225393381E-14, -0.5680647467311510379, 0.8229838658936596829 ) ) ;
#15039 = CARTESIAN_POINT ( 'NONE',  ( 22.03849146056077757, -193.5000000000000000, 103.2098131075567409 ) ) ;
#15042 = DIRECTION ( 'NONE',  ( 0.3202698538628279690, 0.000000000000000000, 0.9473263538541946138 ) ) ;
#15043 = EDGE_LOOP ( 'NONE', ( #44176, #1504, #46345, #41766 ) ) ;
#15044 = LINE ( 'NONE', #47350, #32258 ) ;
#15045 = ORIENTED_EDGE ( 'NONE', *, *, #6179, .F. ) ;
#15046 = EDGE_CURVE ( 'NONE', #27857, #29243, #44324, .T. ) ;
#15047 = ADVANCED_FACE ( 'NONE', ( #1465 ), #41649, .T. ) ;
#15048 = EDGE_CURVE ( 'NONE', #8272, #3435, #48532, .T. ) ;
#15049 = DIRECTION ( 'NONE',  ( 1.000000000000000000, 0.000000000000000000, -0.000000000000000000 ) ) ;
#15050 = PLANE ( 'NONE',  #46445 ) ;
#15052 = FACE_OUTER_BOUND ( 'NONE', #11727, .T. ) ;
#15051 = CARTESIAN_POINT ( 'NONE',  ( -336.3521761649654422, -70.03480886230919111, 25.08789112700620194 ) ) ;
#15053 = ORIENTED_EDGE ( 'NONE', *, *, #28852, .T. ) ;
#15054 = ADVANCED_FACE ( 'NONE', ( #4620 ), #45364, .T. ) ;
#15055 = CONICAL_SURFACE ( 'NONE', #29322, 4.042878180043863345, 0.07858164904571392217 ) ;
#15056 = ORIENTED_EDGE ( 'NONE', *, *, #51545, .F. ) ;
#15057 = DIRECTION ( 'NONE',  ( -0.000000000000000000, 1.000000000000000000, 0.000000000000000000 ) ) ;
#15058 = PLANE ( 'NONE',  #50220 ) ;
#15059 = ORIENTED_EDGE ( 'NONE', *, *, #38092, .F. ) ;
#15060 = ADVANCED_FACE ( 'NONE', ( #37454 ), #686, .F. ) ;
#15061 = DIRECTION ( 'NONE',  ( 0.9993203489176063492, 0.000000000000000000, 0.03686245026030503941 ) ) ;
#15062 = CARTESIAN_POINT ( 'NONE',  ( -332.3517673607765914, -90.77207769297352513, -50.28800156563430335 ) ) ;
#15063 = VERTEX_POINT ( 'NONE', #13993 ) ;
#15064 = CARTESIAN_POINT ( 'NONE',  ( 29.27398957514435196, -177.1207230881787780, -97.87467957287998388 ) ) ;
#15065 = EDGE_CURVE ( 'NONE', #38645, #19776, #12018, .T. ) ;
#15066 = PLANE ( 'NONE',  #28989 ) ;
#15067 = ADVANCED_FACE ( 'NONE', ( #13471 ), #17932, .T. ) ;
#15068 = ORIENTED_EDGE ( 'NONE', *, *, #36892, .T. ) ;
#15069 = CARTESIAN_POINT ( 'NONE',  ( -336.3521761649654422, -123.5000000000000284, 0.000000000000000000 ) ) ;
#15070 = ORIENTED_EDGE ( 'NONE', *, *, #25178, .T. ) ;
#15071 = EDGE_CURVE ( 'NONE', #23360, #20728, #49996, .T. ) ;
#15072 = VECTOR ( 'NONE', #28369, 1000.000000000000000 ) ;
#15073 = DIRECTION ( 'NONE',  ( -0.000000000000000000, 1.000000000000000000, 0.000000000000000000 ) ) ;
#15074 = CARTESIAN_POINT ( 'NONE',  ( -48.47912675150885065, -189.7472609257535510, 6.938893903907228378E-15 ) ) ;
#15075 = ORIENTED_EDGE ( 'NONE', *, *, #23636, .F. ) ;
#15076 = VECTOR ( 'NONE', #34845, 1000.000000000000000 ) ;
#15077 = EDGE_CURVE ( 'NONE', #29008, #34513, #30520, .T. ) ;
#15078 = DIRECTION ( 'NONE',  ( -0.000000000000000000, -0.000000000000000000, 1.000000000000000000 ) ) ;
#15079 = CARTESIAN_POINT ( 'NONE',  ( -48.47912675150885065, -177.1207230881787780, 6.938893903907228378E-15 ) ) ;
#15080 = CARTESIAN_POINT ( 'NONE',  ( -106.2948367055610106, -175.3837268820161057, -110.8257356506552185 ) ) ;
#15081 = ADVANCED_FACE ( 'NONE', ( #34467 ), #37897, .T. ) ;
#15082 = ORIENTED_EDGE ( 'NONE', *, *, #31394, .F. ) ;
#15083 = DIRECTION ( 'NONE',  ( 1.000000000000000000, 0.000000000000000000, 5.782411586589357392E-17 ) ) ;
#15084 = CARTESIAN_POINT ( 'NONE',  ( -88.23625491228470707, -183.6283474603465606, 118.5089480183148254 ) ) ;
#15085 = CARTESIAN_POINT ( 'NONE',  ( 60.00000000000001421, -93.32050807568917605, 51.65063509461090518 ) ) ;
#15087 = VERTEX_POINT ( 'NONE', #6630 ) ;
#15086 = FACE_OUTER_BOUND ( 'NONE', #21712, .T. ) ;
#15088 = ORIENTED_EDGE ( 'NONE', *, *, #19258, .F. ) ;
#15089 = DIRECTION ( 'NONE',  ( -0.000000000000000000, 1.000000000000000000, -0.000000000000000000 ) ) ;
#15090 = EDGE_CURVE ( 'NONE', #47251, #18925, #13727, .T. ) ;
#15091 = AXIS2_PLACEMENT_3D ( 'NONE', #48772, #5670, #25118 ) ;
#15092 = CARTESIAN_POINT ( 'NONE',  ( -336.3521761649654422, -72.48138011061176655, -29.74944317415788930 ) ) ;
#15093 = ORIENTED_EDGE ( 'NONE', *, *, #29796, .T. ) ;
#15094 = ORIENTED_EDGE ( 'NONE', *, *, #6452, .T. ) ;
#15095 = DIRECTION ( 'NONE',  ( 0.000000000000000000, 0.2393156642875516604, -0.9709418174260535661 ) ) ;
#15096 = VERTEX_POINT ( 'NONE', #21880 ) ;
#15097 = LINE ( 'NONE', #22965, #29166 ) ;
#15098 = CARTESIAN_POINT ( 'NONE',  ( -47.74129347246713451, -175.3837268820161057, 0.6749830015182212151 ) ) ;
#15099 = LINE ( 'NONE', #27412, #14373 ) ;
#15100 = PLANE ( 'NONE',  #2288 ) ;
#15101 = ORIENTED_EDGE ( 'NONE', *, *, #50777, .T. ) ;
#15102 = VERTEX_POINT ( 'NONE', #26581 ) ;
#15103 = EDGE_LOOP ( 'NONE', ( #26753, #23251, #25623, #11752 ) ) ;
#15104 = DIRECTION ( 'NONE',  ( 0.000000000000000000, -0.000000000000000000, -1.000000000000000000 ) ) ;
#15105 = CARTESIAN_POINT ( 'NONE',  ( -339.1964088526558498, -162.2499814621216672, -44.49369547121515467 ) ) ;
#15106 = CARTESIAN_POINT ( 'NONE',  ( -139.8555433305420195, -189.7472609257535510, -83.82333043185244037 ) ) ;
#15107 = VECTOR ( 'NONE', #6488, 1000.000000000000000 ) ;
#15108 = FACE_OUTER_BOUND ( 'NONE', #13326, .T. ) ;
#15109 = CARTESIAN_POINT ( 'NONE',  ( -48.64924157374594671, -175.3837268820161057, 124.9998842437354227 ) ) ;
#15110 = VERTEX_POINT ( 'NONE', #6364 ) ;
#15111 = EDGE_CURVE ( 'NONE', #50966, #48020, #25815, .T. ) ;
#15112 = ADVANCED_FACE ( 'NONE', ( #29482 ), #10051, .T. ) ;
#15113 = CARTESIAN_POINT ( 'NONE',  ( -172.0602536473422504, -175.3837268820161057, -10.18383939837523222 ) ) ;
#15114 = EDGE_CURVE ( 'NONE', #1772, #9394, #17148, .T. ) ;
#15115 = EDGE_CURVE ( 'NONE', #29336, #4180, #1895, .T. ) ;
#15116 = ORIENTED_EDGE ( 'NONE', *, *, #35151, .F. ) ;
#15117 = ORIENTED_EDGE ( 'NONE', *, *, #42906, .F. ) ;
#15118 = PLANE ( 'NONE',  #29789 ) ;
#15119 = CARTESIAN_POINT ( 'NONE',  ( -339.1964088526558498, -182.0095552316576573, -7.608018572112655420 ) ) ;
#15120 = CARTESIAN_POINT ( 'NONE',  ( -336.3521761649654422, -181.8730728925770563, 8.732051761644092025 ) ) ;
#15121 = CYLINDRICAL_SURFACE ( 'NONE', #37127, 10.99999999999999645 ) ;
#15122 = DIRECTION ( 'NONE',  ( -0.5085311186492094127, 0.000000000000000000, -0.8610436117673619938 ) ) ;
#15123 = ORIENTED_EDGE ( 'NONE', *, *, #21867, .T. ) ;
#15124 = DIRECTION ( 'NONE',  ( -0.5829794791144703447, 0.000000000000000000, -0.8124868780056825335 ) ) ;
#15125 = AXIS2_PLACEMENT_3D ( 'NONE', #16124, #39747, #35307 ) ;
#15126 = VECTOR ( 'NONE', #28237, 1000.000000000000000 ) ;
#15127 = ORIENTED_EDGE ( 'NONE', *, *, #42830, .F. ) ;
#15128 = LINE ( 'NONE', #3288, #44777 ) ;
#15129 = EDGE_CURVE ( 'NONE', #10851, #7810, #38918, .T. ) ;
#15130 = DIRECTION ( 'NONE',  ( -0.000000000000000000, 0.9350162426854194964, 0.3546048870425235200 ) ) ;
#15131 = EDGE_LOOP ( 'NONE', ( #2356, #50233, #23599, #1664 ) ) ;
#15132 = FACE_OUTER_BOUND ( 'NONE', #439, .T. ) ;
#15133 = DIRECTION ( 'NONE',  ( 0.000000000000000000, -1.000000000000000000, 0.000000000000000000 ) ) ;
#15134 = DIRECTION ( 'NONE',  ( -0.000000000000000000, 1.000000000000000000, -0.000000000000000000 ) ) ;
#15135 = DIRECTION ( 'NONE',  ( -0.000000000000000000, 1.000000000000000000, -0.000000000000000000 ) ) ;
#15136 = EDGE_CURVE ( 'NONE', #51892, #40491, #38139, .T. ) ;
#15137 = DIRECTION ( 'NONE',  ( 0.9266896074318370369, 0.000000000000000000, -0.3758275821142292306 ) ) ;
#15138 = ORIENTED_EDGE ( 'NONE', *, *, #32885, .F. ) ;
#15139 = CIRCLE ( 'NONE', #26002, 125.0000000000000000 ) ;
#15140 = CARTESIAN_POINT ( 'NONE',  ( -173.3294908491238004, -193.5000000000000000, -6.114457023560960991 ) ) ;
#15142 = ORIENTED_EDGE ( 'NONE', *, *, #32240, .F. ) ;
#15141 = CARTESIAN_POINT ( 'NONE',  ( -21.64528618042744412, -193.5000000000000000, 121.0625654437174745 ) ) ;
#15143 = ORIENTED_EDGE ( 'NONE', *, *, #31598, .F. ) ;
#15144 = DIRECTION ( 'NONE',  ( 1.000000000000000000, -3.091579882402700648E-17, -8.151826190875878101E-17 ) ) ;
#15145 = EDGE_LOOP ( 'NONE', ( #15150, #31653, #12385, #21538 ) ) ;
#15146 = DIRECTION ( 'NONE',  ( -0.000000000000000000, 1.000000000000000000, -0.000000000000000000 ) ) ;
#15147 = ORIENTED_EDGE ( 'NONE', *, *, #20275, .F. ) ;
#15148 = LINE ( 'NONE', #23018, #15038 ) ;
#15149 = DIRECTION ( 'NONE',  ( -0.000000000000000000, 0.3546048870425331789, -0.9350162426854158326 ) ) ;
#15150 = ORIENTED_EDGE ( 'NONE', *, *, #39785, .T. ) ;
#15151 = DIRECTION ( 'NONE',  ( -0.000000000000000000, -1.000000000000000000, -0.000000000000000000 ) ) ;
#15152 = CARTESIAN_POINT ( 'NONE',  ( -72.96029774493611342, -183.6283474603465606, 122.5792489240759409 ) ) ;
#15153 = DIRECTION ( 'NONE',  ( -0.1182731709213592358, 0.000000000000000000, -0.9929810960135178055 ) ) ;
#15154 = VERTEX_POINT ( 'NONE', #33696 ) ;
#15155 = ORIENTED_EDGE ( 'NONE', *, *, #20543, .T. ) ;
#15156 = VECTOR ( 'NONE', #28513, 1000.000000000000000 ) ;
#15158 = ORIENTED_EDGE ( 'NONE', *, *, #38795, .T. ) ;
#15157 = VECTOR ( 'NONE', #833, 1000.000000000000227 ) ;
#15159 = DIRECTION ( 'NONE',  ( -0.000000000000000000, -0.3546048870425267951, 0.9350162426854181641 ) ) ;
#15160 = FACE_OUTER_BOUND ( 'NONE', #27739, .T. ) ;
#15161 = CARTESIAN_POINT ( 'NONE',  ( -85.77912150413021664, -189.7472609257535510, -119.3051146910911768 ) ) ;
#15162 = CARTESIAN_POINT ( 'NONE',  ( -49.25565061422688728, -193.5000000000000000, -0.6300878435817132139 ) ) ;
#15163 = FACE_OUTER_BOUND ( 'NONE', #9168, .T. ) ;
#15164 = EDGE_LOOP ( 'NONE', ( #42701, #20685, #18225, #29202 ) ) ;
#15165 = ADVANCED_FACE ( 'NONE', ( #9526 ), #2424, .T. ) ;
#15166 = ADVANCED_FACE ( 'NONE', ( #14512 ), #14252, .F. ) ;
#15167 = CARTESIAN_POINT ( 'NONE',  ( -336.3521761649653854, -110.7312321683605916, -58.62557946887767457 ) ) ;
#15168 = ORIENTED_EDGE ( 'NONE', *, *, #14190, .T. ) ;
#15170 = ORIENTED_EDGE ( 'NONE', *, *, #1863, .F. ) ;
#15169 = DIRECTION ( 'NONE',  ( 0.7765238627180437447, 0.000000000000000000, -0.6300878435817094392 ) ) ;
#15171 = ORIENTED_EDGE ( 'NONE', *, *, #17539, .T. ) ;
#15172 = VECTOR ( 'NONE', #44086, 999.9999999999998863 ) ;
#15173 = DIRECTION ( 'NONE',  ( 0.000000000000000000, -1.000000000000000000, -0.000000000000000000 ) ) ;
#15174 = DIRECTION ( 'NONE',  ( -0.000000000000000000, 1.000000000000000000, 0.000000000000000000 ) ) ;
#15175 = CARTESIAN_POINT ( 'NONE',  ( -165.6791976657750354, -189.7472609257535510, 40.49875167739065773 ) ) ;
#15176 = DIRECTION ( 'NONE',  ( 1.000000000000000000, 0.000000000000000000, -0.000000000000000000 ) ) ;
#15177 = ORIENTED_EDGE ( 'NONE', *, *, #38650, .T. ) ;
#15178 = CARTESIAN_POINT ( 'NONE',  ( -48.47912675150885065, -175.3837268820161057, 6.938893903907228378E-15 ) ) ;
#15179 = ORIENTED_EDGE ( 'NONE', *, *, #26181, .T. ) ;
#15180 = ORIENTED_EDGE ( 'NONE', *, *, #20816, .T. ) ;
#15181 = LINE ( 'NONE', #8326, #43046 ) ;
#15182 = CARTESIAN_POINT ( 'NONE',  ( -48.02249751411514467, -193.5000000000000000, 0.8896570909947569827 ) ) ;
#15183 = EDGE_CURVE ( 'NONE', #503, #26317, #46569, .T. ) ;
#15184 = PLANE ( 'NONE',  #47968 ) ;
#15185 = ORIENTED_EDGE ( 'NONE', *, *, #28792, .T. ) ;
#15186 = PLANE ( 'NONE',  #41640 ) ;
#15187 = PLANE ( 'NONE',  #49133 ) ;
#15188 = VECTOR ( 'NONE', #21383, 999.9999999999998863 ) ;
#15189 = DIRECTION ( 'NONE',  ( 0.2920567706369694982, 0.000000000000000000, 0.9564009842765243130 ) ) ;
#15190 = LINE ( 'NONE', #47255, #11132 ) ;
#15191 = ORIENTED_EDGE ( 'NONE', *, *, #28931, .T. ) ;
#15192 = PLANE ( 'NONE',  #45649 ) ;
#15193 = LINE ( 'NONE', #8072, #42507 ) ;
#15194 = EDGE_CURVE ( 'NONE', #25116, #10598, #22650, .T. ) ;
#15195 = AXIS2_PLACEMENT_3D ( 'NONE', #2589, #26228, #38325 ) ;
#15196 = FACE_BOUND ( 'NONE', #50614, .T. ) ;
#15197 = ORIENTED_EDGE ( 'NONE', *, *, #17558, .F. ) ;
#15198 = CARTESIAN_POINT ( 'NONE',  ( 37.99238433767461487, -189.7472609257535510, -90.26448786734027863 ) ) ;
#15199 = DIRECTION ( 'NONE',  ( 0.000000000000000000, 2.148744145576605138E-13, -1.000000000000000000 ) ) ;
#15200 = ORIENTED_EDGE ( 'NONE', *, *, #8334, .T. ) ;
#15201 = FACE_OUTER_BOUND ( 'NONE', #19471, .T. ) ;
#15202 = EDGE_CURVE ( 'NONE', #22344, #2222, #32002, .T. ) ;
#15203 = EDGE_LOOP ( 'NONE', ( #8476, #25000, #36593, #35173 ) ) ;
#15204 = LINE ( 'NONE', #50960, #40208 ) ;
#15205 = VECTOR ( 'NONE', #27209, 999.9999999999998863 ) ;
#15206 = FACE_BOUND ( 'NONE', #9414, .T. ) ;
#15207 = DIRECTION ( 'NONE',  ( -0.000000000000000000, 1.000000000000000000, -0.000000000000000000 ) ) ;
#15208 = FACE_OUTER_BOUND ( 'NONE', #17508, .T. ) ;
#15209 = EDGE_LOOP ( 'NONE', ( #2603, #45785, #39627, #19644 ) ) ;
#15210 = EDGE_CURVE ( 'NONE', #44900, #45352, #51538, .T. ) ;
#15211 = VERTEX_POINT ( 'NONE', #19659 ) ;
#15212 = LINE ( 'NONE', #11250, #14143 ) ;
#15213 = ORIENTED_EDGE ( 'NONE', *, *, #39305, .T. ) ;
#15214 = DIRECTION ( 'NONE',  ( 0.000000000000000000, 0.000000000000000000, -1.000000000000000000 ) ) ;
#15215 = AXIS2_PLACEMENT_3D ( 'NONE', #20280, #1086, #16625 ) ;
#15216 = ADVANCED_FACE ( 'NONE', ( #6874 ), #7831, .T. ) ;
#15217 = ADVANCED_FACE ( 'NONE', ( #23859 ), #8101, .T. ) ;
#15218 = AXIS2_PLACEMENT_3D ( 'NONE', #38837, #30961, #15199 ) ;
#15219 = LINE ( 'NONE', #26513, #39320 ) ;
#15220 = DIRECTION ( 'NONE',  ( 0.2059786187410889424, 0.000000000000000000, 0.9785564922995060311 ) ) ;
#15221 = VERTEX_POINT ( 'NONE', #24144 ) ;
#15224 = ORIENTED_EDGE ( 'NONE', *, *, #5088, .F. ) ;
#15223 = DIRECTION ( 'NONE',  ( 0.000000000000000000, 0.9350162426854169428, 0.3546048870425300148 ) ) ;
#15222 = PLANE ( 'NONE',  #29218 ) ;
#15225 = EDGE_CURVE ( 'NONE', #23268, #42035, #15997, .T. ) ;
#15226 = CARTESIAN_POINT ( 'NONE',  ( 74.60098876342243557, -183.6283474603465606, 21.82395850507348811 ) ) ;
#15227 = EDGE_LOOP ( 'NONE', ( #12008, #19742, #38613, #24372 ) ) ;
#15228 = PLANE ( 'NONE',  #33997 ) ;
#15229 = ORIENTED_EDGE ( 'NONE', *, *, #3817, .T. ) ;
#15230 = CARTESIAN_POINT ( 'NONE',  ( -101.5170032742336446, -183.6283474603465606, 112.0852863853383070 ) ) ;
#15231 = ORIENTED_EDGE ( 'NONE', *, *, #29077, .F. ) ;
#15233 = LINE ( 'NONE', #51244, #4866 ) ;
#15232 = LINE ( 'NONE', #2876, #2294 ) ;
#15234 = ORIENTED_EDGE ( 'NONE', *, *, #15999, .F. ) ;
#15235 = CARTESIAN_POINT ( 'NONE',  ( -11.80936624585915418, -175.3837268820161057, -119.5003291395395735 ) ) ;
#15236 = VERTEX_POINT ( 'NONE', #28322 ) ;
#15237 = DIRECTION ( 'NONE',  ( -0.000000000000000000, 1.000000000000000000, -0.000000000000000000 ) ) ;
#15239 = CIRCLE ( 'NONE', #26106, 4.999999999999997335 ) ;
#15238 = PLANE ( 'NONE',  #3881 ) ;
#15240 = VERTEX_POINT ( 'NONE', #201 ) ;
#15241 = EDGE_CURVE ( 'NONE', #46197, #33402, #14773, .T. ) ;
#15242 = CARTESIAN_POINT ( 'NONE',  ( 41.00573479224732409, -177.1207230881787780, -87.27805883780175122 ) ) ;
#15243 = DIRECTION ( 'NONE',  ( 0.000000000000000000, 0.9927088740980538617, -0.1205366802553232974 ) ) ;
#15244 = DIRECTION ( 'NONE',  ( -0.000000000000000000, 1.000000000000000000, 0.000000000000000000 ) ) ;
#15245 = DIRECTION ( 'NONE',  ( 0.000000000000000000, -1.000000000000000000, 0.000000000000000000 ) ) ;
#15246 = EDGE_LOOP ( 'NONE', ( #13926, #32973, #12224, #16949 ) ) ;
#15247 = DIRECTION ( 'NONE',  ( 1.000000000000000000, 0.000000000000000000, 0.000000000000000000 ) ) ;
#15248 = CARTESIAN_POINT ( 'NONE',  ( 63.10841233855954613, -175.3837268820161057, -54.07611884703302962 ) ) ;
#15249 = DIRECTION ( 'NONE',  ( -0.000000000000000000, -1.000000000000000000, 0.000000000000000000 ) ) ;
#15250 = CARTESIAN_POINT ( 'NONE',  ( -339.1964088526558498, -108.6560878169895403, 58.13482838284700449 ) ) ;
#15251 = ORIENTED_EDGE ( 'NONE', *, *, #29793, .F. ) ;
#15252 = CARTESIAN_POINT ( 'NONE',  ( -49.47868758801764955, -177.1207230881787780, 0.02963332782255607284 ) ) ;
#15253 = CARTESIAN_POINT ( 'NONE',  ( 60.00000000000001421, -113.5000000000000142, -60.00000000000001421 ) ) ;
#15254 = AXIS2_PLACEMENT_3D ( 'NONE', #46942, #26159, #2769 ) ;
#15255 = LINE ( 'NONE', #34954, #34494 ) ;
#15257 = EDGE_LOOP ( 'NONE', ( #18820, #43888, #35865, #28450 ) ) ;
#15256 = DIRECTION ( 'NONE',  ( -0.4566292373937077542, 0.000000000000000000, -0.8896570909947499883 ) ) ;
#15258 = ORIENTED_EDGE ( 'NONE', *, *, #31344, .T. ) ;
#15259 = VECTOR ( 'NONE', #46156, 1000.000000000000000 ) ;
#15260 = VECTOR ( 'NONE', #41553, 1000.000000000000000 ) ;
#15261 = DIRECTION ( 'NONE',  ( 1.000000000000000000, 0.000000000000000000, -0.000000000000000000 ) ) ;
#15262 = CARTESIAN_POINT ( 'NONE',  ( 23.54917025746143722, -177.1207230881787780, -100.9358816284410523 ) ) ;
#15263 = CARTESIAN_POINT ( 'NONE',  ( -330.4913330509368166, -67.57827586672175357, -21.74306257088736061 ) ) ;
#15264 = CARTESIAN_POINT ( 'NONE',  ( 14.94072793302542124, -193.5000000000000000, 107.7168604805791574 ) ) ;
#15265 = DIRECTION ( 'NONE',  ( 0.000000000000000000, 0.000000000000000000, 1.000000000000000000 ) ) ;
#15266 = ORIENTED_EDGE ( 'NONE', *, *, #39470, .T. ) ;
#15267 = EDGE_CURVE ( 'NONE', #19264, #16302, #51742, .T. ) ;
#15268 = LINE ( 'NONE', #27609, #26856 ) ;
#15269 = VECTOR ( 'NONE', #21398, 1000.000000000000227 ) ;
#15270 = VERTEX_POINT ( 'NONE', #44096 ) ;
#15271 = AXIS2_PLACEMENT_3D ( 'NONE', #44299, #8290, #11436 ) ;
#15272 = ORIENTED_EDGE ( 'NONE', *, *, #6685, .F. ) ;
#15273 = VECTOR ( 'NONE', #38018, 1000.000000000000114 ) ;
#15274 = ORIENTED_EDGE ( 'NONE', *, *, #21872, .F. ) ;
#15275 = CARTESIAN_POINT ( 'NONE',  ( -169.7849785064912567, -193.5000000000000000, -25.70779184431766851 ) ) ;
#15276 = EDGE_CURVE ( 'NONE', #30411, #32877, #31758, .T. ) ;
#15277 = CARTESIAN_POINT ( 'NONE',  ( 46.00000000000000711, 0.000000000000000000, 46.00000000000000000 ) ) ;
#15278 = ORIENTED_EDGE ( 'NONE', *, *, #17856, .T. ) ;
#15279 = EDGE_CURVE ( 'NONE', #10734, #3069, #12055, .T. ) ;
#15280 = DIRECTION ( 'NONE',  ( 1.000000000000000000, -0.000000000000000000, -0.000000000000000000 ) ) ;
#15281 = LINE ( 'NONE', #18965, #20204 ) ;
#15284 = VERTEX_POINT ( 'NONE', #12291 ) ;
#15283 = DIRECTION ( 'NONE',  ( -0.000000000000000000, 1.000000000000000000, -0.000000000000000000 ) ) ;
#15282 = LINE ( 'NONE', #31298, #7361 ) ;
#15285 = EDGE_CURVE ( 'NONE', #51297, #6623, #47799, .T. ) ;
#15286 = DIRECTION ( 'NONE',  ( 0.2635871660690715101, 0.000000000000000000, -0.9646355819083576311 ) ) ;
#15287 = EDGE_LOOP ( 'NONE', ( #17659, #38002, #12991, #8698 ) ) ;
#15288 = DIRECTION ( 'NONE',  ( 0.000000000000000000, 0.000000000000000000, 1.000000000000000000 ) ) ;
#15289 = AXIS2_PLACEMENT_3D ( 'NONE', #40568, #49535, #28485 ) ;
#15290 = VERTEX_POINT ( 'NONE', #52007 ) ;
#15291 = CARTESIAN_POINT ( 'NONE',  ( -48.30901192927175458, -189.7472609257535510, -124.9998842437354227 ) ) ;
#15292 = CARTESIAN_POINT ( 'NONE',  ( -111.6834028793037987, -193.5000000000000000, 106.6827995071088253 ) ) ;
#15293 = AXIS2_PLACEMENT_3D ( 'NONE', #35335, #6969, #51914 ) ;
#15295 = DIRECTION ( 'NONE',  ( 0.000000000000000000, 0.000000000000000000, -1.000000000000000000 ) ) ;
#15294 = LINE ( 'NONE', #39201, #11460 ) ;
#15296 = ORIENTED_EDGE ( 'NONE', *, *, #35032, .F. ) ;
#15297 = AXIS2_PLACEMENT_3D ( 'NONE', #45458, #784, #9200 ) ;
#15298 = LINE ( 'NONE', #35509, #13917 ) ;
#15299 = ORIENTED_EDGE ( 'NONE', *, *, #23102, .F. ) ;
#15300 = PLANE ( 'NONE',  #24810 ) ;
#15301 = ORIENTED_EDGE ( 'NONE', *, *, #10879, .F. ) ;
#15302 = CARTESIAN_POINT ( 'NONE',  ( -170.0000000000000284, -130.6726371812771959, 60.00000000000000711 ) ) ;
#15303 = CARTESIAN_POINT ( 'NONE',  ( -48.47912675150885065, -175.3837268820161057, 6.938893903907228378E-15 ) ) ;
#15304 = VERTEX_POINT ( 'NONE', #20179 ) ;
#15305 = CARTESIAN_POINT ( 'NONE',  ( 75.48400724637754422, -183.6283474603465606, -16.06677968424457248 ) ) ;
#15306 = CIRCLE ( 'NONE', #17824, 125.0000000000000000 ) ;
#15308 = AXIS2_PLACEMENT_3D ( 'NONE', #26922, #10904, #39520 ) ;
#15307 = FACE_OUTER_BOUND ( 'NONE', #16389, .T. ) ;
#15309 = ORIENTED_EDGE ( 'NONE', *, *, #45941, .T. ) ;
#15310 = DIRECTION ( 'NONE',  ( 0.000000000000000000, 0.000000000000000000, -1.000000000000000000 ) ) ;
#15311 = ORIENTED_EDGE ( 'NONE', *, *, #26251, .F. ) ;
#15312 = VECTOR ( 'NONE', #22810, 1000.000000000000000 ) ;
#15313 = VECTOR ( 'NONE', #6947, 1000.000000000000114 ) ;
#15314 = LINE ( 'NONE', #7440, #4372 ) ;
#15315 = VERTEX_POINT ( 'NONE', #8607 ) ;
#15316 = FACE_OUTER_BOUND ( 'NONE', #41863, .T. ) ;
#15317 = DIRECTION ( 'NONE',  ( 1.000000000000000000, -0.000000000000000000, -0.000000000000000000 ) ) ;
#15318 = DIRECTION ( 'NONE',  ( -0.000000000000000000, 1.000000000000000000, -0.000000000000000000 ) ) ;
#15319 = CARTESIAN_POINT ( 'NONE',  ( 141.7825277784304205, -213.5000000000000000, -9.999999999999987566 ) ) ;
#15320 = LINE ( 'NONE', #36061, #48006 ) ;
#15321 = CARTESIAN_POINT ( 'NONE',  ( -336.3521761649654422, -166.5797264208035244, 40.34602258462248159 ) ) ;
#15323 = ORIENTED_EDGE ( 'NONE', *, *, #45602, .F. ) ;
#15322 = LINE ( 'NONE', #3484, #29513 ) ;
#15324 = SHAPE_REPRESENTATION ( 'Eccentric Cam Locking Shaft', ( #31742 ), #42661 ) ;
#15325 = CIRCLE ( 'NONE', #9441, 125.0000000000000000 ) ;
#15326 = ADVANCED_FACE ( 'NONE', ( #30786 ), #24642, .F. ) ;
#15327 = ORIENTED_EDGE ( 'NONE', *, *, #49497, .F. ) ;
#15328 = ADVANCED_FACE ( 'NONE', ( #8364 ), #24388, .T. ) ;
#15329 = EDGE_CURVE ( 'NONE', #22157, #14204, #19646, .T. ) ;
#15330 = DIRECTION ( 'NONE',  ( 0.000000000000000000, 1.000000000000000000, 0.000000000000000000 ) ) ;
#15331 = EDGE_CURVE ( 'NONE', #50010, #16064, #459, .T. ) ;
#15332 = CIRCLE ( 'NONE', #16161, 4.999999999999997335 ) ;
#15333 = DIRECTION ( 'NONE',  ( 0.000000000000000000, 0.8229838658936536877, -0.5680647467311596976 ) ) ;
#15334 = ORIENTED_EDGE ( 'NONE', *, *, #29022, .F. ) ;
#15335 = EDGE_LOOP ( 'NONE', ( #4178, #943, #31882, #32275 ) ) ;
#15336 = DIRECTION ( 'NONE',  ( 0.000000000000000000, 0.9709418174260534551, 0.2393156642875516327 ) ) ;
#15337 = ADVANCED_FACE ( 'NONE', ( #12560 ), #28578, .T. ) ;
#15338 = ORIENTED_EDGE ( 'NONE', *, *, #50136, .T. ) ;
#15339 = LINE ( 'NONE', #16114, #25868 ) ;
#15340 = DIRECTION ( 'NONE',  ( 0.000000000000000000, 0.000000000000000000, 1.000000000000000000 ) ) ;
#15341 = ADVANCED_FACE ( 'NONE', ( #37253 ), #28831, .T. ) ;
#15342 = EDGE_CURVE ( 'NONE', #30647, #23694, #24915, .T. ) ;
#15343 = DIRECTION ( 'NONE',  ( 0.000000000000000000, -0.8229838658936495799, 0.5680647467311656929 ) ) ;
#15344 = DIRECTION ( 'NONE',  ( 0.9266896074318317078, 0.000000000000000000, 0.3758275821142421647 ) ) ;
#15345 = VERTEX_POINT ( 'NONE', #49086 ) ;
#15346 = CIRCLE ( 'NONE', #44717, 125.0000000000000000 ) ;
#15347 = EDGE_LOOP ( 'NONE', ( #12867, #48424, #43407, #1150 ) ) ;
#15348 = EDGE_CURVE ( 'NONE', #36071, #11143, #1514, .T. ) ;
#15349 = ORIENTED_EDGE ( 'NONE', *, *, #37644, .T. ) ;
#15350 = LINE ( 'NONE', #35557, #34199 ) ;
#15351 = CARTESIAN_POINT ( 'NONE',  ( -365.0000000000001137, -168.5000000000000284, 5.000000000000001776 ) ) ;
#15352 = CIRCLE ( 'NONE', #27070, 125.0000000000000000 ) ;
#15353 = CARTESIAN_POINT ( 'NONE',  ( -48.47912675150885065, -183.6283474603465606, 6.938893903907228378E-15 ) ) ;
#15354 = AXIS2_PLACEMENT_3D ( 'NONE', #47066, #23650, #11043 ) ;
#15355 = ADVANCED_FACE ( 'NONE', ( #41714 ), #986, .T. ) ;
#15356 = FACE_OUTER_BOUND ( 'NONE', #27692, .T. ) ;
#15357 = PLANE ( 'NONE',  #12128 ) ;
#15358 = EDGE_LOOP ( 'NONE', ( #9929, #18712, #24159, #20826 ) ) ;
#15359 = EDGE_CURVE ( 'NONE', #21361, #13514, #25176, .T. ) ;
#15360 = UNCERTAINTY_MEASURE_WITH_UNIT (LENGTH_MEASURE( 1.000000000000000082E-05 ), #35774, 'distance_accuracy_value', 'NONE');
#15361 = CIRCLE ( 'NONE', #42198, 125.0000000000000000 ) ;
#15362 = LINE ( 'NONE', #88, #3822 ) ;
#15363 = CARTESIAN_POINT ( 'NONE',  ( -336.3521761649654422, -179.5993808087905279, -18.46045550523168899 ) ) ;
#15364 = ORIENTED_EDGE ( 'NONE', *, *, #22554, .T. ) ;
#15365 = ORIENTED_EDGE ( 'NONE', *, *, #32107, .T. ) ;
#15366 = LINE ( 'NONE', #38738, #39864 ) ;
#15367 = DIRECTION ( 'NONE',  ( -0.000000000000000000, -1.000000000000000000, 0.000000000000000000 ) ) ;
#15368 = EDGE_LOOP ( 'NONE', ( #736, #10011, #34622, #9362 ) ) ;
#15369 = CARTESIAN_POINT ( 'NONE',  ( -305.0000000000000568, -73.83865025250327108, -33.67120938215323633 ) ) ;
#15370 = AXIS2_PLACEMENT_3D ( 'NONE', #18291, #6202, #30603 ) ;
#15371 = DIRECTION ( 'NONE',  ( -1.000000000000000000, 0.000000000000000000, 0.000000000000000000 ) ) ;
#15372 = CARTESIAN_POINT ( 'NONE',  ( -48.47912675150885065, -177.1207230881787780, 6.938893903907228378E-15 ) ) ;
#15373 = EDGE_LOOP ( 'NONE', ( #4566, #15546, #39368, #29987 ) ) ;
#15374 = LINE ( 'NONE', #14337, #4068 ) ;
#15375 = EDGE_CURVE ( 'NONE', #11314, #43961, #45165, .T. ) ;
#15376 = CIRCLE ( 'NONE', #14553, 60.00000000000000000 ) ;
#15377 = ORIENTED_EDGE ( 'NONE', *, *, #39363, .F. ) ;
#15378 = DIRECTION ( 'NONE',  ( -0.000000000000000000, 1.000000000000000000, 0.000000000000000000 ) ) ;
#15379 = CARTESIAN_POINT ( 'NONE',  ( -0.3054481938615516423, -183.6283474603465606, 115.3442529744090450 ) ) ;
#15380 = EDGE_LOOP ( 'NONE', ( #6356, #17714, #27396, #13694 ) ) ;
#15381 = CARTESIAN_POINT ( 'NONE',  ( 116.9235303384055840, -213.5000000000000000, 2.819679052520814125E-14 ) ) ;
#15382 = FACE_OUTER_BOUND ( 'NONE', #34463, .T. ) ;
#15383 = CARTESIAN_POINT ( 'NONE',  ( -158.0280232639029236, -189.7472609257535510, 60.19999396110247858 ) ) ;
#15384 = AXIS2_PLACEMENT_3D ( 'NONE', #4202, #773, #36492 ) ;
#15385 = CARTESIAN_POINT ( 'NONE',  ( -339.1964088526558498, -123.5000000000000284, 0.000000000000000000 ) ) ;
#15386 = AXIS2_PLACEMENT_3D ( 'NONE', #1755, #5965, #17792 ) ;
#15387 = FACE_OUTER_BOUND ( 'NONE', #3490, .T. ) ;
#15388 = VERTEX_POINT ( 'NONE', #17040 ) ;
#15389 = EDGE_CURVE ( 'NONE', #12090, #10873, #9150, .T. ) ;
#15390 = ORIENTED_EDGE ( 'NONE', *, *, #47135, .F. ) ;
#15391 = AXIS2_PLACEMENT_3D ( 'NONE', #28159, #32637, #12398 ) ;
#15392 = PLANE ( 'NONE',  #10520 ) ;
#15394 = ORIENTED_EDGE ( 'NONE', *, *, #11574, .T. ) ;
#15393 = CARTESIAN_POINT ( 'NONE',  ( 69.14211578623219623, -183.6283474603465606, 42.31126686685117733 ) ) ;
#15395 = ADVANCED_FACE ( 'NONE', ( #21750 ), #12808, .T. ) ;
#15396 = EDGE_CURVE ( 'NONE', #51222, #31290, #5210, .T. ) ;
#15397 = ORIENTED_EDGE ( 'NONE', *, *, #32193, .T. ) ;
#15398 = EDGE_CURVE ( 'NONE', #9161, #49147, #41186, .T. ) ;
#15399 = LINE ( 'NONE', #18807, #35517 ) ;
#15400 = EDGE_CURVE ( 'NONE', #8154, #41535, #49610, .T. ) ;
#15401 = CIRCLE ( 'NONE', #44765, 10.00000000000000178 ) ;
#15402 = EDGE_CURVE ( 'NONE', #10873, #26098, #44883, .T. ) ;
#15403 = DIRECTION ( 'NONE',  ( -1.000000000000000000, 0.000000000000000000, 0.000000000000000000 ) ) ;
#15404 = VERTEX_POINT ( 'NONE', #29361 ) ;
#15405 = LINE ( 'NONE', #31414, #34820 ) ;
#15406 = EDGE_CURVE ( 'NONE', #650, #4203, #13594, .T. ) ;
#15407 = FACE_OUTER_BOUND ( 'NONE', #26786, .T. ) ;
#15408 = EDGE_CURVE ( 'NONE', #6739, #40019, #8726, .T. ) ;
#15409 = ORIENTED_EDGE ( 'NONE', *, *, #50358, .F. ) ;
#15410 = CYLINDRICAL_SURFACE ( 'NONE', #19124, 10.00000000000000178 ) ;
#15411 = VECTOR ( 'NONE', #40686, 1000.000000000000000 ) ;
#15412 = EDGE_CURVE ( 'NONE', #46461, #26719, #33901, .T. ) ;
#15413 = CARTESIAN_POINT ( 'NONE',  ( -339.1964088526558498, -167.9936954712156592, -38.74998146212110584 ) ) ;
#15414 = DIRECTION ( 'NONE',  ( 0.000000000000000000, 0.000000000000000000, 1.000000000000000000 ) ) ;
#15415 = EDGE_LOOP ( 'NONE', ( #14492, #23661, #6455, #21771 ) ) ;
#15416 = EDGE_LOOP ( 'NONE', ( #24276, #11015, #50471, #48265 ) ) ;
#15417 = CIRCLE ( 'NONE', #310, 125.0000000000000000 ) ;
#15418 = EDGE_CURVE ( 'NONE', #48304, #48442, #37511, .T. ) ;
#15419 = ORIENTED_EDGE ( 'NONE', *, *, #14322, .T. ) ;
#15420 = DIRECTION ( 'NONE',  ( 0.000000000000000000, 0.000000000000000000, -1.000000000000000000 ) ) ;
#15421 = CYLINDRICAL_SURFACE ( 'NONE', #36068, 125.0000000000000000 ) ;
#15422 = ADVANCED_FACE ( 'NONE', ( #29617 ), #45669, .T. ) ;
#15423 = LINE ( 'NONE', #31428, #50297 ) ;
#15424 = CARTESIAN_POINT ( 'NONE',  ( -332.3517673607765914, -64.73342574900661361, 5.491276508483657892 ) ) ;
#15425 = CARTESIAN_POINT ( 'NONE',  ( 60.51025563957495734, -175.3837268820161057, 59.13814366165117065 ) ) ;
#15426 = EDGE_LOOP ( 'NONE', ( #12597, #1823, #11580, #25695 ) ) ;
#15427 = EDGE_CURVE ( 'NONE', #30276, #3919, #34351, .T. ) ;
#15428 = VECTOR ( 'NONE', #27365, 1000.000000000000000 ) ;
#15429 = EDGE_CURVE ( 'NONE', #186, #43501, #38280, .T. ) ;
#15430 = CARTESIAN_POINT ( 'NONE',  ( -112.7586829773731267, -189.7472609257535510, -107.2060569716373521 ) ) ;
#15431 = ORIENTED_EDGE ( 'NONE', *, *, #6987, .F. ) ;
#15433 = EDGE_LOOP ( 'NONE', ( #6826, #2354, #22798, #24010 ) ) ;
#15432 = CARTESIAN_POINT ( 'NONE',  ( -48.53836737940257251, -189.7472609257535510, 0.9982437317643279018 ) ) ;
#15434 = AXIS2_PLACEMENT_3D ( 'NONE', #1002, #12573, #44636 ) ;
#15435 = ORIENTED_EDGE ( 'NONE', *, *, #50700, .T. ) ;
#15436 = LINE ( 'NONE', #30655, #42589 ) ;
#15437 = CARTESIAN_POINT ( 'NONE',  ( -159.0901268547125653, -193.5000000000000000, 58.22548115875957109 ) ) ;
#15438 = LINE ( 'NONE', #39575, #11207 ) ;
#15439 = DIRECTION ( 'NONE',  ( -0.9982437317643222396, 0.000000000000000000, 0.05924062789370006937 ) ) ;
#15440 = ORIENTED_EDGE ( 'NONE', *, *, #33400, .T. ) ;
#15441 = FACE_OUTER_BOUND ( 'NONE', #8746, .T. ) ;
#15442 = ORIENTED_EDGE ( 'NONE', *, *, #23915, .F. ) ;
#15443 = ADVANCED_FACE ( 'NONE', ( #26970 ), #14640, .T. ) ;
#15444 = ORIENTED_EDGE ( 'NONE', *, *, #11473, .F. ) ;
#15445 = LINE ( 'NONE', #28727, #32295 ) ;
#15446 = DIRECTION ( 'NONE',  ( 1.000000000000000000, 0.000000000000000000, 0.000000000000000000 ) ) ;
#15447 = CARTESIAN_POINT ( 'NONE',  ( 76.52053249983504202, -177.1207230881787780, -0.2918682030015403162 ) ) ;
#15448 = AXIS2_PLACEMENT_3D ( 'NONE', #16028, #4713, #20743 ) ;
#15449 = CARTESIAN_POINT ( 'NONE',  ( 53.18081239921338721, -175.3837268820161057, -72.73415134495935774 ) ) ;
#15450 = FACE_OUTER_BOUND ( 'NONE', #7793, .T. ) ;
#15451 = DIRECTION ( 'NONE',  ( 0.000000000000000000, 0.000000000000000000, 1.000000000000000000 ) ) ;
#15452 = ORIENTED_EDGE ( 'NONE', *, *, #21501, .T. ) ;
#15453 = LINE ( 'NONE', #43558, #33882 ) ;
#15454 = DIRECTION ( 'NONE',  ( 0.000000000000000000, 0.000000000000000000, -1.000000000000000000 ) ) ;
#15455 = CIRCLE ( 'NONE', #3685, 125.0000000000000000 ) ;
#15456 = CARTESIAN_POINT ( 'NONE',  ( -173.2419626162308646, -177.1207230881787780, 7.696413904698416353 ) ) ;
#15457 = ORIENTED_EDGE ( 'NONE', *, *, #16467, .F. ) ;
#15458 = CARTESIAN_POINT ( 'NONE',  ( -48.47912675150885065, -177.1207230881787780, 6.938893903907228378E-15 ) ) ;
#15459 = CARTESIAN_POINT ( 'NONE',  ( 0.000000000000000000, 65.00000000000000000, 0.000000000000000000 ) ) ;
#15460 = ADVANCED_FACE ( 'NONE', ( #51178 ), #3062, .T. ) ;
#15461 = ORIENTED_EDGE ( 'NONE', *, *, #20343, .F. ) ;
#15462 = EDGE_CURVE ( 'NONE', #12462, #48052, #11239, .T. ) ;
#15463 = LINE ( 'NONE', #35410, #6950 ) ;
#15464 = VECTOR ( 'NONE', #20707, 1000.000000000000000 ) ;
#15465 = VERTEX_POINT ( 'NONE', #30923 ) ;
#15466 = CARTESIAN_POINT ( 'NONE',  ( -336.3521761649654422, -64.50000000000000000, -1.632288850093980725 ) ) ;
#15467 = FACE_BOUND ( 'NONE', #33514, .T. ) ;
#15469 = ORIENTED_EDGE ( 'NONE', *, *, #38051, .F. ) ;
#15468 = FACE_OUTER_BOUND ( 'NONE', #27083, .T. ) ;
#15470 = CARTESIAN_POINT ( 'NONE',  ( -336.3521761649654422, -171.1288023355047585, 34.85916744524404720 ) ) ;
#15471 = ORIENTED_EDGE ( 'NONE', *, *, #17883, .T. ) ;
#15472 = VERTEX_POINT ( 'NONE', #19105 ) ;
#15473 = DIRECTION ( 'NONE',  ( 0.000000000000000000, 1.000000000000000000, 0.000000000000000000 ) ) ;
#15474 = ORIENTED_EDGE ( 'NONE', *, *, #51284, .F. ) ;
#15475 = EDGE_CURVE ( 'NONE', #29517, #38097, #43125, .T. ) ;
#15476 = DIRECTION ( 'NONE',  ( 0.000000000000000000, -1.000000000000000000, 0.000000000000000000 ) ) ;
#15477 = VECTOR ( 'NONE', #13224, 1000.000000000000000 ) ;
#15478 = AXIS2_PLACEMENT_3D ( 'NONE', #2630, #10262, #18154 ) ;
#15479 = AXIS2_PLACEMENT_3D ( 'NONE', #8265, #24295, #20341 ) ;
#15480 = ADVANCED_FACE ( 'NONE', ( #42485 ), #38790, .T. ) ;
#15481 = SURFACE_STYLE_USAGE ( .BOTH. , #35429 ) ;
#15482 = CARTESIAN_POINT ( 'NONE',  ( -170.0000000000000284, -123.5000000000000284, -41.63467731922663972 ) ) ;
#15483 = EDGE_LOOP ( 'NONE', ( #5493, #37185, #32939, #45616 ) ) ;
#15486 = ORIENTED_EDGE ( 'NONE', *, *, #44353, .T. ) ;
#15485 = DIRECTION ( 'NONE',  ( 0.000000000000000000, 1.000000000000000000, 0.000000000000000000 ) ) ;
#15484 = DIRECTION ( 'NONE',  ( -0.000000000000000000, 1.000000000000000000, -0.000000000000000000 ) ) ;
#15487 = CARTESIAN_POINT ( 'NONE',  ( -161.6832731452239784, -189.7472609257535510, -53.00774697410100345 ) ) ;
#15488 = VERTEX_POINT ( 'NONE', #10423 ) ;
#15489 = DIRECTION ( 'NONE',  ( 0.000000000000000000, 0.000000000000000000, -1.000000000000000000 ) ) ;
#15490 = ORIENTED_EDGE ( 'NONE', *, *, #26294, .T. ) ;
#15491 = DIRECTION ( 'NONE',  ( 0.000000000000000000, -0.000000000000000000, 1.000000000000000000 ) ) ;
#15492 = VERTEX_POINT ( 'NONE', #2796 ) ;
#15494 = CARTESIAN_POINT ( 'NONE',  ( 12.99855592850622443, -177.1207230881787780, 108.8370090194294875 ) ) ;
#15493 = DIRECTION ( 'NONE',  ( 0.000000000000000000, 0.000000000000000000, 1.000000000000000000 ) ) ;
#15495 = AXIS2_PLACEMENT_3D ( 'NONE', #36405, #400, #16456 ) ;
#15496 = ORIENTED_EDGE ( 'NONE', *, *, #42547, .T. ) ;
#15497 = DIRECTION ( 'NONE',  ( 0.8757349421956379665, 0.000000000000000000, -0.4827922027307427477 ) ) ;
#15498 = ORIENTED_EDGE ( 'NONE', *, *, #16334, .T. ) ;
#15499 = LINE ( 'NONE', #51500, #4401 ) ;
#15500 = DIRECTION ( 'NONE',  ( -0.000000000000000000, 1.000000000000000000, -0.000000000000000000 ) ) ;
#15501 = DIRECTION ( 'NONE',  ( 0.000000000000000000, 0.000000000000000000, -1.000000000000000000 ) ) ;
#15502 = DIRECTION ( 'NONE',  ( 0.000000000000000000, 0.000000000000000000, -1.000000000000000000 ) ) ;
#15503 = PLANE ( 'NONE',  #22380 ) ;
#15504 = ADVANCED_BREP_SHAPE_REPRESENTATION ( '', ( #1141, #31742 ), #35946 ) ;
#15505 = CYLINDRICAL_SURFACE ( 'NONE', #20527, 20.00000000000000000 ) ;
#15506 = ORIENTED_EDGE ( 'NONE', *, *, #1199, .F. ) ;
#15507 = CARTESIAN_POINT ( 'NONE',  ( 22.37192613399955476, 5.000000000000000888, -6.938893903907228378E-15 ) ) ;
#15508 = LINE ( 'NONE', #20218, #12877 ) ;
#15509 = FACE_OUTER_BOUND ( 'NONE', #39824, .T. ) ;
#15510 = DIRECTION ( 'NONE',  ( 1.000000000000000000, 0.000000000000000000, -0.000000000000000000 ) ) ;
#15511 = ORIENTED_EDGE ( 'NONE', *, *, #11520, .F. ) ;
#15512 = CARTESIAN_POINT ( 'NONE',  ( -48.53836737940255119, -189.7472609257535510, -0.9982437317643153563 ) ) ;
#15513 = CARTESIAN_POINT ( 'NONE',  ( 40.30419662299490824, -183.6283474603465606, -87.99159897727903967 ) ) ;
#15514 = AXIS2_PLACEMENT_3D ( 'NONE', #47095, #26075, #6125 ) ;
#15515 = CIRCLE ( 'NONE', #50747, 125.0000000000000000 ) ;
#15516 = DIRECTION ( 'NONE',  ( -0.000000000000000000, 1.000000000000000000, -0.000000000000000000 ) ) ;
#15518 = ORIENTED_EDGE ( 'NONE', *, *, #22092, .F. ) ;
#15517 = LINE ( 'NONE', #46298, #40888 ) ;
#15519 = EDGE_CURVE ( 'NONE', #2868, #5990, #10169, .T. ) ;
#15520 = ORIENTED_EDGE ( 'NONE', *, *, #25374, .T. ) ;
#15521 = ORIENTED_EDGE ( 'NONE', *, *, #34965, .F. ) ;
#15522 = CIRCLE ( 'NONE', #44886, 125.0000000000000000 ) ;
#15523 = CARTESIAN_POINT ( 'NONE',  ( -29.73468717939733708, -193.5000000000000000, 123.5865930638410930 ) ) ;
#15524 = DIRECTION ( 'NONE',  ( 0.000000000000000000, 6.753856733136369375E-14, 1.000000000000000000 ) ) ;
#15525 = VECTOR ( 'NONE', #6821, 1000.000000000000000 ) ;
#15526 = DIRECTION ( 'NONE',  ( 0.4566292373937140270, 0.000000000000000000, -0.8896570909947467687 ) ) ;
#15527 = CARTESIAN_POINT ( 'NONE',  ( -124.4642912599203584, -189.7472609257535510, 99.25348746834863789 ) ) ;
#15528 = ORIENTED_EDGE ( 'NONE', *, *, #14751, .F. ) ;
#15529 = CIRCLE ( 'NONE', #34015, 60.00000000000000000 ) ;
#15530 = CYLINDRICAL_SURFACE ( 'NONE', #22671, 4.999999999999997335 ) ;
#15531 = VERTEX_POINT ( 'NONE', #23032 ) ;
#15532 = ORIENTED_EDGE ( 'NONE', *, *, #5424, .F. ) ;
#15533 = ORIENTED_EDGE ( 'NONE', *, *, #3578, .T. ) ;
#15534 = ADVANCED_FACE ( 'NONE', ( #15163 ), #22782, .F. ) ;
#15535 = LINE ( 'NONE', #12353, #46033 ) ;
#15536 = CARTESIAN_POINT ( 'NONE',  ( -332.3517673607765914, -169.4076645216271402, -37.15394033962039089 ) ) ;
#15537 = VERTEX_POINT ( 'NONE', #10692 ) ;
#15538 = FACE_OUTER_BOUND ( 'NONE', #3990, .T. ) ;
#15539 = PLANE ( 'NONE',  #3395 ) ;
#15542 = ORIENTED_EDGE ( 'NONE', *, *, #1048, .F. ) ;
#15541 = DIRECTION ( 'NONE',  ( 0.000000000000000000, -1.000000000000000000, 0.000000000000000000 ) ) ;
#15540 = DIRECTION ( 'NONE',  ( 0.4677363560876406923, 0.000000000000000000, 0.8838680338115275648 ) ) ;
#15543 = VECTOR ( 'NONE', #9301, 999.9999999999998863 ) ;
#15544 = PLANE ( 'NONE',  #24788 ) ;
#15545 = CIRCLE ( 'NONE', #7999, 60.00000000000000000 ) ;
#15546 = ORIENTED_EDGE ( 'NONE', *, *, #5882, .F. ) ;
#15547 = DIRECTION ( 'NONE',  ( 1.000000000000000000, 2.086444717177546192E-17, 8.465038975556398759E-17 ) ) ;
#15548 = EDGE_LOOP ( 'NONE', ( #18398, #23567, #17046, #34800 ) ) ;
#15549 = VECTOR ( 'NONE', #5893, 1000.000000000000000 ) ;
#15550 = DIRECTION ( 'NONE',  ( 1.000000000000000000, -0.000000000000000000, -0.000000000000000000 ) ) ;
#15551 = LINE ( 'NONE', #11605, #50644 ) ;
#15553 = CARTESIAN_POINT ( 'NONE',  ( -48.47912675150885065, -183.6283474603465606, 6.938893903907228378E-15 ) ) ;
#15552 = CARTESIAN_POINT ( 'NONE',  ( 0.000000000000000000, 51.50530197288473744, -13.91328567938375294 ) ) ;
#15554 = VECTOR ( 'NONE', #29596, 1000.000000000000000 ) ;
#15555 = ORIENTED_EDGE ( 'NONE', *, *, #37713, .T. ) ;
#15556 = LINE ( 'NONE', #23189, #40754 ) ;
#15557 = DIRECTION ( 'NONE',  ( -0.000000000000000000, 0.7485107481710999711, -0.6631226582407964143 ) ) ;
#15558 = ORIENTED_EDGE ( 'NONE', *, *, #2546, .F. ) ;
#15559 = VECTOR ( 'NONE', #47749, 1000.000000000000227 ) ;
#15560 = CARTESIAN_POINT ( 'NONE',  ( -109.0835867659424565, -193.5000000000000000, -109.3256576763154726 ) ) ;
#15561 = AXIS2_PLACEMENT_3D ( 'NONE', #14834, #38716, #50828 ) ;
#15562 = FACE_OUTER_BOUND ( 'NONE', #3172, .T. ) ;
#15563 = ADVANCED_FACE ( 'NONE', ( #46443 ), #18333, .F. ) ;
#15564 = VERTEX_POINT ( 'NONE', #38550 ) ;
#15565 = CARTESIAN_POINT ( 'NONE',  ( -25.00456841203573077, 65.00000000000000000, 0.000000000000000000 ) ) ;
#15566 = AXIS2_PLACEMENT_3D ( 'NONE', #26521, #42040, #14203 ) ;
#15567 = CARTESIAN_POINT ( 'NONE',  ( -339.1964088526558498, -131.1080185721124849, 58.50955523165764305 ) ) ;
#15568 = EDGE_CURVE ( 'NONE', #11646, #15597, #42756, .T. ) ;
#15569 = DIRECTION ( 'NONE',  ( 0.000000000000000000, 0.000000000000000000, 1.000000000000000000 ) ) ;
#15570 = AXIS2_PLACEMENT_3D ( 'NONE', #51481, #27557, #43588 ) ;
#15571 = VERTEX_POINT ( 'NONE', #42219 ) ;
#15572 = DIRECTION ( 'NONE',  ( 0.000000000000000000, -0.000000000000000000, -1.000000000000000000 ) ) ;
#15573 = EDGE_LOOP ( 'NONE', ( #2587, #20912, #48744, #5339 ) ) ;
#15574 = CARTESIAN_POINT ( 'NONE',  ( -102.5006284722404502, -177.1207230881787780, -112.7238987608084386 ) ) ;
#15575 = DIRECTION ( 'NONE',  ( 0.000000000000000000, -1.000000000000000000, 0.000000000000000000 ) ) ;
#15576 = CYLINDRICAL_SURFACE ( 'NONE', #31907, 125.0000000000000000 ) ;
#15577 = FACE_OUTER_BOUND ( 'NONE', #9668, .T. ) ;
#15578 = CARTESIAN_POINT ( 'NONE',  ( 11.61413489515543418, -177.1207230881787780, -109.6074810615842381 ) ) ;
#15579 = ADVANCED_FACE ( 'NONE', ( #26718 ), #18577, .T. ) ;
#15580 = EDGE_CURVE ( 'NONE', #12334, #10851, #34848, .T. ) ;
#15581 = FACE_OUTER_BOUND ( 'NONE', #34065, .T. ) ;
#15582 = ADVANCED_FACE ( 'NONE', ( #46968 ), #10949, .T. ) ;
#15583 = CIRCLE ( 'NONE', #25624, 60.00000000000000000 ) ;
#15584 = DIRECTION ( 'NONE',  ( -0.000000000000000000, 1.000000000000000000, -0.000000000000000000 ) ) ;
#15585 = LINE ( 'NONE', #16358, #33138 ) ;
#15587 = ORIENTED_EDGE ( 'NONE', *, *, #11812, .F. ) ;
#15586 = CARTESIAN_POINT ( 'NONE',  ( -67.10529315269982931, -183.6283474603465606, -122.5936119678274565 ) ) ;
#15588 = VECTOR ( 'NONE', #37917, 1000.000000000000000 ) ;
#15589 = VECTOR ( 'NONE', #14488, 1000.000000000000000 ) ;
#15590 = ORIENTED_EDGE ( 'NONE', *, *, #20484, .F. ) ;
#15591 = DIRECTION ( 'NONE',  ( -0.000000000000000000, 1.000000000000000000, -0.000000000000000000 ) ) ;
#15592 = CARTESIAN_POINT ( 'NONE',  ( -11.47118876952528765, -189.7472609257535510, 118.3487137068149053 ) ) ;
#15593 = ORIENTED_EDGE ( 'NONE', *, *, #32069, .F. ) ;
#15594 = ORIENTED_EDGE ( 'NONE', *, *, #34209, .F. ) ;
#15595 = CARTESIAN_POINT ( 'NONE',  ( -336.3521761649654422, -66.84438072661991725, -16.67542351306652648 ) ) ;
#15596 = VECTOR ( 'NONE', #26137, 1000.000000000000000 ) ;
#15597 = VERTEX_POINT ( 'NONE', #47742 ) ;
#15598 = EDGE_CURVE ( 'NONE', #30219, #28004, #43777, .T. ) ;
#15599 = CARTESIAN_POINT ( 'NONE',  ( -339.1964088526558498, -64.50000000000000000, 0.4999999999999543698 ) ) ;
#15600 = FACE_OUTER_BOUND ( 'NONE', #2893, .T. ) ;
#15601 = AXIS2_PLACEMENT_3D ( 'NONE', #14095, #22743, #39012 ) ;
#15603 = VECTOR ( 'NONE', #27035, 1000.000000000000000 ) ;
#15602 = DIRECTION ( 'NONE',  ( 0.000000000000000000, 0.000000000000000000, 1.000000000000000000 ) ) ;
#15604 = DIRECTION ( 'NONE',  ( -0.000000000000000000, 1.000000000000000000, -0.000000000000000000 ) ) ;
#15605 = VERTEX_POINT ( 'NONE', #28269 ) ;
#15606 = EDGE_LOOP ( 'NONE', ( #46827, #27308, #12813, #36436 ) ) ;
#15607 = ORIENTED_EDGE ( 'NONE', *, *, #19190, .T. ) ;
#15608 = VECTOR ( 'NONE', #4831, 1000.000000000000000 ) ;
#15609 = CARTESIAN_POINT ( 'NONE',  ( -332.3517673607765914, -178.6135371030394481, 23.71704087764532076 ) ) ;
#15610 = CARTESIAN_POINT ( 'NONE',  ( -109.9568094315246327, -183.6283474603465606, -108.8370090194290611 ) ) ;
#15611 = CARTESIAN_POINT ( 'NONE',  ( -336.3521761649654422, -74.01670616005314685, 32.17247266903214609 ) ) ;
#15612 = DIRECTION ( 'NONE',  ( -0.7765238627180349740, 0.000000000000000000, -0.6300878435817203194 ) ) ;
#15613 = PLANE ( 'NONE',  #22234 ) ;
#15614 = VERTEX_POINT ( 'NONE', #15425 ) ;
#15615 = CARTESIAN_POINT ( 'NONE',  ( 60.00000000000000000, -113.5000000000000000, -40.00000000000001421 ) ) ;
#15616 = DIRECTION ( 'NONE',  ( -0.000000000000000000, 1.000000000000000000, -0.000000000000000000 ) ) ;
#15617 = CARTESIAN_POINT ( 'NONE',  ( -336.3521761649654422, -160.6539403396202772, 45.90766452162722544 ) ) ;
#15618 = EDGE_LOOP ( 'NONE', ( #12451, #5064, #4583, #21271 ) ) ;
#15619 = ORIENTED_EDGE ( 'NONE', *, *, #26176, .F. ) ;
#15620 = VECTOR ( 'NONE', #19437, 1000.000000000000114 ) ;
#15621 = ORIENTED_EDGE ( 'NONE', *, *, #36259, .T. ) ;
#15622 = DIRECTION ( 'NONE',  ( -0.05924062789370748011, 0.000000000000000000, -0.9982437317643217956 ) ) ;
#15623 = CIRCLE ( 'NONE', #9769, 125.0000000000000000 ) ;
#15624 = CARTESIAN_POINT ( 'NONE',  ( -339.1964088526558498, -182.5000000000000568, 0.5000000000000457412 ) ) ;
#15625 = ORIENTED_EDGE ( 'NONE', *, *, #41967, .T. ) ;
#15626 = LINE ( 'NONE', #40032, #45875 ) ;
#15627 = AXIS2_PLACEMENT_3D ( 'NONE', #36548, #5298, #12634 ) ;
#15628 = FACE_OUTER_BOUND ( 'NONE', #8703, .T. ) ;
#15629 = ADVANCED_FACE ( 'NONE', ( #23809 ), #16193, .T. ) ;
#15630 = EDGE_CURVE ( 'NONE', #18239, #14029, #20122, .T. ) ;
#15631 = DIRECTION ( 'NONE',  ( 1.000000000000000000, 0.000000000000000000, -0.000000000000000000 ) ) ;
#15632 = ORIENTED_EDGE ( 'NONE', *, *, #27401, .F. ) ;
#15633 = DIRECTION ( 'NONE',  ( 0.000000000000000000, 0.000000000000000000, 1.000000000000000000 ) ) ;
#15634 = EDGE_LOOP ( 'NONE', ( #40731, #2770, #26377, #38656 ) ) ;
#15635 = FACE_OUTER_BOUND ( 'NONE', #19318, .T. ) ;
#15636 = CIRCLE ( 'NONE', #22346, 124.9999999999999858 ) ;
#15637 = DIRECTION ( 'NONE',  ( -0.7378332790417239107, 0.000000000000000000, -0.6749830015182142207 ) ) ;
#15638 = VERTEX_POINT ( 'NONE', #39819 ) ;
#15639 = SHAPE_REPRESENTATION ( 'Quick-Change Tool Holder Block', ( #31742 ), #35946 ) ;
#15640 = VECTOR ( 'NONE', #30890, 999.9999999999998863 ) ;
#15641 = CIRCLE ( 'NONE', #34207, 125.0000000000000000 ) ;
#15642 = DIRECTION ( 'NONE',  ( -0.000000000000000000, 1.000000000000000000, -0.000000000000000000 ) ) ;
#15643 = CARTESIAN_POINT ( 'NONE',  ( -332.3517673607765914, -77.59233547837267508, 37.15394033962009246 ) ) ;
#15644 = DIRECTION ( 'NONE',  ( -0.000000000000000000, 1.000000000000000000, -0.000000000000000000 ) ) ;
#15645 = EDGE_CURVE ( 'NONE', #25767, #31054, #27745, .T. ) ;
#15646 = VECTOR ( 'NONE', #11270, 1000.000000000000000 ) ;
#15647 = LINE ( 'NONE', #19069, #44199 ) ;
#15648 = EDGE_CURVE ( 'NONE', #25351, #4219, #8042, .T. ) ;
#15649 = VERTEX_POINT ( 'NONE', #19358 ) ;
#15651 = VECTOR ( 'NONE', #22481, 1000.000000000000114 ) ;
#15650 = CARTESIAN_POINT ( 'NONE',  ( -131.8938452225253855, -177.1207230881787780, 93.09664195018557109 ) ) ;
#15652 = VERTEX_POINT ( 'NONE', #23311 ) ;
#15653 = ORIENTED_EDGE ( 'NONE', *, *, #25660, .F. ) ;
#15654 = EDGE_CURVE ( 'NONE', #16440, #27371, #47990, .T. ) ;
#15655 = LINE ( 'NONE', #39790, #13425 ) ;
#15657 = ORIENTED_EDGE ( 'NONE', *, *, #30163, .F. ) ;
#15656 = DIRECTION ( 'NONE',  ( 0.000000000000000000, 0.000000000000000000, 1.000000000000000000 ) ) ;
#15658 = EDGE_CURVE ( 'NONE', #43736, #47366, #36442, .T. ) ;
#15659 = VERTEX_POINT ( 'NONE', #35370 ) ;
#15660 = DIRECTION ( 'NONE',  ( 1.043714542225393381E-14, 0.000000000000000000, -1.000000000000000000 ) ) ;
#15661 = CARTESIAN_POINT ( 'NONE',  ( 67.29469129333651267, -177.1207230881787780, -44.41421852208627996 ) ) ;
#15662 = CIRCLE ( 'NONE', #18172, 125.0000000000000000 ) ;
#15663 = VECTOR ( 'NONE', #22688, 1000.000000000000000 ) ;
#15664 = ORIENTED_EDGE ( 'NONE', *, *, #7396, .T. ) ;
#15665 = LINE ( 'NONE', #3825, #24254 ) ;
#15666 = CARTESIAN_POINT ( 'NONE',  ( -332.3517673607765914, -98.41210887299327226, -53.46519113769058151 ) ) ;
#15667 = VERTEX_POINT ( 'NONE', #48527 ) ;
#15668 = DIRECTION ( 'NONE',  ( 1.000000000000000000, -0.000000000000000000, -0.000000000000000000 ) ) ;
#15669 = CARTESIAN_POINT ( 'NONE',  ( 26.89923761108473954, -189.7472609257535510, -98.45863302693476271 ) ) ;
#15670 = VECTOR ( 'NONE', #556, 1000.000000000000000 ) ;
#15671 = LINE ( 'NONE', #3048, #69 ) ;
#15672 = CARTESIAN_POINT ( 'NONE',  ( -28.74596282265200387, -193.5000000000000000, 123.4325817657431230 ) ) ;
#15673 = ORIENTED_EDGE ( 'NONE', *, *, #35536, .T. ) ;
#15674 = EDGE_LOOP ( 'NONE', ( #1310, #15822, #759, #2806 ) ) ;
#15675 = ORIENTED_EDGE ( 'NONE', *, *, #11248, .T. ) ;
#15676 = DIRECTION ( 'NONE',  ( 1.000000000000000000, 0.000000000000000000, 0.000000000000000000 ) ) ;
#15677 = DIRECTION ( 'NONE',  ( 0.000000000000000000, 0.8660254037844354880, -0.5000000000000054401 ) ) ;
#15678 = AXIS2_PLACEMENT_3D ( 'NONE', #48523, #23547, #11445 ) ;
#15679 = CIRCLE ( 'NONE', #51767, 125.0000000000000000 ) ;
#15680 = PLANE ( 'NONE',  #49482 ) ;
#15681 = CIRCLE ( 'NONE', #29923, 10.00000000000000711 ) ;
#15683 = VECTOR ( 'NONE', #51907, 1000.000000000000227 ) ;
#15682 = FACE_OUTER_BOUND ( 'NONE', #1103, .T. ) ;
#15684 = CARTESIAN_POINT ( 'NONE',  ( -339.1964088526558498, -90.39567187580880159, -48.84008046109142498 ) ) ;
#15685 = ORIENTED_EDGE ( 'NONE', *, *, #11202, .T. ) ;
#15686 = VECTOR ( 'NONE', #35891, 1000.000000000000000 ) ;
#15687 = VECTOR ( 'NONE', #31052, 1000.000000000000114 ) ;
#15688 = CARTESIAN_POINT ( 'NONE',  ( -171.9128728525929262, -193.5000000000000000, 11.83705339977326965 ) ) ;
#15689 = ADVANCED_FACE ( 'NONE', ( #51428 ), #11453, .F. ) ;
#15690 = VERTEX_POINT ( 'NONE', #32209 ) ;
#15692 = EDGE_LOOP ( 'NONE', ( #48850, #26011, #4505, #41159 ) ) ;
#15691 = CARTESIAN_POINT ( 'NONE',  ( 0.000000000000000000, -175.7419055135392227, 27.41866715058277038 ) ) ;
#15693 = ORIENTED_EDGE ( 'NONE', *, *, #40425, .T. ) ;
#15694 = DIRECTION ( 'NONE',  ( -0.000000000000000000, 1.000000000000000000, 0.000000000000000000 ) ) ;
#15695 = CARTESIAN_POINT ( 'NONE',  ( -46.00000000000000711, 20.00000000000000000, -41.00000000000000000 ) ) ;
#15696 = ADVANCED_FACE ( 'NONE', ( #47472 ), #43532, .T. ) ;
#15697 = DIRECTION ( 'NONE',  ( -0.000000000000000000, -0.4647231720437604574, 0.8854560256532141294 ) ) ;
#15698 = EDGE_CURVE ( 'NONE', #15649, #4141, #34758, .T. ) ;
#15699 = ADVANCED_FACE ( 'NONE', ( #3574 ), #31696, .T. ) ;
#15700 = CARTESIAN_POINT ( 'NONE',  ( 45.66222513722991749, -183.6283474603465606, 80.70646587903453906 ) ) ;
#15701 = VERTEX_POINT ( 'NONE', #51951 ) ;
#15702 = DIRECTION ( 'NONE',  ( 0.000000000000000000, -0.000000000000000000, 1.000000000000000000 ) ) ;
#15703 = EDGE_CURVE ( 'NONE', #34344, #18494, #28003, .T. ) ;
#15704 = ORIENTED_EDGE ( 'NONE', *, *, #19424, .F. ) ;
#15705 = DIRECTION ( 'NONE',  ( -0.05924062789370006937, 0.000000000000000000, -0.9982437317643222396 ) ) ;
#15706 = VECTOR ( 'NONE', #3166, 1000.000000000000114 ) ;
#15707 = EDGE_CURVE ( 'NONE', #2833, #4101, #3733, .T. ) ;
#15708 = CARTESIAN_POINT ( 'NONE',  ( -152.8713435144644563, -177.1207230881787780, -68.75510947788596638 ) ) ;
#15709 = CARTESIAN_POINT ( 'NONE',  ( -339.1964088526558498, -123.5000000000000284, 0.000000000000000000 ) ) ;
#15710 = LINE ( 'NONE', #15449, #411 ) ;
#15711 = CIRCLE ( 'NONE', #6485, 125.0000000000000000 ) ;
#15712 = CARTESIAN_POINT ( 'NONE',  ( -332.3517673607765914, -123.5000000000000284, 0.000000000000000000 ) ) ;
#15713 = CARTESIAN_POINT ( 'NONE',  ( -180.0000000000000568, -155.0173647354142759, 14.76740078976490622 ) ) ;
#15714 = ADVANCED_FACE ( 'NONE', ( #20380 ), #12231, .F. ) ;
#15715 = VERTEX_POINT ( 'NONE', #32476 ) ;
#15716 = LINE ( 'NONE', #19637, #43114 ) ;
#15717 = LINE ( 'NONE', #32236, #13970 ) ;
#15718 = ADVANCED_FACE ( 'NONE', ( #12501 ), #20643, .T. ) ;
#15719 = FACE_BOUND ( 'NONE', #47162, .T. ) ;
#15720 = ORIENTED_EDGE ( 'NONE', *, *, #17963, .T. ) ;
#15721 = VECTOR ( 'NONE', #32139, 1000.000000000000000 ) ;
#15722 = ADVANCED_FACE ( 'NONE', ( #36680 ), #21422, .T. ) ;
#15723 = VECTOR ( 'NONE', #28962, 1000.000000000000114 ) ;
#15724 = CARTESIAN_POINT ( 'NONE',  ( -339.1964088526558498, -131.1080185721133660, -58.50955523165751515 ) ) ;
#15725 = AXIS2_PLACEMENT_3D ( 'NONE', #39445, #15049, #19477 ) ;
#15726 = AXIS2_PLACEMENT_3D ( 'NONE', #16092, #9247, #25269 ) ;
#15727 = FACE_OUTER_BOUND ( 'NONE', #29457, .T. ) ;
#15728 = EDGE_CURVE ( 'NONE', #13540, #30593, #25618, .T. ) ;
#15729 = ORIENTED_EDGE ( 'NONE', *, *, #43423, .F. ) ;
#15730 = LINE ( 'NONE', #31739, #43066 ) ;
#15731 = VECTOR ( 'NONE', #40231, 1000.000000000000114 ) ;
#15732 = EDGE_LOOP ( 'NONE', ( #35257, #38291, #24666, #18404 ) ) ;
#15733 = ADVANCED_FACE ( 'NONE', ( #29560 ), #13286, .T. ) ;
#15734 = VECTOR ( 'NONE', #17387, 1000.000000000000000 ) ;
#15735 = EDGE_CURVE ( 'NONE', #16447, #34175, #37189, .T. ) ;
#15736 = LINE ( 'NONE', #19394, #15891 ) ;
#15737 = FACE_BOUND ( 'NONE', #47342, .T. ) ;
#15739 = ORIENTED_EDGE ( 'NONE', *, *, #9829, .F. ) ;
#15738 = PLANE ( 'NONE',  #2768 ) ;
#15740 = LINE ( 'NONE', #30703, #5913 ) ;
#15741 = ADVANCED_FACE ( 'NONE', ( #13007 ), #5151, .T. ) ;
#15742 = ORIENTED_EDGE ( 'NONE', *, *, #641, .T. ) ;
#15743 = VERTEX_POINT ( 'NONE', #5674 ) ;
#15744 = CARTESIAN_POINT ( 'NONE',  ( -156.2577088867455473, -183.6283474603465606, -63.31490529818422885 ) ) ;
#15745 = VECTOR ( 'NONE', #41261, 1000.000000000000000 ) ;
#15746 = AXIS2_PLACEMENT_3D ( 'NONE', #31806, #20753, #44414 ) ;
#15747 = ORIENTED_EDGE ( 'NONE', *, *, #49983, .F. ) ;
#15748 = DIRECTION ( 'NONE',  ( 0.000000000000000000, 0.000000000000000000, 1.000000000000000000 ) ) ;
#15749 = CARTESIAN_POINT ( 'NONE',  ( -305.0000000000000568, -120.8677111499054320, 59.94223098458771659 ) ) ;
#15750 = CIRCLE ( 'NONE', #45123, 60.00000000000000000 ) ;
#15751 = DIRECTION ( 'NONE',  ( 1.000000000000000000, 7.719741424018497712E-17, 4.051632851310676353E-17 ) ) ;
#15752 = DIRECTION ( 'NONE',  ( 0.000000000000000000, 0.000000000000000000, -1.000000000000000000 ) ) ;
#15753 = ORIENTED_EDGE ( 'NONE', *, *, #47155, .F. ) ;
#15756 = ORIENTED_EDGE ( 'NONE', *, *, #6800, .F. ) ;
#15755 = CARTESIAN_POINT ( 'NONE',  ( -144.0067397530739584, -193.5000000000000000, -80.61932246194587037 ) ) ;
#15754 = CARTESIAN_POINT ( 'NONE',  ( -60.80616967713028487, -193.5000000000000000, -123.3865623328508292 ) ) ;
#15757 = AXIS2_PLACEMENT_3D ( 'NONE', #26437, #42470, #6495 ) ;
#15758 = VERTEX_POINT ( 'NONE', #32732 ) ;
#15759 = AXIS2_PLACEMENT_3D ( 'NONE', #21298, #26013, #41793 ) ;
#15760 = AXIS2_PLACEMENT_3D ( 'NONE', #32744, #16464, #36413 ) ;
#15761 = DIRECTION ( 'NONE',  ( -0.9785564922995046988, 0.000000000000000000, 0.2059786187410953262 ) ) ;
#15762 = ORIENTED_EDGE ( 'NONE', *, *, #51776, .T. ) ;
#15763 = CARTESIAN_POINT ( 'NONE',  ( 71.87891646118019651, -189.7472609257535510, -33.74820638215424395 ) ) ;
#15764 = ORIENTED_EDGE ( 'NONE', *, *, #17007, .T. ) ;
#15765 = ADVANCED_FACE ( 'NONE', ( #33521 ), #45614, .T. ) ;
#15766 = EDGE_CURVE ( 'NONE', #5824, #49603, #28516, .T. ) ;
#15767 = AXIS2_PLACEMENT_3D ( 'NONE', #13178, #13952, #1851 ) ;
#15768 = CARTESIAN_POINT ( 'NONE',  ( -151.9915035862630646, -177.1207230881787780, 70.07273251429430161 ) ) ;
#15769 = VERTEX_POINT ( 'NONE', #1455 ) ;
#15771 = LINE ( 'NONE', #31780, #47663 ) ;
#15770 = CARTESIAN_POINT ( 'NONE',  ( 71.15591247552652021, -177.1207230881787780, 36.22785377504034443 ) ) ;
#15772 = ORIENTED_EDGE ( 'NONE', *, *, #27825, .F. ) ;
#15773 = EDGE_CURVE ( 'NONE', #4130, #27476, #29036, .T. ) ;
#15774 = AXIS2_PLACEMENT_3D ( 'NONE', #47865, #36025, #15540 ) ;
#15775 = EDGE_CURVE ( 'NONE', #47743, #6051, #7089, .T. ) ;
#15776 = CARTESIAN_POINT ( 'NONE',  ( -332.3517673607765914, -166.5797264208035244, 40.34602258462248159 ) ) ;
#15777 = ORIENTED_EDGE ( 'NONE', *, *, #50380, .T. ) ;
#15778 = CARTESIAN_POINT ( 'NONE',  ( -339.1964088526558498, -65.36517161715286761, -14.84391218300986282 ) ) ;
#15779 = PLANE ( 'NONE',  #29034 ) ;
#15780 = CARTESIAN_POINT ( 'NONE',  ( -160.7804753152582293, -193.5000000000000000, -52.57768177182447999 ) ) ;
#15781 = CARTESIAN_POINT ( 'NONE',  ( 31.28129687248616619, -193.5000000000000000, 96.24590808611479531 ) ) ;
#15782 = CARTESIAN_POINT ( 'NONE',  ( -55.99477380783406488, -175.3837268820161057, 123.7720294769269742 ) ) ;
#15783 = LINE ( 'NONE', #36235, #13827 ) ;
#15784 = ORIENTED_EDGE ( 'NONE', *, *, #51886, .F. ) ;
#15785 = DIRECTION ( 'NONE',  ( 1.000000000000000000, 0.000000000000000000, 0.000000000000000000 ) ) ;
#15786 = CARTESIAN_POINT ( 'NONE',  ( -107.1845112550870027, -177.1207230881787780, 109.2239789693437331 ) ) ;
#15787 = CARTESIAN_POINT ( 'NONE',  ( 50.70030191143631981, -183.6283474603465606, -76.08180419845318454 ) ) ;
#15788 = ORIENTED_EDGE ( 'NONE', *, *, #572, .F. ) ;
#15789 = CIRCLE ( 'NONE', #25003, 125.0000000000000000 ) ;
#15790 = AXIS2_PLACEMENT_3D ( 'NONE', #28596, #44393, #44641 ) ;
#15791 = CARTESIAN_POINT ( 'NONE',  ( -50.83192613281184435, -183.6283474603465606, 123.9784823535113816 ) ) ;
#15792 = EDGE_CURVE ( 'NONE', #45794, #18389, #17506, .T. ) ;
#15793 = AXIS2_PLACEMENT_3D ( 'NONE', #35299, #31356, #50322 ) ;
#15794 = DIRECTION ( 'NONE',  ( -0.9890401873221654760, 0.000000000000000000, 0.1476465640024710868 ) ) ;
#15796 = VERTEX_POINT ( 'NONE', #4615 ) ;
#15795 = DIRECTION ( 'NONE',  ( -1.000000000000000000, -6.921107616850788183E-15, -7.812315528781864579E-15 ) ) ;
#15797 = ORIENTED_EDGE ( 'NONE', *, *, #20852, .T. ) ;
#15798 = ORIENTED_EDGE ( 'NONE', *, *, #45278, .T. ) ;
#15799 = ADVANCED_FACE ( 'NONE', ( #12744 ), #49560, .F. ) ;
#15800 = FACE_OUTER_BOUND ( 'NONE', #48587, .T. ) ;
#15801 = DIRECTION ( 'NONE',  ( -0.000000000000000000, 1.000000000000000000, -0.000000000000000000 ) ) ;
#15802 = CARTESIAN_POINT ( 'NONE',  ( -336.3521761649654422, -181.7525362123217292, 9.724760635742144999 ) ) ;
#15803 = ORIENTED_EDGE ( 'NONE', *, *, #38401, .F. ) ;
#15804 = CARTESIAN_POINT ( 'NONE',  ( -48.47912675150885065, -175.3837268820161057, 6.938893903907228378E-15 ) ) ;
#15805 = CIRCLE ( 'NONE', #33394, 125.0000000000000000 ) ;
#15806 = ORIENTED_EDGE ( 'NONE', *, *, #26390, .T. ) ;
#15807 = EDGE_LOOP ( 'NONE', ( #35191, #40838, #11017, #28298 ) ) ;
#15808 = ORIENTED_EDGE ( 'NONE', *, *, #25015, .F. ) ;
#15809 = DIRECTION ( 'NONE',  ( -0.8294056854502011022, 0.000000000000000000, -0.5586467658036535777 ) ) ;
#15810 = VERTEX_POINT ( 'NONE', #9090 ) ;
#15811 = SURFACE_STYLE_USAGE ( .BOTH. , #44690 ) ;
#15812 = DIRECTION ( 'NONE',  ( 0.000000000000000000, 0.000000000000000000, 1.000000000000000000 ) ) ;
#15815 = VERTEX_POINT ( 'NONE', #33248 ) ;
#15814 = CARTESIAN_POINT ( 'NONE',  ( -339.1964088526558498, -109.8658467157464571, 57.40522506028071348 ) ) ;
#15813 = LINE ( 'NONE', #48649, #11546 ) ;
#15816 = AXIS2_PLACEMENT_3D ( 'NONE', #43792, #11735, #23824 ) ;
#15817 = AXIS2_PLACEMENT_3D ( 'NONE', #44959, #24987, #1587 ) ;
#15818 = LINE ( 'NONE', #39686, #9677 ) ;
#15819 = ORIENTED_EDGE ( 'NONE', *, *, #20503, .F. ) ;
#15820 = DIRECTION ( 'NONE',  ( 1.043714542225393381E-14, 0.8854560256532141294, 0.4647231720437604574 ) ) ;
#15821 = CIRCLE ( 'NONE', #11602, 125.0000000000000000 ) ;
#15822 = ORIENTED_EDGE ( 'NONE', *, *, #3341, .T. ) ;
#15823 = EDGE_CURVE ( 'NONE', #45342, #41076, #41643, .T. ) ;
#15824 = DIRECTION ( 'NONE',  ( -0.6749830015182091136, 0.000000000000000000, -0.7378332790417285736 ) ) ;
#15825 = DIRECTION ( 'NONE',  ( 0.000000000000000000, -0.6631226582407885317, 0.7485107481711069655 ) ) ;
#15827 = PLANE ( 'NONE',  #49181 ) ;
#15826 = DIRECTION ( 'NONE',  ( 0.000000000000000000, 1.000000000000000000, 0.000000000000000000 ) ) ;
#15828 = ORIENTED_EDGE ( 'NONE', *, *, #15279, .F. ) ;
#15829 = AXIS2_PLACEMENT_3D ( 'NONE', #3258, #35298, #35547 ) ;
#15830 = PLANE ( 'NONE',  #42451 ) ;
#15831 = CARTESIAN_POINT ( 'NONE',  ( -180.0000000000000568, -130.6726371812771959, 60.00000000000000711 ) ) ;
#15832 = LINE ( 'NONE', #23687, #11593 ) ;
#15833 = ORIENTED_EDGE ( 'NONE', *, *, #2683, .F. ) ;
#15834 = DIRECTION ( 'NONE',  ( -0.8858462335218260097, 0.000000000000000000, -0.4639789333096864810 ) ) ;
#15835 = CARTESIAN_POINT ( 'NONE',  ( -144.6608085595393618, -189.7472609257535510, -78.26291788638665992 ) ) ;
#15836 = CARTESIAN_POINT ( 'NONE',  ( 43.33156026654913262, 30.00000000000000355, -51.04247435516399634 ) ) ;
#15837 = EDGE_LOOP ( 'NONE', ( #36953, #10545, #6490, #50522 ) ) ;
#15838 = CARTESIAN_POINT ( 'NONE',  ( -330.4913330509368166, -79.66942718702493664, 39.49849221029193558 ) ) ;
#15839 = DIRECTION ( 'NONE',  ( -8.718379230999707126E-17, -0.9927088740980551940, -0.1205366802553130001 ) ) ;
#15840 = AXIS2_PLACEMENT_3D ( 'NONE', #7848, #23377, #39891 ) ;
#15841 = EDGE_LOOP ( 'NONE', ( #15756, #6659, #49520, #3561 ) ) ;
#15842 = PLANE ( 'NONE',  #34983 ) ;
#15843 = ORIENTED_EDGE ( 'NONE', *, *, #8609, .F. ) ;
#15844 = DIRECTION ( 'NONE',  ( -1.000000000000000000, 0.000000000000000000, 0.000000000000000000 ) ) ;
#15845 = CARTESIAN_POINT ( 'NONE',  ( -330.4913330509368166, -65.36517161715264024, 14.84391218300897286 ) ) ;
#15846 = EDGE_CURVE ( 'NONE', #25260, #4153, #25371, .T. ) ;
#15847 = DIRECTION ( 'NONE',  ( 0.9785564922995017012, 0.000000000000000000, 0.2059786187411094538 ) ) ;
#15848 = CARTESIAN_POINT ( 'NONE',  ( -63.09433862318514485, -189.7472609257535510, -124.1426420773539547 ) ) ;
#15849 = FACE_OUTER_BOUND ( 'NONE', #5362, .T. ) ;
#15850 = CARTESIAN_POINT ( 'NONE',  ( -161.2555905272863868, -189.7472609257535510, -53.91167979418499812 ) ) ;
#15851 = AXIS2_PLACEMENT_3D ( 'NONE', #7371, #19194, #47313 ) ;
#15852 = CIRCLE ( 'NONE', #7445, 125.0000000000000000 ) ;
#15853 = CARTESIAN_POINT ( 'NONE',  ( -170.0502155641509319, -193.5000000000000000, -29.07697310430878090 ) ) ;
#15854 = CARTESIAN_POINT ( 'NONE',  ( -48.98765787015805984, -175.3837268820161057, -0.8610436117673551104 ) ) ;
#15856 = EDGE_LOOP ( 'NONE', ( #38289, #26196, #40511, #10296 ) ) ;
#15855 = LINE ( 'NONE', #42912, #25362 ) ;
#15857 = AXIS2_PLACEMENT_3D ( 'NONE', #13925, #2079, #50971 ) ;
#15858 = ORIENTED_EDGE ( 'NONE', *, *, #18488, .T. ) ;
#15859 = LINE ( 'NONE', #19772, #36666 ) ;
#15860 = ADVANCED_FACE ( 'NONE', ( #44822 ), #13539, .F. ) ;
#15861 = DIRECTION ( 'NONE',  ( 0.000000000000000000, 1.000000000000000000, 0.000000000000000000 ) ) ;
#15862 = ORIENTED_EDGE ( 'NONE', *, *, #21158, .T. ) ;
#15863 = AXIS2_PLACEMENT_3D ( 'NONE', #1234, #33310, #13341 ) ;
#15864 = VERTEX_POINT ( 'NONE', #37968 ) ;
#15865 = EDGE_LOOP ( 'NONE', ( #3453, #39294, #4544, #109 ) ) ;
#15866 = CARTESIAN_POINT ( 'NONE',  ( -48.47912675150885065, -173.5000000000000284, 6.938893903907228378E-15 ) ) ;
#15867 = DIRECTION ( 'NONE',  ( 0.000000000000000000, -0.9709418174260527890, -0.2393156642875547968 ) ) ;
#15868 = CARTESIAN_POINT ( 'NONE',  ( -48.59739992243020623, -183.6283474603465606, -0.9929810960135115883 ) ) ;
#15869 = LINE ( 'NONE', #26898, #17424 ) ;
#15870 = ORIENTED_EDGE ( 'NONE', *, *, #25942, .F. ) ;
#15871 = ORIENTED_EDGE ( 'NONE', *, *, #7398, .T. ) ;
#15872 = VERTEX_POINT ( 'NONE', #46387 ) ;
#15873 = AXIS2_PLACEMENT_3D ( 'NONE', #11471, #15176, #11212 ) ;
#15874 = EDGE_CURVE ( 'NONE', #18957, #11444, #24712, .T. ) ;
#15875 = CARTESIAN_POINT ( 'NONE',  ( -158.3442440847886985, -189.7472609257535510, -59.62093586438118109 ) ) ;
#15876 = FACE_OUTER_BOUND ( 'NONE', #5125, .T. ) ;
#15877 = DIRECTION ( 'NONE',  ( -0.000000000000000000, 1.000000000000000000, -0.000000000000000000 ) ) ;
#15878 = DIRECTION ( 'NONE',  ( 0.000000000000000000, 0.8229838658936596829, 0.5680647467311510379 ) ) ;
#15879 = CARTESIAN_POINT ( 'NONE',  ( -339.1964088526558498, -79.66942718702553350, -39.49849221029258928 ) ) ;
#15880 = EDGE_LOOP ( 'NONE', ( #8923, #19583, #40599, #44234 ) ) ;
#15881 = DIRECTION ( 'NONE',  ( -0.6528221181905280446, 0.000000000000000000, 0.7575112421616145841 ) ) ;
#15882 = EDGE_CURVE ( 'NONE', #17543, #37732, #28900, .T. ) ;
#15883 = DIRECTION ( 'NONE',  ( -0.000000000000000000, 1.000000000000000000, -0.000000000000000000 ) ) ;
#15884 = CARTESIAN_POINT ( 'NONE',  ( 47.70255505652112049, -193.5000000000000000, 78.26291788638732783 ) ) ;
#15885 = ORIENTED_EDGE ( 'NONE', *, *, #28871, .T. ) ;
#15886 = ORIENTED_EDGE ( 'NONE', *, *, #46606, .T. ) ;
#15887 = EDGE_CURVE ( 'NONE', #51600, #46293, #22718, .T. ) ;
#15888 = ORIENTED_EDGE ( 'NONE', *, *, #16504, .F. ) ;
#15889 = DIRECTION ( 'NONE',  ( 1.000000000000000000, -0.000000000000000000, -0.000000000000000000 ) ) ;
#15891 = VECTOR ( 'NONE', #2593, 1000.000000000000000 ) ;
#15890 = DIRECTION ( 'NONE',  ( 0.000000000000000000, 0.000000000000000000, 1.000000000000000000 ) ) ;
#15892 = ORIENTED_EDGE ( 'NONE', *, *, #793, .F. ) ;
#15893 = CARTESIAN_POINT ( 'NONE',  ( -336.3521761649654422, -87.81784868886214213, 47.06073758877343494 ) ) ;
#15894 = VECTOR ( 'NONE', #34086, 1000.000000000000000 ) ;
#15895 = DIRECTION ( 'NONE',  ( 0.000000000000000000, 0.9350162426854169428, 0.3546048870425300148 ) ) ;
#15896 = LINE ( 'NONE', #47943, #38554 ) ;
#15897 = EDGE_LOOP ( 'NONE', ( #21217, #38064, #44738, #463 ) ) ;
#15898 = DIRECTION ( 'NONE',  ( -0.000000000000000000, -0.3546048870425267951, 0.9350162426854181641 ) ) ;
#15899 = ORIENTED_EDGE ( 'NONE', *, *, #25451, .T. ) ;
#15900 = CARTESIAN_POINT ( 'NONE',  ( -48.47912675150885065, -183.6283474603465606, 6.938893903907228378E-15 ) ) ;
#15901 = DIRECTION ( 'NONE',  ( 0.000000000000000000, 0.8660254037844354880, -0.5000000000000054401 ) ) ;
#15902 = FACE_BOUND ( 'NONE', #6274, .T. ) ;
#15903 = LINE ( 'NONE', #47950, #42854 ) ;
#15904 = EDGE_CURVE ( 'NONE', #978, #32381, #30335, .T. ) ;
#15905 = EDGE_LOOP ( 'NONE', ( #4974, #43713, #28809, #52005 ) ) ;
#15906 = DIRECTION ( 'NONE',  ( 0.000000000000000000, 1.000000000000000000, -0.000000000000000000 ) ) ;
#15907 = CYLINDRICAL_SURFACE ( 'NONE', #24703, 125.0000000000000000 ) ;
#15908 = FACE_OUTER_BOUND ( 'NONE', #43207, .T. ) ;
#15909 = DIRECTION ( 'NONE',  ( 0.4566292373937140270, 0.000000000000000000, -0.8896570909947467687 ) ) ;
#15910 = AXIS2_PLACEMENT_3D ( 'NONE', #10784, #6326, #10510 ) ;
#15911 = ORIENTED_EDGE ( 'NONE', *, *, #19299, .T. ) ;
#15912 = DIRECTION ( 'NONE',  ( 0.3758275821142292861, 0.000000000000000000, 0.9266896074318371479 ) ) ;
#15913 = ORIENTED_EDGE ( 'NONE', *, *, #5081, .T. ) ;
#15914 = ORIENTED_EDGE ( 'NONE', *, *, #33546, .T. ) ;
#15915 = CARTESIAN_POINT ( 'NONE',  ( -330.4913330509368166, -115.8919814278871598, -58.50955523165758621 ) ) ;
#15917 = ORIENTED_EDGE ( 'NONE', *, *, #7691, .F. ) ;
#15916 = DIRECTION ( 'NONE',  ( 0.000000000000000000, -0.000000000000000000, -1.000000000000000000 ) ) ;
#15918 = VERTEX_POINT ( 'NONE', #50846 ) ;
#15919 = CARTESIAN_POINT ( 'NONE',  ( -330.4913330509368166, -168.0775241366801254, -40.16023333900968595 ) ) ;
#15920 = CARTESIAN_POINT ( 'NONE',  ( -170.6250538923603131, -189.7472609257535510, 26.55884942729649723 ) ) ;
#15921 = VERTEX_POINT ( 'NONE', #10114 ) ;
#15922 = AXIS2_PLACEMENT_3D ( 'NONE', #723, #31988, #24132 ) ;
#15923 = PLANE ( 'NONE',  #5825 ) ;
#15924 = DIRECTION ( 'NONE',  ( 1.000000000000000000, 0.000000000000000000, -0.000000000000000000 ) ) ;
#15925 = ORIENTED_EDGE ( 'NONE', *, *, #46546, .F. ) ;
#15926 = CARTESIAN_POINT ( 'NONE',  ( -336.3521761649654422, -169.4076645216271402, -37.15394033962039089 ) ) ;
#15927 = DIRECTION ( 'NONE',  ( -0.9929810960135185827, 0.000000000000000000, 0.1182731709213523247 ) ) ;
#15928 = CIRCLE ( 'NONE', #27656, 124.9999999999999858 ) ;
#15929 = EDGE_CURVE ( 'NONE', #12643, #38136, #49898, .T. ) ;
#15930 = EDGE_CURVE ( 'NONE', #8565, #18537, #22200, .T. ) ;
#15931 = CARTESIAN_POINT ( 'NONE',  ( -336.3521761649654422, -85.59754891220836726, -45.24454186338619621 ) ) ;
#15932 = FACE_OUTER_BOUND ( 'NONE', #2195, .T. ) ;
#15933 = ORIENTED_EDGE ( 'NONE', *, *, #39410, .T. ) ;
#15934 = ORIENTED_EDGE ( 'NONE', *, *, #27608, .F. ) ;
#15935 = EDGE_LOOP ( 'NONE', ( #35080, #30105, #47072, #38597 ) ) ;
#15936 = CARTESIAN_POINT ( 'NONE',  ( -169.2746641285359317, -189.7472609257535510, -32.14713283941905786 ) ) ;
#15937 = DIRECTION ( 'NONE',  ( -0.5085311186492273983, 0.000000000000000000, 0.8610436117673514467 ) ) ;
#15938 = PLANE ( 'NONE',  #25124 ) ;
#15939 = DIRECTION ( 'NONE',  ( -0.000000000000000000, -1.000000000000000000, 0.000000000000000000 ) ) ;
#15940 = CARTESIAN_POINT ( 'NONE',  ( -336.3521761649654422, -173.5513585866778214, -31.34948880313881503 ) ) ;
#15941 = VERTEX_POINT ( 'NONE', #46134 ) ;
#15942 = ADVANCED_FACE ( 'NONE', ( #19040 ), #50074, .T. ) ;
#15943 = EDGE_CURVE ( 'NONE', #32738, #42284, #22202, .T. ) ;
#15944 = AXIS2_PLACEMENT_3D ( 'NONE', #13590, #13343, #33311 ) ;
#15945 = DIRECTION ( 'NONE',  ( 0.000000000000000000, 0.000000000000000000, 1.000000000000000000 ) ) ;
#15946 = ORIENTED_EDGE ( 'NONE', *, *, #39419, .T. ) ;
#15947 = APPLICATION_CONTEXT ( 'automotive_design' ) ;
#15949 = VERTEX_POINT ( 'NONE', #34290 ) ;
#15948 = FACE_OUTER_BOUND ( 'NONE', #37680, .T. ) ;
#15950 = VERTEX_POINT ( 'NONE', #2998 ) ;
#15951 = EDGE_CURVE ( 'NONE', #38828, #4817, #2737, .T. ) ;
#15952 = LINE ( 'NONE', #44568, #32494 ) ;
#15953 = DIRECTION ( 'NONE',  ( 0.000000000000000000, 0.000000000000000000, 1.000000000000000000 ) ) ;
#15954 = EDGE_CURVE ( 'NONE', #9440, #14212, #42162, .T. ) ;
#15955 = CARTESIAN_POINT ( 'NONE',  ( -47.50057025920934706, -177.1207230881787780, 0.2059786187411091207 ) ) ;
#15956 = DIRECTION ( 'NONE',  ( 0.000000000000000000, -0.9927088740980556381, -0.1205366802553095307 ) ) ;
#15957 = EDGE_LOOP ( 'NONE', ( #20090, #13280, #10656, #30798 ) ) ;
#15958 = CARTESIAN_POINT ( 'NONE',  ( -330.4913330509368166, -183.0001959263614424, -7.728304129924260302 ) ) ;
#15959 = ORIENTED_EDGE ( 'NONE', *, *, #32729, .F. ) ;
#15960 = ORIENTED_EDGE ( 'NONE', *, *, #1154, .T. ) ;
#15961 = DIRECTION ( 'NONE',  ( -0.000000000000000000, 1.000000000000000000, -0.000000000000000000 ) ) ;
#15962 = AXIS2_PLACEMENT_3D ( 'NONE', #6353, #22374, #9071 ) ;
#15963 = PLANE ( 'NONE',  #33709 ) ;
#15964 = CARTESIAN_POINT ( 'NONE',  ( 75.01583293582058332, -193.5000000000000000, 11.18012358327990086 ) ) ;
#15965 = DIRECTION ( 'NONE',  ( 0.3482016354343928088, 0.000000000000000000, 0.9374196611341231167 ) ) ;
#15966 = CARTESIAN_POINT ( 'NONE',  ( -48.71401279728982558, -193.5000000000000000, -0.9720229140804069745 ) ) ;
#15967 = LINE ( 'NONE', #44066, #15312 ) ;
#15968 = ORIENTED_EDGE ( 'NONE', *, *, #31518, .F. ) ;
#15969 = DIRECTION ( 'NONE',  ( 0.4216675885939766832, 0.4327645661435912672, 0.7968131995768455988 ) ) ;
#15970 = CARTESIAN_POINT ( 'NONE',  ( 10.73478887071927623, -193.5000000000000000, -110.0850225811106924 ) ) ;
#15971 = FACE_BOUND ( 'NONE', #37143, .T. ) ;
#15972 = EDGE_LOOP ( 'NONE', ( #30147, #17389, #41203, #33955 ) ) ;
#15973 = CARTESIAN_POINT ( 'NONE',  ( -336.3521761649654422, -105.0395444947681369, -56.09938080879045685 ) ) ;
#15974 = CARTESIAN_POINT ( 'NONE',  ( -336.3521761649653854, -84.94915232962709695, -45.97643030831888211 ) ) ;
#15975 = ORIENTED_EDGE ( 'NONE', *, *, #11875, .F. ) ;
#15976 = FACE_OUTER_BOUND ( 'NONE', #25481, .T. ) ;
#15977 = ORIENTED_EDGE ( 'NONE', *, *, #22114, .T. ) ;
#15978 = AXIS2_PLACEMENT_3D ( 'NONE', #13474, #9530, #48959 ) ;
#15979 = AXIS2_PLACEMENT_3D ( 'NONE', #45768, #41825, #6343 ) ;
#15980 = LINE ( 'NONE', #20423, #1668 ) ;
#15981 = FACE_BOUND ( 'NONE', #29639, .T. ) ;
#15983 = ORIENTED_EDGE ( 'NONE', *, *, #18329, .F. ) ;
#15982 = CARTESIAN_POINT ( 'NONE',  ( -73.94077438226447896, -177.1207230881787780, 122.3793467049372481 ) ) ;
#15984 = EDGE_CURVE ( 'NONE', #17851, #16442, #30866, .T. ) ;
#15985 = EDGE_CURVE ( 'NONE', #46519, #33480, #12082, .T. ) ;
#15986 = EDGE_CURVE ( 'NONE', #47167, #13896, #12959, .T. ) ;
#15987 = LINE ( 'NONE', #8861, #25221 ) ;
#15988 = ORIENTED_EDGE ( 'NONE', *, *, #33037, .T. ) ;
#15989 = EDGE_CURVE ( 'NONE', #29431, #41564, #21943, .T. ) ;
#15990 = VERTEX_POINT ( 'NONE', #30587 ) ;
#15991 = LINE ( 'NONE', #15744, #47751 ) ;
#15992 = AXIS2_PLACEMENT_3D ( 'NONE', #34078, #2011, #9913 ) ;
#15993 = ORIENTED_EDGE ( 'NONE', *, *, #24893, .F. ) ;
#15994 = ADVANCED_FACE ( 'NONE', ( #46909 ), #14320, .F. ) ;
#15995 = DIRECTION ( 'NONE',  ( -0.6965510290629982615, 0.000000000000000000, 0.7175072570443298270 ) ) ;
#15996 = EDGE_CURVE ( 'NONE', #8921, #18649, #9603, .T. ) ;
#15997 = LINE ( 'NONE', #15749, #6227 ) ;
#15998 = EDGE_CURVE ( 'NONE', #42041, #33417, #45867, .T. ) ;
#15999 = EDGE_CURVE ( 'NONE', #43044, #36835, #46598, .T. ) ;
#16000 = FILL_AREA_STYLE ('',( #32007 ) ) ;
#16001 = DIRECTION ( 'NONE',  ( -0.1768902751225666370, 0.000000000000000000, -0.9842305779475979399 ) ) ;
#16002 = VERTEX_POINT ( 'NONE', #48187 ) ;
#16005 = ORIENTED_EDGE ( 'NONE', *, *, #14398, .F. ) ;
#16004 = DIRECTION ( 'NONE',  ( -0.4031234292879600778, 0.000000000000000000, -0.9151456172430237901 ) ) ;
#16003 = CARTESIAN_POINT ( 'NONE',  ( 1.663811650136608034, -175.3837268820161057, -113.4093733337827530 ) ) ;
#16006 = ORIENTED_EDGE ( 'NONE', *, *, #22337, .T. ) ;
#16007 = ADVANCED_FACE ( 'NONE', ( #27160 ), #16128, .F. ) ;
#16008 = FACE_OUTER_BOUND ( 'NONE', #42048, .T. ) ;
#16009 = ORIENTED_EDGE ( 'NONE', *, *, #28184, .F. ) ;
#16010 = DIRECTION ( 'NONE',  ( -0.000000000000000000, 1.000000000000000000, -0.000000000000000000 ) ) ;
#16011 = EDGE_LOOP ( 'NONE', ( #41207, #50333, #13476, #31775 ) ) ;
#16012 = EDGE_CURVE ( 'NONE', #779, #19842, #7123, .T. ) ;
#16013 = DIRECTION ( 'NONE',  ( 0.000000000000000000, 0.000000000000000000, 1.000000000000000000 ) ) ;
#16014 = EDGE_LOOP ( 'NONE', ( #21462, #47819, #11915, #40011 ) ) ;
#16016 = CARTESIAN_POINT ( 'NONE',  ( -339.1964088526558498, -116.8846903019852164, -58.63009191191289915 ) ) ;
#16015 = DIRECTION ( 'NONE',  ( 0.000000000000000000, 1.000000000000000000, 0.000000000000000000 ) ) ;
#16017 = EDGE_LOOP ( 'NONE', ( #6138, #43422, #12330, #12347 ) ) ;
#16018 = AXIS2_PLACEMENT_3D ( 'NONE', #46834, #46320, #10821 ) ;
#16019 = CIRCLE ( 'NONE', #29423, 125.0000000000000000 ) ;
#16020 = ORIENTED_EDGE ( 'NONE', *, *, #36138, .T. ) ;
#16021 = CARTESIAN_POINT ( 'NONE',  ( -36.09284319799462537, -193.5000000000000000, 124.3848060646152618 ) ) ;
#16022 = DIRECTION ( 'NONE',  ( -0.7765238627180393038, 0.000000000000000000, -0.6300878435817147682 ) ) ;
#16023 = LINE ( 'NONE', #27313, #47364 ) ;
#16024 = FACE_OUTER_BOUND ( 'NONE', #30012, .T. ) ;
#16025 = DIRECTION ( 'NONE',  ( 6.978251959525016136E-17, 0.000000000000000000, 1.000000000000000000 ) ) ;
#16026 = DIRECTION ( 'NONE',  ( 0.000000000000000000, 0.9350162426854181641, 0.3546048870425267951 ) ) ;
#16027 = ORIENTED_EDGE ( 'NONE', *, *, #38177, .F. ) ;
#16028 = CARTESIAN_POINT ( 'NONE',  ( -48.47912675150885065, -183.6283474603465606, 6.938893903907228378E-15 ) ) ;
#16029 = ADVANCED_FACE ( 'NONE', ( #19541 ), #15357, .F. ) ;
#16030 = LINE ( 'NONE', #12057, #15620 ) ;
#16031 = DIRECTION ( 'NONE',  ( -0.000000000000000000, -0.1205366802553268363, -0.9927088740980534176 ) ) ;
#16032 = ORIENTED_EDGE ( 'NONE', *, *, #5257, .F. ) ;
#16033 = VECTOR ( 'NONE', #41379, 1000.000000000000000 ) ;
#16034 = CARTESIAN_POINT ( 'NONE',  ( -171.5592422664403216, -183.6283474603465606, -21.82395850507258928 ) ) ;
#16035 = DIRECTION ( 'NONE',  ( 0.000000000000000000, 0.000000000000000000, 1.000000000000000000 ) ) ;
#16036 = DIRECTION ( 'NONE',  ( 0.9646355819083576311, 0.000000000000000000, 0.2635871660690715101 ) ) ;
#16037 = ORIENTED_EDGE ( 'NONE', *, *, #19576, .T. ) ;
#16038 = VERTEX_POINT ( 'NONE', #39751 ) ;
#16039 = VERTEX_POINT ( 'NONE', #15109 ) ;
#16040 = EDGE_CURVE ( 'NONE', #19079, #7467, #36087, .T. ) ;
#16041 = CARTESIAN_POINT ( 'NONE',  ( -48.47912675150885065, -189.7472609257535510, 6.938893903907228378E-15 ) ) ;
#16042 = FACE_OUTER_BOUND ( 'NONE', #21506, .T. ) ;
#16043 = PLANE ( 'NONE',  #36289 ) ;
#16044 = CARTESIAN_POINT ( 'NONE',  ( -154.2693405752510500, -175.3837268820161057, 66.58401203837830451 ) ) ;
#16045 = TOROIDAL_SURFACE ( 'NONE', #45424, 9.000000000000000000, 2.000000000000000000 ) ;
#16046 = VERTEX_POINT ( 'NONE', #27424 ) ;
#16047 = ADVANCED_FACE ( 'NONE', ( #47161, #39507 ), #43196, .F. ) ;
#16048 = EDGE_CURVE ( 'NONE', #3432, #150, #26428, .T. ) ;
#16049 = EDGE_CURVE ( 'NONE', #16791, #25116, #44242, .T. ) ;
#16050 = CARTESIAN_POINT ( 'NONE',  ( 2.246147418155142628, 51.04815051713691076, -20.95336071107404408 ) ) ;
#16051 = VERTEX_POINT ( 'NONE', #8235 ) ;
#16052 = ADVANCED_FACE ( 'NONE', ( #83 ), #15613, .T. ) ;
#16053 = AXIS2_PLACEMENT_3D ( 'NONE', #10862, #6920, #26107 ) ;
#16054 = EDGE_LOOP ( 'NONE', ( #39383, #40702, #19248, #46009 ) ) ;
#16055 = EDGE_LOOP ( 'NONE', ( #25884, #30517, #1840, #21311 ) ) ;
#16056 = ORIENTED_EDGE ( 'NONE', *, *, #32905, .F. ) ;
#16057 = CARTESIAN_POINT ( 'NONE',  ( -336.3521761649654422, -178.0871407151310279, 22.44790492310219676 ) ) ;
#16058 = ADVANCED_FACE ( 'NONE', ( #43718 ), #3271, .T. ) ;
#16059 = ORIENTED_EDGE ( 'NONE', *, *, #5927, .F. ) ;
#16060 = DIRECTION ( 'NONE',  ( 0.000000000000000000, -1.000000000000000000, 0.000000000000000000 ) ) ;
#16061 = CARTESIAN_POINT ( 'NONE',  ( -339.1964088526558498, -66.33409060400673241, -14.60509510167901404 ) ) ;
#16064 = VERTEX_POINT ( 'NONE', #11661 ) ;
#16063 = CARTESIAN_POINT ( 'NONE',  ( -106.4764934152196645, -213.5000000000000000, 110.7307791902283043 ) ) ;
#16062 = DIRECTION ( 'NONE',  ( 0.000000000000000000, 0.000000000000000000, -1.000000000000000000 ) ) ;
#16065 = CIRCLE ( 'NONE', #10166, 124.9999999999999858 ) ;
#16066 = ADVANCED_FACE ( 'NONE', ( #23745 ), #47408, .T. ) ;
#16067 = DIRECTION ( 'NONE',  ( 0.000000000000000000, 1.000000000000000000, 0.000000000000000000 ) ) ;
#16068 = ORIENTED_EDGE ( 'NONE', *, *, #51189, .F. ) ;
#16069 = DIRECTION ( 'NONE',  ( 0.000000000000000000, -1.000000000000000000, 0.000000000000000000 ) ) ;
#16070 = ORIENTED_EDGE ( 'NONE', *, *, #40606, .F. ) ;
#16071 = EDGE_CURVE ( 'NONE', #5652, #45186, #23497, .T. ) ;
#16072 = CARTESIAN_POINT ( 'NONE',  ( -109.5001801941309196, -177.1207230881787780, -107.9473519284343297 ) ) ;
#16073 = CARTESIAN_POINT ( 'NONE',  ( -16.77927958806650821, -177.1207230881787780, -120.9136869416130082 ) ) ;
#16075 = LINE ( 'NONE', #20261, #27357 ) ;
#16074 = CARTESIAN_POINT ( 'NONE',  ( -339.1964088526558498, -180.6659093959932250, 14.60509510167942437 ) ) ;
#16076 = VERTEX_POINT ( 'NONE', #11905 ) ;
#16077 = EDGE_CURVE ( 'NONE', #15270, #11472, #24269, .T. ) ;
#16078 = DIRECTION ( 'NONE',  ( -0.9993203489176063492, 0.000000000000000000, -0.03686245026030392224 ) ) ;
#16079 = DIRECTION ( 'NONE',  ( -0.000000000000000000, 0.000000000000000000, 1.000000000000000000 ) ) ;
#16080 = VERTEX_POINT ( 'NONE', #4043 ) ;
#16081 = LINE ( 'NONE', #20015, #40871 ) ;
#16082 = DIRECTION ( 'NONE',  ( 0.000000000000000000, 1.000000000000000000, -0.000000000000000000 ) ) ;
#16083 = VECTOR ( 'NONE', #4862, 1000.000000000000000 ) ;
#16084 = DIRECTION ( 'NONE',  ( -0.000000000000000000, 1.000000000000000000, 0.000000000000000000 ) ) ;
#16085 = ORIENTED_EDGE ( 'NONE', *, *, #8288, .F. ) ;
#16086 = CARTESIAN_POINT ( 'NONE',  ( 141.7825277784304205, -193.5000000000000000, -9.999999999999987566 ) ) ;
#16087 = VECTOR ( 'NONE', #15446, 1000.000000000000000 ) ;
#16088 = DIRECTION ( 'NONE',  ( 0.000000000000000000, 0.1205366802553130001, -0.9927088740980551940 ) ) ;
#16089 = AXIS2_PLACEMENT_3D ( 'NONE', #43633, #40200, #47068 ) ;
#16090 = EDGE_CURVE ( 'NONE', #48687, #3778, #20060, .T. ) ;
#16091 = ORIENTED_EDGE ( 'NONE', *, *, #37513, .T. ) ;
#16092 = CARTESIAN_POINT ( 'NONE',  ( -48.47912675150885065, -189.7472609257535510, 6.938893903907228378E-15 ) ) ;
#16093 = ORIENTED_EDGE ( 'NONE', *, *, #20694, .F. ) ;
#16094 = CARTESIAN_POINT ( 'NONE',  ( 58.12687231399078058, -177.1207230881787780, -63.33473559879913495 ) ) ;
#16095 = FACE_OUTER_BOUND ( 'NONE', #25982, .T. ) ;
#16096 = CARTESIAN_POINT ( 'NONE',  ( -330.4913330509368166, -122.9999999999994600, 59.00000000000002132 ) ) ;
#16097 = DIRECTION ( 'NONE',  ( 0.000000000000000000, 1.000000000000000000, -0.000000000000000000 ) ) ;
#16098 = DIRECTION ( 'NONE',  ( -0.9646355819083594074, 0.000000000000000000, 0.2635871660690647933 ) ) ;
#16099 = CIRCLE ( 'NONE', #30339, 60.00000000000000000 ) ;
#16100 = PLANE ( 'NONE',  #26291 ) ;
#16101 = AXIS2_PLACEMENT_3D ( 'NONE', #10422, #45412, #29881 ) ;
#16102 = PLANE ( 'NONE',  #1821 ) ;
#16103 = LINE ( 'NONE', #32117, #12111 ) ;
#16105 = ORIENTED_EDGE ( 'NONE', *, *, #40394, .T. ) ;
#16104 = DIRECTION ( 'NONE',  ( 0.9995608365087942371, 0.000000000000000000, 0.02963332782256331357 ) ) ;
#16106 = ORIENTED_EDGE ( 'NONE', *, *, #24142, .T. ) ;
#16107 = EDGE_CURVE ( 'NONE', #31330, #26846, #20544, .T. ) ;
#16108 = ADVANCED_FACE ( 'NONE', ( #36609 ), #45297, .T. ) ;
#16109 = DIRECTION ( 'NONE',  ( -0.000000000000000000, 0.2393156642875685636, 0.9709418174260492362 ) ) ;
#16110 = CARTESIAN_POINT ( 'NONE',  ( -48.47912675150885065, -175.3837268820161057, 6.938893903907228378E-15 ) ) ;
#16111 = ORIENTED_EDGE ( 'NONE', *, *, #51330, .F. ) ;
#16112 = ORIENTED_EDGE ( 'NONE', *, *, #14285, .T. ) ;
#16113 = ORIENTED_EDGE ( 'NONE', *, *, #11829, .F. ) ;
#16114 = CARTESIAN_POINT ( 'NONE',  ( 76.04209377433249983, -189.7472609257535510, -10.93003379476865611 ) ) ;
#16115 = PLANE ( 'NONE',  #43460 ) ;
#16116 = DIRECTION ( 'NONE',  ( 0.000000000000000000, 0.000000000000000000, 1.000000000000000000 ) ) ;
#16117 = DIRECTION ( 'NONE',  ( 0.000000000000000000, -1.000000000000000000, 0.000000000000000000 ) ) ;
#16118 = VECTOR ( 'NONE', #27967, 1000.000000000000000 ) ;
#16119 = ORIENTED_EDGE ( 'NONE', *, *, #4162, .T. ) ;
#16120 = ORIENTED_EDGE ( 'NONE', *, *, #17371, .F. ) ;
#16122 = ORIENTED_EDGE ( 'NONE', *, *, #34270, .T. ) ;
#16121 = VECTOR ( 'NONE', #13911, 1000.000000000000000 ) ;
#16123 = CARTESIAN_POINT ( 'NONE',  ( -116.2964108826154330, -177.1207230881787780, -105.0038855142073260 ) ) ;
#16124 = CARTESIAN_POINT ( 'NONE',  ( -336.3521761649654422, -104.1045282520827300, -55.74477592174792306 ) ) ;
#16125 = CARTESIAN_POINT ( 'NONE',  ( -23.01747912075234836, -177.1207230881787780, -122.3793467049370634 ) ) ;
#16126 = ADVANCED_FACE ( 'NONE', ( #32911 ), #9535, .T. ) ;
#16127 = FACE_OUTER_BOUND ( 'NONE', #41458, .T. ) ;
#16128 = PLANE ( 'NONE',  #39849 ) ;
#16129 = VERTEX_POINT ( 'NONE', #29244 ) ;
#16130 = CARTESIAN_POINT ( 'NONE',  ( 9.518239912201957864, -193.5000000000000000, -110.7307791902283043 ) ) ;
#16131 = DIRECTION ( 'NONE',  ( -0.000000000000000000, 0.9709418174260519008, -0.2393156642875582940 ) ) ;
#16132 = CARTESIAN_POINT ( 'NONE',  ( -48.47912675150885065, -175.3837268820161057, -0.9999999999999931166 ) ) ;
#16133 = CARTESIAN_POINT ( 'NONE',  ( -155.4465502054561057, -193.5000000000000000, 64.67588669375881238 ) ) ;
#16134 = AXIS2_PLACEMENT_3D ( 'NONE', #46618, #41359, #21922 ) ;
#16135 = EDGE_CURVE ( 'NONE', #7602, #37376, #9279, .T. ) ;
#16136 = EDGE_LOOP ( 'NONE', ( #34409, #2072, #46061, #31449 ) ) ;
#16137 = ORIENTED_EDGE ( 'NONE', *, *, #45313, .T. ) ;
#16138 = VECTOR ( 'NONE', #2052, 1000.000000000000000 ) ;
#16139 = ORIENTED_EDGE ( 'NONE', *, *, #44534, .T. ) ;
#16140 = VECTOR ( 'NONE', #40017, 1000.000000000000227 ) ;
#16141 = DIRECTION ( 'NONE',  ( -1.000000000000000000, -9.241633304753541364E-15, 4.850383327711987764E-15 ) ) ;
#16142 = CARTESIAN_POINT ( 'NONE',  ( -98.71382891444395113, -189.7472609257535510, -114.4616734920523555 ) ) ;
#16143 = ORIENTED_EDGE ( 'NONE', *, *, #35795, .F. ) ;
#16144 = CARTESIAN_POINT ( 'NONE',  ( -78.64590280292341617, -175.3837268820161057, -121.3052580173827408 ) ) ;
#16145 = PLANE ( 'NONE',  #29589 ) ;
#16146 = PLANE ( 'NONE',  #20936 ) ;
#16147 = VERTEX_POINT ( 'NONE', #16660 ) ;
#16148 = PLANE ( 'NONE',  #22571 ) ;
#16149 = VERTEX_POINT ( 'NONE', #17441 ) ;
#16150 = CARTESIAN_POINT ( 'NONE',  ( -332.3517673607765914, -120.8677111499054320, 59.00000000000000000 ) ) ;
#16151 = ORIENTED_EDGE ( 'NONE', *, *, #368, .T. ) ;
#16152 = CARTESIAN_POINT ( 'NONE',  ( -48.47912675150885065, -183.6283474603465606, 6.938893903907228378E-15 ) ) ;
#16153 = DIRECTION ( 'NONE',  ( -1.000000000000000000, 0.000000000000000000, 0.000000000000000000 ) ) ;
#16154 = CARTESIAN_POINT ( 'NONE',  ( -170.0000000000000284, -123.5000000000000284, -37.63467731922663972 ) ) ;
#16155 = EDGE_LOOP ( 'NONE', ( #27323, #27827, #30679, #24615 ) ) ;
#16156 = AXIS2_PLACEMENT_3D ( 'NONE', #16021, #480, #23883 ) ;
#16157 = CARTESIAN_POINT ( 'NONE',  ( 34.23904069044534992, -177.1207230881787780, -92.37913469314065651 ) ) ;
#16158 = PLANE ( 'NONE',  #45723 ) ;
#16159 = DIRECTION ( 'NONE',  ( 0.000000000000000000, 0.000000000000000000, 1.000000000000000000 ) ) ;
#16160 = DIRECTION ( 'NONE',  ( -0.5586467658036476935, 0.000000000000000000, -0.8294056854502049880 ) ) ;
#16161 = AXIS2_PLACEMENT_3D ( 'NONE', #19453, #35474, #8 ) ;
#16162 = ORIENTED_EDGE ( 'NONE', *, *, #42993, .T. ) ;
#16163 = DIRECTION ( 'NONE',  ( 0.000000000000000000, 0.1205366802553164696, -0.9927088740980548609 ) ) ;
#16164 = EDGE_LOOP ( 'NONE', ( #32733, #25933, #16343, #35072 ) ) ;
#16165 = ORIENTED_EDGE ( 'NONE', *, *, #42216, .T. ) ;
#16167 = VERTEX_POINT ( 'NONE', #29488 ) ;
#16166 = DIRECTION ( 'NONE',  ( -0.000000000000000000, 0.4647231720437664526, -0.8854560256532110207 ) ) ;
#16168 = ORIENTED_EDGE ( 'NONE', *, *, #29045, .T. ) ;
#16169 = FACE_OUTER_BOUND ( 'NONE', #37959, .T. ) ;
#16170 = EDGE_CURVE ( 'NONE', #29802, #25337, #32398, .T. ) ;
#16171 = CIRCLE ( 'NONE', #45552, 125.0000000000000000 ) ;
#16172 = VECTOR ( 'NONE', #19811, 1000.000000000000000 ) ;
#16173 = LINE ( 'NONE', #32189, #40241 ) ;
#16174 = ADVANCED_FACE ( 'NONE', ( #24515 ), #44499, .T. ) ;
#16175 = AXIS2_PLACEMENT_3D ( 'NONE', #10861, #41887, #9834 ) ;
#16176 = VERTEX_POINT ( 'NONE', #605 ) ;
#16177 = CARTESIAN_POINT ( 'NONE',  ( -339.1964088526558498, -182.5000000000000568, 0.5000000000000457412 ) ) ;
#16178 = DIRECTION ( 'NONE',  ( 0.000000000000000000, -1.000000000000000000, 0.000000000000000000 ) ) ;
#16179 = ORIENTED_EDGE ( 'NONE', *, *, #43345, .T. ) ;
#16180 = LINE ( 'NONE', #28504, #10713 ) ;
#16181 = CYLINDRICAL_SURFACE ( 'NONE', #46810, 125.0000000000000000 ) ;
#16182 = ADVANCED_FACE ( 'NONE', ( #16388 ), #45032, .F. ) ;
#16183 = DIRECTION ( 'NONE',  ( 0.000000000000000000, 0.5680647467311569221, 0.8229838658936556861 ) ) ;
#16184 = PLANE ( 'NONE',  #20697 ) ;
#16185 = ORIENTED_EDGE ( 'NONE', *, *, #40859, .T. ) ;
#16186 = VERTEX_POINT ( 'NONE', #25552 ) ;
#16187 = VERTEX_POINT ( 'NONE', #20577 ) ;
#16188 = CARTESIAN_POINT ( 'NONE',  ( -29.73468717939733708, -177.1207230881787780, 123.5865930638410930 ) ) ;
#16189 = CARTESIAN_POINT ( 'NONE',  ( 8.750818922897904528, -175.3837268820161057, -111.1293539894138434 ) ) ;
#16190 = EDGE_CURVE ( 'NONE', #30709, #30058, #28703, .T. ) ;
#16191 = DIRECTION ( 'NONE',  ( -1.000000000000000000, 0.000000000000000000, 0.000000000000000000 ) ) ;
#16192 = FACE_BOUND ( 'NONE', #4163, .T. ) ;
#16193 = PLANE ( 'NONE',  #45703 ) ;
#16194 = AXIS2_PLACEMENT_3D ( 'NONE', #42179, #41931, #26149 ) ;
#16195 = ORIENTED_EDGE ( 'NONE', *, *, #46202, .F. ) ;
#16196 = VECTOR ( 'NONE', #37571, 1000.000000000000000 ) ;
#16197 = ORIENTED_EDGE ( 'NONE', *, *, #48142, .F. ) ;
#16199 = ORIENTED_EDGE ( 'NONE', *, *, #48156, .F. ) ;
#16198 = FACE_OUTER_BOUND ( 'NONE', #46233, .T. ) ;
#16200 = ORIENTED_EDGE ( 'NONE', *, *, #25634, .F. ) ;
#16201 = CARTESIAN_POINT ( 'NONE',  ( -47.82630463331833681, -193.5000000000000000, 0.7575112421616305713 ) ) ;
#16202 = CARTESIAN_POINT ( 'NONE',  ( -339.1964088526558498, -66.09477493971917283, -13.63415328425296202 ) ) ;
#16203 = DIRECTION ( 'NONE',  ( 0.9266896074318343723, 0.000000000000000000, -0.3758275821142357809 ) ) ;
#16204 = CARTESIAN_POINT ( 'NONE',  ( -305.0000000000000568, -125.1322888500942554, -59.97779283292990016 ) ) ;
#16205 = ORIENTED_EDGE ( 'NONE', *, *, #240, .F. ) ;
#16206 = DIRECTION ( 'NONE',  ( -0.000000000000000000, 1.047444401652940007E-14, 1.000000000000000000 ) ) ;
#16207 = CIRCLE ( 'NONE', #4463, 125.0000000000000000 ) ;
#16208 = ORIENTED_EDGE ( 'NONE', *, *, #37307, .F. ) ;
#16209 = VECTOR ( 'NONE', #189, 1000.000000000000000 ) ;
#16210 = VERTEX_POINT ( 'NONE', #48709 ) ;
#16211 = FACE_OUTER_BOUND ( 'NONE', #34744, .T. ) ;
#16212 = AXIS2_PLACEMENT_3D ( 'NONE', #51329, #3240, #4014 ) ;
#16213 = LINE ( 'NONE', #7801, #50497 ) ;
#16214 = LINE ( 'NONE', #8832, #33245 ) ;
#16215 = LINE ( 'NONE', #51704, #37372 ) ;
#16216 = EDGE_CURVE ( 'NONE', #50565, #36650, #19712, .T. ) ;
#16217 = FACE_OUTER_BOUND ( 'NONE', #118, .T. ) ;
#16218 = DIRECTION ( 'NONE',  ( 0.6068001458185945385, 0.000000000000000000, -0.7948544414133523750 ) ) ;
#16219 = VECTOR ( 'NONE', #45142, 1000.000000000000000 ) ;
#16220 = ORIENTED_EDGE ( 'NONE', *, *, #30492, .T. ) ;
#16221 = CARTESIAN_POINT ( 'NONE',  ( 34.23904069044534992, -193.5000000000000000, -92.37913469314065651 ) ) ;
#16222 = DIRECTION ( 'NONE',  ( -1.000000000000000000, -0.000000000000000000, -0.000000000000000000 ) ) ;
#16223 = ADVANCED_FACE ( 'NONE', ( #13478 ), #44760, .T. ) ;
#16224 = FACE_BOUND ( 'NONE', #15043, .T. ) ;
#16225 = ORIENTED_EDGE ( 'NONE', *, *, #43260, .T. ) ;
#16226 = CARTESIAN_POINT ( 'NONE',  ( -40.90423906728908321, -193.5000000000000000, -124.7702732086912221 ) ) ;
#16227 = AXIS2_PLACEMENT_3D ( 'NONE', #51008, #22623, #18676 ) ;
#16228 = CARTESIAN_POINT ( 'NONE',  ( 43.33156026654913262, 35.00000000000000000, -51.04247435516399634 ) ) ;
#16229 = ORIENTED_EDGE ( 'NONE', *, *, #34748, .T. ) ;
#16230 = DIRECTION ( 'NONE',  ( 0.000000000000000000, 1.000000000000000000, 0.000000000000000000 ) ) ;
#16231 = EDGE_CURVE ( 'NONE', #48776, #44261, #17221, .T. ) ;
#16232 = ORIENTED_EDGE ( 'NONE', *, *, #39261, .T. ) ;
#16233 = EDGE_CURVE ( 'NONE', #36797, #5120, #14701, .T. ) ;
#16234 = AXIS2_PLACEMENT_3D ( 'NONE', #17426, #847, #30008 ) ;
#16235 = LINE ( 'NONE', #32247, #10888 ) ;
#16236 = EDGE_CURVE ( 'NONE', #23376, #5997, #33180, .T. ) ;
#16237 = DIRECTION ( 'NONE',  ( -0.000000000000000000, 1.000000000000000000, -0.000000000000000000 ) ) ;
#16239 = VERTEX_POINT ( 'NONE', #36345 ) ;
#16238 = CARTESIAN_POINT ( 'NONE',  ( -336.3521761649654422, -160.6539403396202772, 45.90766452162722544 ) ) ;
#16241 = AXIS2_PLACEMENT_3D ( 'NONE', #36034, #3708, #51822 ) ;
#16240 = CARTESIAN_POINT ( 'NONE',  ( -60.00000000000000000, 20.00000000000000000, 60.00000000000000711 ) ) ;
#16242 = ORIENTED_EDGE ( 'NONE', *, *, #14421, .T. ) ;
#16243 = ORIENTED_EDGE ( 'NONE', *, *, #47155, .T. ) ;
#16244 =( REPRESENTATION_RELATIONSHIP ('NONE','NONE', #4578, #33452 ) REPRESENTATION_RELATIONSHIP_WITH_TRANSFORMATION ( #13629 )SHAPE_REPRESENTATION_RELATIONSHIP( ) );
#16245 = CARTESIAN_POINT ( 'NONE',  ( -172.4465090799742484, -193.5000000000000000, -2.844930291600638927 ) ) ;
#16246 = AXIS2_PLACEMENT_3D ( 'NONE', #37007, #36755, #32805 ) ;
#16247 = VERTEX_POINT ( 'NONE', #337 ) ;
#16248 = DIRECTION ( 'NONE',  ( 0.000000000000000000, 0.000000000000000000, -1.000000000000000000 ) ) ;
#16249 = CARTESIAN_POINT ( 'NONE',  ( 6.443011874827243801, -177.1207230881787780, 112.2878385610370771 ) ) ;
#16250 = DIRECTION ( 'NONE',  ( 0.000000000000000000, -1.000000000000000000, 0.000000000000000000 ) ) ;
#16251 = CARTESIAN_POINT ( 'NONE',  ( -339.1964088526558498, -89.57268800991437274, 48.27201571435973904 ) ) ;
#16252 = VERTEX_POINT ( 'NONE', #5083 ) ;
#16254 = ORIENTED_EDGE ( 'NONE', *, *, #43336, .F. ) ;
#16253 = LINE ( 'NONE', #4423, #24165 ) ;
#16255 = ORIENTED_EDGE ( 'NONE', *, *, #7857, .T. ) ;
#16256 = CARTESIAN_POINT ( 'NONE',  ( -339.1964088526558498, -172.3400804610910200, 33.10432812419180948 ) ) ;
#16257 = VERTEX_POINT ( 'NONE', #49228 ) ;
#16258 = DIRECTION ( 'NONE',  ( 0.000000000000000000, 1.000000000000000000, 0.000000000000000000 ) ) ;
#16259 = AXIS2_PLACEMENT_3D ( 'NONE', #16815, #37023, #8907 ) ;
#16260 = ORIENTED_EDGE ( 'NONE', *, *, #37951, .T. ) ;
#16261 = DIRECTION ( 'NONE',  ( -0.3202698538628350744, 0.000000000000000000, -0.9473263538541923934 ) ) ;
#16262 = EDGE_LOOP ( 'NONE', ( #33238, #14160, #32442, #37099 ) ) ;
#16264 = DIRECTION ( 'NONE',  ( -0.000000000000000000, 1.000000000000000000, -0.000000000000000000 ) ) ;
#16263 = CYLINDRICAL_SURFACE ( 'NONE', #24089, 125.0000000000000000 ) ;
#16265 = ORIENTED_EDGE ( 'NONE', *, *, #39151, .T. ) ;
#16266 = AXIS2_PLACEMENT_3D ( 'NONE', #42341, #30263, #6866 ) ;
#16267 = ORIENTED_EDGE ( 'NONE', *, *, #25688, .F. ) ;
#16268 = DIRECTION ( 'NONE',  ( 0.5829794791144650157, 0.000000000000000000, 0.8124868780056864193 ) ) ;
#16269 = LINE ( 'NONE', #40176, #41606 ) ;
#16270 = PLANE ( 'NONE',  #14613 ) ;
#16271 = CARTESIAN_POINT ( 'NONE',  ( -142.6204786402482512, -177.1207230881787780, -80.70646587903382851 ) ) ;
#16272 = DIRECTION ( 'NONE',  ( -0.8124868780056742068, 0.000000000000000000, -0.5829794791144820021 ) ) ;
#16273 = CARTESIAN_POINT ( 'NONE',  ( -4.176930889631405464, -189.7472609257535510, 116.8859077982279615 ) ) ;
#16274 = EDGE_CURVE ( 'NONE', #11192, #8568, #30623, .T. ) ;
#16275 = VERTEX_POINT ( 'NONE', #41318 ) ;
#16276 = EDGE_CURVE ( 'NONE', #21483, #30086, #5344, .T. ) ;
#16277 = PRODUCT_CONTEXT ( 'NONE', #18627, 'mechanical' ) ;
#16278 = AXIS2_PLACEMENT_3D ( 'NONE', #29100, #8875, #17803 ) ;
#16279 = CARTESIAN_POINT ( 'NONE',  ( -120.2975302769383177, -177.1207230881787780, 102.3089288139534005 ) ) ;
#16280 = CARTESIAN_POINT ( 'NONE',  ( -12.13476221271688615, -193.5000000000000000, 119.5996955107804638 ) ) ;
#16281 = CARTESIAN_POINT ( 'NONE',  ( -49.38192458147459263, -183.6283474603465606, -0.4300652022765235616 ) ) ;
#16282 = ORIENTED_EDGE ( 'NONE', *, *, #18717, .F. ) ;
#16283 = CYLINDRICAL_SURFACE ( 'NONE', #38267, 125.0000000000000000 ) ;
#16284 = EDGE_CURVE ( 'NONE', #24073, #9161, #2672, .T. ) ;
#16285 = DIRECTION ( 'NONE',  ( -0.000000000000000000, 1.000000000000000000, -0.000000000000000000 ) ) ;
#16286 = CARTESIAN_POINT ( 'NONE',  ( 1.352451982137491404, -189.7472609257535510, 113.5465278748096978 ) ) ;
#16287 = ORIENTED_EDGE ( 'NONE', *, *, #40464, .F. ) ;
#16288 = ORIENTED_EDGE ( 'NONE', *, *, #12180, .T. ) ;
#16289 = ADVANCED_FACE ( 'NONE', ( #30795 ), #21631, .T. ) ;
#16290 = VERTEX_POINT ( 'NONE', #13736 ) ;
#16291 = EDGE_CURVE ( 'NONE', #3877, #21100, #38147, .T. ) ;
#16292 = DIRECTION ( 'NONE',  ( 0.000000000000000000, -0.000000000000000000, 1.000000000000000000 ) ) ;
#16293 = EDGE_CURVE ( 'NONE', #19975, #35261, #2081, .T. ) ;
#16294 = CARTESIAN_POINT ( 'NONE',  ( -330.4913330509368166, -167.3305728129743102, 39.49849221029282376 ) ) ;
#16295 = DIRECTION ( 'NONE',  ( 0.000000000000000000, 0.000000000000000000, 1.000000000000000000 ) ) ;
#16296 = CARTESIAN_POINT ( 'NONE',  ( -14.28570516517293854, -183.6283474603465606, 120.2323164553486521 ) ) ;
#16297 = CIRCLE ( 'NONE', #9586, 125.0000000000000000 ) ;
#16298 = ADVANCED_FACE ( 'NONE', ( #50271 ), #30278, .T. ) ;
#16299 = ORIENTED_EDGE ( 'NONE', *, *, #21789, .F. ) ;
#16300 = VECTOR ( 'NONE', #51255, 1000.000000000000000 ) ;
#16301 = CARTESIAN_POINT ( 'NONE',  ( -336.3521761649654422, -64.73342574900661361, 5.491276508483657892 ) ) ;
#16302 = VERTEX_POINT ( 'NONE', #34727 ) ;
#16303 = VECTOR ( 'NONE', #9624, 1000.000000000000000 ) ;
#16304 = ORIENTED_EDGE ( 'NONE', *, *, #11223, .T. ) ;
#16305 = VERTEX_POINT ( 'NONE', #41853 ) ;
#16306 = CARTESIAN_POINT ( 'NONE',  ( -117.6201219941651601, -175.3837268820161057, 104.1370384486469760 ) ) ;
#16308 = EDGE_LOOP ( 'NONE', ( #30950, #25816, #30903, #15397 ) ) ;
#16307 = VECTOR ( 'NONE', #49297, 1000.000000000000000 ) ;
#16309 = CARTESIAN_POINT ( 'NONE',  ( 141.7825277784304205, -213.5000000000000000, 41.45482488023466772 ) ) ;
#16310 = LINE ( 'NONE', #5019, #16844 ) ;
#16311 = ADVANCED_FACE ( 'NONE', ( #6374 ), #38671, .F. ) ;
#16314 = VERTEX_POINT ( 'NONE', #1902 ) ;
#16313 = CARTESIAN_POINT ( 'NONE',  ( -48.47912675150885065, -177.1207230881787780, 6.938893903907228378E-15 ) ) ;
#16312 = CARTESIAN_POINT ( 'NONE',  ( -305.0000000000000568, -87.28260048324004572, 47.83617848703421771 ) ) ;
#16315 = DIRECTION ( 'NONE',  ( -0.5085311186492154079, 0.000000000000000000, -0.8610436117673585521 ) ) ;
#16316 = VERTEX_POINT ( 'NONE', #22400 ) ;
#16317 = CARTESIAN_POINT ( 'NONE',  ( -332.3517673607765914, -101.0520950768976149, 54.58714071513087873 ) ) ;
#16318 = ORIENTED_EDGE ( 'NONE', *, *, #7688, .T. ) ;
#16319 = LINE ( 'NONE', #17572, #49295 ) ;
#16320 = DIRECTION ( 'NONE',  ( 0.000000000000000000, -0.2393156642875448881, 0.9709418174260553425 ) ) ;
#16322 = FACE_OUTER_BOUND ( 'NONE', #7486, .T. ) ;
#16321 = DIRECTION ( 'NONE',  ( 0.000000000000000000, 0.000000000000000000, -1.000000000000000000 ) ) ;
#16323 = VERTEX_POINT ( 'NONE', #18204 ) ;
#16324 = EDGE_CURVE ( 'NONE', #9367, #14713, #38424, .T. ) ;
#16325 = LINE ( 'NONE', #12632, #30748 ) ;
#16326 = DIRECTION ( 'NONE',  ( 0.2635871660690715101, 0.000000000000000000, -0.9646355819083576311 ) ) ;
#16327 = DIRECTION ( 'NONE',  ( -0.7378332790417189146, 0.000000000000000000, -0.6749830015182196608 ) ) ;
#16328 = ORIENTED_EDGE ( 'NONE', *, *, #3625, .T. ) ;
#16329 = DIRECTION ( 'NONE',  ( 0.9890401873221644768, 0.000000000000000000, -0.1476465640024779702 ) ) ;
#16330 = LINE ( 'NONE', #28661, #49214 ) ;
#16331 = AXIS2_PLACEMENT_3D ( 'NONE', #49443, #4758, #33119 ) ;
#16332 = CARTESIAN_POINT ( 'NONE',  ( -332.3517673607765914, -182.5000000000000568, 2.632288850093980503 ) ) ;
#16333 = VECTOR ( 'NONE', #44475, 1000.000000000000114 ) ;
#16334 = EDGE_CURVE ( 'NONE', #5462, #6625, #25569, .T. ) ;
#16335 = EDGE_CURVE ( 'NONE', #32062, #24955, #29749, .T. ) ;
#16336 = EDGE_CURVE ( 'NONE', #35575, #51281, #10827, .T. ) ;
#16337 = EDGE_LOOP ( 'NONE', ( #24412, #51647, #36115, #24336 ) ) ;
#16338 = EDGE_CURVE ( 'NONE', #18266, #24476, #45801, .T. ) ;
#16339 = DIRECTION ( 'NONE',  ( -0.000000000000000000, 1.000000000000000000, -0.000000000000000000 ) ) ;
#16341 = AXIS2_PLACEMENT_3D ( 'NONE', #8513, #40304, #31914 ) ;
#16340 = DIRECTION ( 'NONE',  ( 1.000000000000000000, -4.952603889764075929E-17, -7.175085443855059889E-17 ) ) ;
#16342 = EDGE_CURVE ( 'NONE', #5990, #6703, #45730, .T. ) ;
#16343 = ORIENTED_EDGE ( 'NONE', *, *, #4453, .T. ) ;
#16344 = CARTESIAN_POINT ( 'NONE',  ( -48.47912675150885065, -188.5000000000000284, -14.99999999999999289 ) ) ;
#16345 = EDGE_LOOP ( 'NONE', ( #28620, #8242, #43659, #21417 ) ) ;
#16346 = DIRECTION ( 'NONE',  ( 0.000000000000000000, 0.000000000000000000, -1.000000000000000000 ) ) ;
#16347 = EDGE_CURVE ( 'NONE', #39780, #26611, #21887, .T. ) ;
#16348 = FACE_OUTER_BOUND ( 'NONE', #962, .T. ) ;
#16349 = PLANE ( 'NONE',  #8420 ) ;
#16350 = DIRECTION ( 'NONE',  ( 0.000000000000000000, 0.000000000000000000, 1.000000000000000000 ) ) ;
#16351 = CARTESIAN_POINT ( 'NONE',  ( -332.3517673607765914, -66.60506506233235768, -15.70448169564047092 ) ) ;
#16352 = EDGE_CURVE ( 'NONE', #29838, #38530, #46578, .T. ) ;
#16353 = AXIS2_PLACEMENT_3D ( 'NONE', #37904, #30024, #9796 ) ;
#16354 = ADVANCED_FACE ( 'NONE', ( #26333 ), #18458, .T. ) ;
#16355 = LINE ( 'NONE', #29217, #3628 ) ;
#16356 = ADVANCED_FACE ( 'NONE', ( #14782 ), #42626, .T. ) ;
#16357 = LINE ( 'NONE', #32370, #40399 ) ;
#16358 = CARTESIAN_POINT ( 'NONE',  ( -63.43218022845230308, -189.7472609257535510, 124.1024020384604540 ) ) ;
#16360 = VERTEX_POINT ( 'NONE', #3703 ) ;
#16359 = CARTESIAN_POINT ( 'NONE',  ( -147.8383830610225971, -193.5000000000000000, -74.18852968774183410 ) ) ;
#16361 = ADVANCED_FACE ( 'NONE', ( #43132 ), #31045, .F. ) ;
#16362 = ORIENTED_EDGE ( 'NONE', *, *, #10157, .T. ) ;
#16363 = PLANE ( 'NONE',  #5663 ) ;
#16364 = EDGE_CURVE ( 'NONE', #3547, #44417, #15529, .T. ) ;
#16365 = LINE ( 'NONE', #51587, #46437 ) ;
#16366 = EDGE_LOOP ( 'NONE', ( #17521, #51341, #38510, #35389 ) ) ;
#16367 = ORIENTED_EDGE ( 'NONE', *, *, #36926, .F. ) ;
#16368 = CIRCLE ( 'NONE', #5465, 60.00000000000000000 ) ;
#16369 = VERTEX_POINT ( 'NONE', #51817 ) ;
#16370 = DIRECTION ( 'NONE',  ( -0.000000000000000000, -0.3546048870425396182, -0.9350162426854132791 ) ) ;
#16371 = CIRCLE ( 'NONE', #44924, 14.36509618646847386 ) ;
#16372 = AXIS2_PLACEMENT_3D ( 'NONE', #19633, #19378, #51451 ) ;
#16373 = DIRECTION ( 'NONE',  ( -0.4031234292879792847, 0.000000000000000000, 0.9151456172430153524 ) ) ;
#16374 = DIRECTION ( 'NONE',  ( -0.1768902751225733261, 0.000000000000000000, 0.9842305779475966077 ) ) ;
#16375 = ORIENTED_EDGE ( 'NONE', *, *, #7084, .T. ) ;
#16376 = ORIENTED_EDGE ( 'NONE', *, *, #50725, .T. ) ;
#16377 = EDGE_CURVE ( 'NONE', #32161, #33399, #47093, .T. ) ;
#16378 = VECTOR ( 'NONE', #437, 1000.000000000000000 ) ;
#16379 = ORIENTED_EDGE ( 'NONE', *, *, #39268, .T. ) ;
#16380 = EDGE_CURVE ( 'NONE', #32293, #50764, #17262, .T. ) ;
#16381 = CARTESIAN_POINT ( 'NONE',  ( -162.4844509910036550, -193.5000000000000000, -48.77484799213890909 ) ) ;
#16382 = LINE ( 'NONE', #858, #20165 ) ;
#16384 = VERTEX_POINT ( 'NONE', #7900 ) ;
#16383 = FACE_OUTER_BOUND ( 'NONE', #27636, .T. ) ;
#16385 = CIRCLE ( 'NONE', #43194, 125.0000000000000000 ) ;
#16386 = CARTESIAN_POINT ( 'NONE',  ( -171.4559849729830603, -177.1207230881787780, 22.39848972532369942 ) ) ;
#16387 = AXIS2_PLACEMENT_3D ( 'NONE', #5659, #34276, #10355 ) ;
#16388 = FACE_OUTER_BOUND ( 'NONE', #15483, .T. ) ;
#16389 = EDGE_LOOP ( 'NONE', ( #47542, #21581, #33637, #15213 ) ) ;
#16390 = DIRECTION ( 'NONE',  ( -0.8294056854502011022, 0.000000000000000000, -0.5586467658036535777 ) ) ;
#16391 = CARTESIAN_POINT ( 'NONE',  ( -160.0666658415768211, -193.5000000000000000, 54.07611884703389649 ) ) ;
#16392 = AXIS2_PLACEMENT_3D ( 'NONE', #25763, #10245, #30467 ) ;
#16393 = DIRECTION ( 'NONE',  ( 0.000000000000000000, 1.000000000000000000, 0.000000000000000000 ) ) ;
#16394 = LINE ( 'NONE', #43979, #35811 ) ;
#16395 = AXIS2_PLACEMENT_3D ( 'NONE', #4489, #524, #24988 ) ;
#16396 = ORIENTED_EDGE ( 'NONE', *, *, #38803, .F. ) ;
#16397 = VERTEX_POINT ( 'NONE', #22912 ) ;
#16398 = VERTEX_POINT ( 'NONE', #38925 ) ;
#16399 = PLANE ( 'NONE',  #20602 ) ;
#16400 = CYLINDRICAL_SURFACE ( 'NONE', #13259, 124.9999999999999858 ) ;
#16401 = ORIENTED_EDGE ( 'NONE', *, *, #5473, .F. ) ;
#16402 = CARTESIAN_POINT ( 'NONE',  ( -48.47912675150885065, -183.6283474603465606, 6.938893903907228378E-15 ) ) ;
#16403 = LINE ( 'NONE', #28981, #7759 ) ;
#16404 = EDGE_CURVE ( 'NONE', #40001, #12462, #7651, .T. ) ;
#16405 = EDGE_CURVE ( 'NONE', #51701, #45007, #35498, .T. ) ;
#16406 = ORIENTED_EDGE ( 'NONE', *, *, #44992, .F. ) ;
#16407 = FACE_OUTER_BOUND ( 'NONE', #15164, .T. ) ;
#16408 = DIRECTION ( 'NONE',  ( 0.000000000000000000, -0.6631226582407885317, 0.7485107481711069655 ) ) ;
#16409 = EDGE_CURVE ( 'NONE', #12138, #41880, #15818, .T. ) ;
#16410 = EDGE_CURVE ( 'NONE', #1773, #16914, #2931, .T. ) ;
#16411 = ORIENTED_EDGE ( 'NONE', *, *, #40430, .F. ) ;
#16412 = DIRECTION ( 'NONE',  ( -0.000000000000000000, 1.000000000000000000, -0.000000000000000000 ) ) ;
#16413 = EDGE_LOOP ( 'NONE', ( #44632, #19647, #70, #18512 ) ) ;
#16414 = FACE_BOUND ( 'NONE', #32898, .T. ) ;
#16415 = VECTOR ( 'NONE', #42894, 1000.000000000000000 ) ;
#16416 = DIRECTION ( 'NONE',  ( 0.000000000000000000, 0.000000000000000000, -1.000000000000000000 ) ) ;
#16417 = ORIENTED_EDGE ( 'NONE', *, *, #24024, .F. ) ;
#16418 = VECTOR ( 'NONE', #16141, 1000.000000000000000 ) ;
#16419 = VECTOR ( 'NONE', #18168, 1000.000000000000000 ) ;
#16420 = FACE_OUTER_BOUND ( 'NONE', #12300, .T. ) ;
#16421 = DIRECTION ( 'NONE',  ( 0.000000000000000000, 0.000000000000000000, 1.000000000000000000 ) ) ;
#16422 = DIRECTION ( 'NONE',  ( 0.000000000000000000, -0.6631226582407937498, 0.7485107481711024136 ) ) ;
#16423 = LINE ( 'NONE', #4860, #4782 ) ;
#16424 = EDGE_LOOP ( 'NONE', ( #6480, #50075, #50965, #23498 ) ) ;
#16425 = CARTESIAN_POINT ( 'NONE',  ( -336.3521761649654422, -174.5186198893880771, 29.74944317415823392 ) ) ;
#16426 = VERTEX_POINT ( 'NONE', #39195 ) ;
#16427 = ORIENTED_EDGE ( 'NONE', *, *, #16894, .F. ) ;
#16429 = AXIS2_PLACEMENT_3D ( 'NONE', #4361, #20131, #40340 ) ;
#16428 = PRODUCT_RELATED_PRODUCT_CATEGORY ( 'part', '', ( #20959 ) ) ;
#16430 = DIRECTION ( 'NONE',  ( 1.000000000000000000, -0.000000000000000000, 0.000000000000000000 ) ) ;
#16432 = VERTEX_POINT ( 'NONE', #31302 ) ;
#16431 = CARTESIAN_POINT ( 'NONE',  ( -170.2790847791494855, -183.6283474603465606, -28.10285082451569494 ) ) ;
#16433 = CIRCLE ( 'NONE', #36553, 60.00000000000000000 ) ;
#16434 = EDGE_LOOP ( 'NONE', ( #17548, #39537, #435, #29319 ) ) ;
#16435 = CARTESIAN_POINT ( 'NONE',  ( 53.56330073376472001, -189.7472609257535510, 72.19655804062048787 ) ) ;
#16436 = VECTOR ( 'NONE', #24465, 1000.000000000000114 ) ;
#16437 = ADVANCED_FACE ( 'NONE', ( #31831 ), #15544, .F. ) ;
#16438 = AXIS2_PLACEMENT_3D ( 'NONE', #20065, #8239, #32405 ) ;
#16439 = LINE ( 'NONE', #31675, #50330 ) ;
#16440 = VERTEX_POINT ( 'NONE', #11068 ) ;
#16441 = DIRECTION ( 'NONE',  ( 0.000000000000000000, 0.000000000000000000, -1.000000000000000000 ) ) ;
#16442 = VERTEX_POINT ( 'NONE', #36028 ) ;
#16443 = DIRECTION ( 'NONE',  ( 1.000000000000000000, 0.000000000000000000, 0.000000000000000000 ) ) ;
#16444 = FACE_OUTER_BOUND ( 'NONE', #44595, .T. ) ;
#16445 = CARTESIAN_POINT ( 'NONE',  ( -339.1964088526558498, -175.9742670995615015, -26.97593913775538965 ) ) ;
#16446 = DIRECTION ( 'NONE',  ( -1.000000000000000000, 0.000000000000000000, 0.000000000000000000 ) ) ;
#16447 = VERTEX_POINT ( 'NONE', #32078 ) ;
#16448 = VERTEX_POINT ( 'NONE', #48119 ) ;
#16449 = VERTEX_POINT ( 'NONE', #27359 ) ;
#16450 = DIRECTION ( 'NONE',  ( 0.000000000000000000, 0.000000000000000000, 1.000000000000000000 ) ) ;
#16451 = CARTESIAN_POINT ( 'NONE',  ( -336.3521761649654422, -125.1322888500942270, -59.00000000000002132 ) ) ;
#16452 = AXIS2_PLACEMENT_3D ( 'NONE', #24952, #40964, #17077 ) ;
#16453 = CARTESIAN_POINT ( 'NONE',  ( -48.47912675150885065, -177.1207230881787780, 6.938893903907228378E-15 ) ) ;
#16454 = CIRCLE ( 'NONE', #46687, 125.0000000000000000 ) ;
#16455 = FACE_BOUND ( 'NONE', #28987, .T. ) ;
#16456 = DIRECTION ( 'NONE',  ( 0.000000000000000000, 0.4647231720437664526, -0.8854560256532110207 ) ) ;
#16457 = ORIENTED_EDGE ( 'NONE', *, *, #35318, .F. ) ;
#16458 = ORIENTED_EDGE ( 'NONE', *, *, #14880, .F. ) ;
#16460 = ORIENTED_EDGE ( 'NONE', *, *, #34275, .F. ) ;
#16459 = DIRECTION ( 'NONE',  ( 1.043714542225393381E-14, -0.4647231720437631775, 0.8854560256532126861 ) ) ;
#16461 = ORIENTED_EDGE ( 'NONE', *, *, #40850, .T. ) ;
#16462 = DIRECTION ( 'NONE',  ( 0.000000000000000000, 0.000000000000000000, 1.000000000000000000 ) ) ;
#16463 = AXIS2_PLACEMENT_3D ( 'NONE', #13289, #1463, #29311 ) ;
#16464 = DIRECTION ( 'NONE',  ( -0.000000000000000000, 1.000000000000000000, -0.000000000000000000 ) ) ;
#16465 = CIRCLE ( 'NONE', #45843, 125.0000000000000000 ) ;
#16466 = DIRECTION ( 'NONE',  ( 0.000000000000000000, 0.000000000000000000, -1.000000000000000000 ) ) ;
#16467 = EDGE_CURVE ( 'NONE', #36797, #794, #47616, .T. ) ;
#16468 = CARTESIAN_POINT ( 'NONE',  ( 65.79610465833508215, -193.5000000000000000, -50.65739320401928580 ) ) ;
#16469 = EDGE_LOOP ( 'NONE', ( #3224, #4951, #34420, #12019 ) ) ;
#16470 = DIRECTION ( 'NONE',  ( 0.000000000000000000, 0.000000000000000000, 1.000000000000000000 ) ) ;
#16471 = VECTOR ( 'NONE', #17890, 1000.000000000000000 ) ;
#16472 = EDGE_LOOP ( 'NONE', ( #11854, #32957, #15729, #20161 ) ) ;
#16473 = AXIS2_PLACEMENT_3D ( 'NONE', #3801, #10659, #42966 ) ;
#16474 = VERTEX_POINT ( 'NONE', #11321 ) ;
#16475 = DIRECTION ( 'NONE',  ( -0.000000000000000000, 0.4647231720437695057, 0.8854560256532093554 ) ) ;
#16476 = CARTESIAN_POINT ( 'NONE',  ( -336.3521761649654422, -123.5000000000000284, 0.000000000000000000 ) ) ;
#16477 = CARTESIAN_POINT ( 'NONE',  ( -67.22356632362124174, -177.1207230881787780, -123.5865930638409509 ) ) ;
#16478 = CARTESIAN_POINT ( 'NONE',  ( -332.3517673607765914, -154.8494888031386836, 50.05135858667791382 ) ) ;
#16479 = PLANE ( 'NONE',  #44816 ) ;
#16480 = DIRECTION ( 'NONE',  ( -0.000000000000000000, 1.000000000000000000, -0.000000000000000000 ) ) ;
#16481 = EDGE_LOOP ( 'NONE', ( #41595, #12796, #38748, #14679 ) ) ;
#16482 = CARTESIAN_POINT ( 'NONE',  ( 47.58409946089483356, 28.88712326890129489, -43.00657248973679714 ) ) ;
#16483 = DIRECTION ( 'NONE',  ( -0.000000000000000000, 1.000000000000000000, -0.000000000000000000 ) ) ;
#16484 = FACE_OUTER_BOUND ( 'NONE', #7017, .T. ) ;
#16485 = FACE_BOUND ( 'NONE', #1365, .T. ) ;
#16486 = ORIENTED_EDGE ( 'NONE', *, *, #35594, .F. ) ;
#16487 = VECTOR ( 'NONE', #26418, 1000.000000000000000 ) ;
#16488 = AXIS2_PLACEMENT_3D ( 'NONE', #32497, #24109, #44583 ) ;
#16489 = EDGE_CURVE ( 'NONE', #13663, #51264, #2126, .T. ) ;
#16490 = CARTESIAN_POINT ( 'NONE',  ( -339.1964088526558498, -157.4273119900845757, 48.27201571436049932 ) ) ;
#16491 = AXIS2_PLACEMENT_3D ( 'NONE', #21848, #44988, #37859 ) ;
#16492 = CARTESIAN_POINT ( 'NONE',  ( -339.1964088526558498, -176.3931552210903249, -28.32515014536811293 ) ) ;
#16493 = ORIENTED_EDGE ( 'NONE', *, *, #5095, .F. ) ;
#16494 = CARTESIAN_POINT ( 'NONE',  ( -330.4913330509368166, -171.7720157143599238, 33.92731199008539278 ) ) ;
#16495 = VERTEX_POINT ( 'NONE', #34995 ) ;
#16496 = DIRECTION ( 'NONE',  ( -0.000000000000000000, 1.000000000000000000, -0.000000000000000000 ) ) ;
#16497 = CIRCLE ( 'NONE', #25838, 124.9999999999999858 ) ;
#16498 = CARTESIAN_POINT ( 'NONE',  ( 15.23368049493606335, -189.7472609257535510, -107.5438431188757136 ) ) ;
#16500 = VERTEX_POINT ( 'NONE', #7413 ) ;
#16499 = CARTESIAN_POINT ( 'NONE',  ( 69.04371411670898340, -193.5000000000000000, -39.55227055146230697 ) ) ;
#16501 = ADVANCED_FACE ( 'NONE', ( #27095 ), #7137, .T. ) ;
#16502 = CIRCLE ( 'NONE', #45879, 125.0000000000000000 ) ;
#16503 = AXIS2_PLACEMENT_3D ( 'NONE', #6260, #50933, #22281 ) ;
#16504 = EDGE_CURVE ( 'NONE', #28628, #49289, #36518, .T. ) ;
#16505 = AXIS2_PLACEMENT_3D ( 'NONE', #22243, #30635, #46690 ) ;
#16506 = CARTESIAN_POINT ( 'NONE',  ( -339.1964088526558498, -156.6043281241916816, -48.84008046109114076 ) ) ;
#16507 = VERTEX_POINT ( 'NONE', #11599 ) ;
#16508 = ORIENTED_EDGE ( 'NONE', *, *, #38177, .T. ) ;
#16509 = AXIS2_PLACEMENT_3D ( 'NONE', #25829, #9542, #6129 ) ;
#16510 = CARTESIAN_POINT ( 'NONE',  ( 116.9235303384055840, -213.5000000000000000, 10.00000000000000000 ) ) ;
#16511 = ADVANCED_FACE ( 'NONE', ( #27626 ), #24209, .F. ) ;
#16512 = ORIENTED_EDGE ( 'NONE', *, *, #12861, .T. ) ;
#16513 = VECTOR ( 'NONE', #35177, 999.9999999999998863 ) ;
#16514 = DIRECTION ( 'NONE',  ( 0.7765238627180349740, 0.000000000000000000, 0.6300878435817203194 ) ) ;
#16515 = LINE ( 'NONE', #29099, #49679 ) ;
#16516 = CARTESIAN_POINT ( 'NONE',  ( -173.0563034899574859, -189.7472609257535510, -10.27263529369817618 ) ) ;
#16517 = EDGE_CURVE ( 'NONE', #28894, #50885, #7159, .T. ) ;
#16518 = CARTESIAN_POINT ( 'NONE',  ( -336.3521761649654422, -119.0014323656137947, -58.88711093124865670 ) ) ;
#16519 = DIRECTION ( 'NONE',  ( 0.000000000000000000, -1.000000000000000000, -0.000000000000000000 ) ) ;
#16520 = ORIENTED_EDGE ( 'NONE', *, *, #7386, .F. ) ;
#16523 = VERTEX_POINT ( 'NONE', #277 ) ;
#16522 = DIRECTION ( 'NONE',  ( 0.000000000000000000, -0.000000000000000000, 1.000000000000000000 ) ) ;
#16521 = DIRECTION ( 'NONE',  ( -0.000000000000000000, 1.000000000000000000, -0.000000000000000000 ) ) ;
#16524 = VECTOR ( 'NONE', #23522, 1000.000000000000000 ) ;
#16525 = ORIENTED_EDGE ( 'NONE', *, *, #20067, .F. ) ;
#16526 = AXIS2_PLACEMENT_3D ( 'NONE', #10086, #38184, #17723 ) ;
#16527 = FACE_OUTER_BOUND ( 'NONE', #10154, .T. ) ;
#16528 = EDGE_LOOP ( 'NONE', ( #16825, #20237, #46310, #46107 ) ) ;
#16529 = DIRECTION ( 'NONE',  ( 0.000000000000000000, 0.000000000000000000, -1.000000000000000000 ) ) ;
#16530 = VERTEX_POINT ( 'NONE', #12621 ) ;
#16531 = VECTOR ( 'NONE', #15089, 1000.000000000000000 ) ;
#16532 = CARTESIAN_POINT ( 'NONE',  ( 35.67816836544798065, -183.6283474603465606, -92.42591454022746689 ) ) ;
#16533 = EDGE_CURVE ( 'NONE', #6563, #44074, #29808, .T. ) ;
#16534 = CARTESIAN_POINT ( 'NONE',  ( -2.700932609314997457, -193.5000000000000000, -116.3157639405751809 ) ) ;
#16535 = EDGE_LOOP ( 'NONE', ( #46347, #19364, #1343, #7920 ) ) ;
#16537 = CARTESIAN_POINT ( 'NONE',  ( -339.1964088526558498, -123.5000000000000284, 0.000000000000000000 ) ) ;
#16536 = DIRECTION ( 'NONE',  ( -0.000000000000000000, 1.000000000000000000, -0.000000000000000000 ) ) ;
#16538 = ORIENTED_EDGE ( 'NONE', *, *, #43964, .F. ) ;
#16539 = ADVANCED_FACE ( 'NONE', ( #29180 ), #21300, .F. ) ;
#16540 = VERTEX_POINT ( 'NONE', #21041 ) ;
#16541 = LINE ( 'NONE', #31785, #40475 ) ;
#16542 = CIRCLE ( 'NONE', #45057, 125.0000000000000000 ) ;
#16543 = EDGE_CURVE ( 'NONE', #14578, #3536, #20509, .T. ) ;
#16544 = CARTESIAN_POINT ( 'NONE',  ( -330.4913330509368166, -182.1300919119129560, -6.615309698014691264 ) ) ;
#16545 = AXIS2_PLACEMENT_3D ( 'NONE', #51361, #23999, #35559 ) ;
#16546 = DIRECTION ( 'NONE',  ( 0.000000000000000000, -0.000000000000000000, 1.000000000000000000 ) ) ;
#16547 = DIRECTION ( 'NONE',  ( -0.6965510290629882695, 0.000000000000000000, -0.7175072570443395970 ) ) ;
#16548 = LINE ( 'NONE', #35452, #6459 ) ;
#16549 = AXIS2_PLACEMENT_3D ( 'NONE', #36349, #1119, #28455 ) ;
#16550 = AXIS2_PLACEMENT_3D ( 'NONE', #36838, #28414, #44463 ) ;
#16551 = FACE_OUTER_BOUND ( 'NONE', #24472, .T. ) ;
#16552 = SHAPE_DEFINITION_REPRESENTATION ( #14704, #4578 ) ;
#16553 = PLANE ( 'NONE',  #19458 ) ;
#16554 = VECTOR ( 'NONE', #39741, 1000.000000000000000 ) ;
#16555 = LINE ( 'NONE', #51779, #28810 ) ;
#16556 = DIRECTION ( 'NONE',  ( -0.000000000000000000, 1.000000000000000000, -0.000000000000000000 ) ) ;
#16557 = CIRCLE ( 'NONE', #23267, 15.24495751795539000 ) ;
#16558 = FACE_OUTER_BOUND ( 'NONE', #19046, .T. ) ;
#16559 = VERTEX_POINT ( 'NONE', #20254 ) ;
#16560 = ORIENTED_EDGE ( 'NONE', *, *, #33253, .T. ) ;
#16561 = DIRECTION ( 'NONE',  ( 0.000000000000000000, 0.1205366802553199251, -0.9927088740980544168 ) ) ;
#16562 = ADVANCED_FACE ( 'NONE', ( #13415 ), #36277, .F. ) ;
#16563 = CARTESIAN_POINT ( 'NONE',  ( -330.4913330509368166, -84.00150778970706256, 43.83057281297416097 ) ) ;
#16564 = DIRECTION ( 'NONE',  ( 0.000000000000000000, 0.000000000000000000, 1.000000000000000000 ) ) ;
#16565 = ORIENTED_EDGE ( 'NONE', *, *, #36879, .T. ) ;
#16566 = ORIENTED_EDGE ( 'NONE', *, *, #40704, .T. ) ;
#16567 = EDGE_LOOP ( 'NONE', ( #23480, #19673, #37430, #17681 ) ) ;
#16568 = AXIS2_PLACEMENT_3D ( 'NONE', #29570, #17761, #46143 ) ;
#16569 = DIRECTION ( 'NONE',  ( 0.000000000000000000, 0.9927088740980548609, 0.1205366802553164696 ) ) ;
#16570 = AXIS2_PLACEMENT_3D ( 'NONE', #20283, #308, #44729 ) ;
#16571 = CARTESIAN_POINT ( 'NONE',  ( -145.2888470698896981, -193.5000000000000000, -77.48473115145239376 ) ) ;
#16572 = DIRECTION ( 'NONE',  ( 0.000000000000000000, 0.000000000000000000, -1.000000000000000000 ) ) ;
#16573 = AXIS2_PLACEMENT_3D ( 'NONE', #45995, #38072, #17857 ) ;
#16574 = ORIENTED_EDGE ( 'NONE', *, *, #24704, .F. ) ;
#16575 = CARTESIAN_POINT ( 'NONE',  ( 72.68824389704326450, -175.3837268820161057, -26.35287080855459863 ) ) ;
#16576 = CARTESIAN_POINT ( 'NONE',  ( -330.4913330509368166, -71.49045607248250178, -27.86139516340898581 ) ) ;
#16577 = DIRECTION ( 'NONE',  ( 0.000000000000000000, -7.632783294297951215E-14, 1.000000000000000000 ) ) ;
#16578 = ORIENTED_EDGE ( 'NONE', *, *, #7832, .F. ) ;
#16579 = AXIS2_PLACEMENT_3D ( 'NONE', #27208, #23021, #46686 ) ;
#16580 = AXIS2_PLACEMENT_3D ( 'NONE', #33700, #25819, #41851 ) ;
#16581 = EDGE_LOOP ( 'NONE', ( #24177, #42783, #17528, #43843 ) ) ;
#16582 = LINE ( 'NONE', #24983, #27540 ) ;
#16583 = VECTOR ( 'NONE', #18074, 1000.000000000000000 ) ;
#16584 = ADVANCED_FACE ( 'NONE', ( #24453 ), #20781, .F. ) ;
#16585 = ADVANCED_FACE ( 'NONE', ( #48380 ), #1320, .T. ) ;
#16586 = AXIS2_PLACEMENT_3D ( 'NONE', #39903, #7860, #228 ) ;
#16587 = AXIS2_PLACEMENT_3D ( 'NONE', #39191, #26587, #50268 ) ;
#16588 = FACE_OUTER_BOUND ( 'NONE', #12349, .T. ) ;
#16589 = DIRECTION ( 'NONE',  ( 0.000000000000000000, 0.000000000000000000, 1.000000000000000000 ) ) ;
#16592 = ORIENTED_EDGE ( 'NONE', *, *, #49030, .T. ) ;
#16591 = CARTESIAN_POINT ( 'NONE',  ( -339.1964088526558498, -167.9936954712156592, -38.74998146212110584 ) ) ;
#16590 = CARTESIAN_POINT ( 'NONE',  ( -180.0000000000000568, -123.5000000000000284, -45.63467731922664683 ) ) ;
#16593 = CARTESIAN_POINT ( 'NONE',  ( -48.47912675150885065, -189.7472609257535510, 6.938893903907228378E-15 ) ) ;
#16594 = ORIENTED_EDGE ( 'NONE', *, *, #11245, .F. ) ;
#16595 = PLANE ( 'NONE',  #48229 ) ;
#16596 = PLANE ( 'NONE',  #43418 ) ;
#16597 = VERTEX_POINT ( 'NONE', #28391 ) ;
#16598 = CARTESIAN_POINT ( 'NONE',  ( -336.3521761649654422, -177.7325358280884586, 23.38292116578760726 ) ) ;
#16599 = EDGE_CURVE ( 'NONE', #13870, #34792, #44440, .T. ) ;
#16600 = DIRECTION ( 'NONE',  ( 0.000000000000000000, 1.000000000000000000, 0.000000000000000000 ) ) ;
#16602 = CARTESIAN_POINT ( 'NONE',  ( 73.66680038934278230, -193.5000000000000000, -26.55884942729568365 ) ) ;
#16601 = DIRECTION ( 'NONE',  ( 0.000000000000000000, 1.000000000000000000, 0.000000000000000000 ) ) ;
#16603 = EDGE_LOOP ( 'NONE', ( #16255, #33891, #46527, #12080 ) ) ;
#16604 = ADVANCED_FACE ( 'NONE', ( #8957 ), #17381, .F. ) ;
#16605 = DIRECTION ( 'NONE',  ( -0.3758275821142357809, 0.000000000000000000, -0.9266896074318343723 ) ) ;
#16606 = VECTOR ( 'NONE', #94, 1000.000000000000227 ) ;
#16607 = CARTESIAN_POINT ( 'NONE',  ( -48.65601702663143868, -189.7472609257535510, 0.9842305779476024918 ) ) ;
#16608 = AXIS2_PLACEMENT_3D ( 'NONE', #23380, #43602, #7597 ) ;
#16609 = EDGE_CURVE ( 'NONE', #512, #48767, #41002, .T. ) ;
#16610 = CARTESIAN_POINT ( 'NONE',  ( 28.02885774092381865, -189.7472609257535510, 98.85104101073331151 ) ) ;
#16611 = ORIENTED_EDGE ( 'NONE', *, *, #38996, .F. ) ;
#16612 = FILL_AREA_STYLE ('',( #41021 ) ) ;
#16613 = DIRECTION ( 'NONE',  ( 0.000000000000000000, 0.000000000000000000, 1.000000000000000000 ) ) ;
#16614 = AXIS2_PLACEMENT_3D ( 'NONE', #5068, #5859, #9270 ) ;
#16615 = CARTESIAN_POINT ( 'NONE',  ( -21.46839590530488451, -177.1207230881787780, 122.0467960216650738 ) ) ;
#16616 = EDGE_CURVE ( 'NONE', #20140, #32545, #41549, .T. ) ;
#16617 = ORIENTED_EDGE ( 'NONE', *, *, #2401, .T. ) ;
#16618 = DIRECTION ( 'NONE',  ( 0.9473263538541923934, 0.000000000000000000, -0.3202698538628350744 ) ) ;
#16619 = DIRECTION ( 'NONE',  ( 1.000000000000000000, 0.000000000000000000, 0.000000000000000000 ) ) ;
#16620 = ORIENTED_EDGE ( 'NONE', *, *, #45146, .T. ) ;
#16621 = CARTESIAN_POINT ( 'NONE',  ( -332.3517673607765914, -145.9479049231020440, -54.58714071513102795 ) ) ;
#16622 = ORIENTED_EDGE ( 'NONE', *, *, #29301, .T. ) ;
#16623 = VECTOR ( 'NONE', #4880, 1000.000000000000000 ) ;
#16624 = CARTESIAN_POINT ( 'NONE',  ( -9.671950287350391307, -193.5000000000000000, -118.8234112238815499 ) ) ;
#16625 = DIRECTION ( 'NONE',  ( 0.000000000000000000, 0.000000000000000000, 1.000000000000000000 ) ) ;
#16626 = CARTESIAN_POINT ( 'NONE',  ( -49.32472275501067571, -177.1207230881787780, -0.5338233779647935107 ) ) ;
#16627 = LINE ( 'NONE', #22038, #6291 ) ;
#16628 = DIRECTION ( 'NONE',  ( 0.000000000000000000, -0.2393156642875652051, -0.9709418174260502354 ) ) ;
#16630 = AXIS2_PLACEMENT_3D ( 'NONE', #22320, #34414, #14454 ) ;
#16629 = PLANE ( 'NONE',  #11169 ) ;
#16631 = FACE_OUTER_BOUND ( 'NONE', #41409, .T. ) ;
#16632 = CYLINDRICAL_SURFACE ( 'NONE', #50563, 125.0000000000000000 ) ;
#16634 = VERTEX_POINT ( 'NONE', #49441 ) ;
#16633 = FACE_OUTER_BOUND ( 'NONE', #29874, .T. ) ;
#16635 = ORIENTED_EDGE ( 'NONE', *, *, #36402, .F. ) ;
#16636 = LINE ( 'NONE', #8725, #47631 ) ;
#16637 = DIRECTION ( 'NONE',  ( -0.6068001458185890984, 0.000000000000000000, -0.7948544414133565938 ) ) ;
#16638 = ORIENTED_EDGE ( 'NONE', *, *, #32991, .F. ) ;
#16639 = VECTOR ( 'NONE', #10709, 1000.000000000000114 ) ;
#16640 = VERTEX_POINT ( 'NONE', #1055 ) ;
#16642 = EDGE_CURVE ( 'NONE', #1163, #23236, #25609, .T. ) ;
#16641 = ORIENTED_EDGE ( 'NONE', *, *, #402, .F. ) ;
#16643 = FACE_OUTER_BOUND ( 'NONE', #41020, .T. ) ;
#16644 = VECTOR ( 'NONE', #19225, 1000.000000000000000 ) ;
#16645 = EDGE_CURVE ( 'NONE', #2312, #45117, #27286, .T. ) ;
#16646 = ADVANCED_FACE ( 'NONE', ( #48653 ), #44174, .F. ) ;
#16647 = EDGE_CURVE ( 'NONE', #48164, #11058, #29959, .T. ) ;
#16648 = CARTESIAN_POINT ( 'NONE',  ( -48.13092511607445800, -183.6283474603465606, 0.9374196611341301111 ) ) ;
#16649 = DIRECTION ( 'NONE',  ( -0.000000000000000000, 1.000000000000000000, 0.000000000000000000 ) ) ;
#16650 = VERTEX_POINT ( 'NONE', #42558 ) ;
#16651 = ORIENTED_EDGE ( 'NONE', *, *, #51252, .F. ) ;
#16652 = ADVANCED_FACE ( 'NONE', ( #22070 ), #33641, .T. ) ;
#16653 = CARTESIAN_POINT ( 'NONE',  ( -30.00000000000000000, 0.000000000000000000, -30.00000000000000711 ) ) ;
#16654 = CARTESIAN_POINT ( 'NONE',  ( -332.3517673607765914, -165.9166037625627439, 41.09453333279358134 ) ) ;
#16655 = AXIS2_PLACEMENT_3D ( 'NONE', #7068, #43320, #46498 ) ;
#16657 = ORIENTED_EDGE ( 'NONE', *, *, #44149, .T. ) ;
#16656 = FACE_OUTER_BOUND ( 'NONE', #49626, .T. ) ;
#16658 = ADVANCED_FACE ( 'NONE', ( #6054 ), #49939, .T. ) ;
#16659 = CARTESIAN_POINT ( 'NONE',  ( -142.9772358822569629, -177.1207230881787780, 81.82363577055969017 ) ) ;
#16660 = CARTESIAN_POINT ( 'NONE',  ( -330.4913330509368166, -65.12585595286510909, 13.87297036558300078 ) ) ;
#16661 = ORIENTED_EDGE ( 'NONE', *, *, #21040, .T. ) ;
#16662 = CARTESIAN_POINT ( 'NONE',  ( -330.4913330509368166, -157.4273119900852578, -48.27201571436002325 ) ) ;
#16663 = VERTEX_POINT ( 'NONE', #18136 ) ;
#16664 = LINE ( 'NONE', #45036, #49257 ) ;
#16665 = EDGE_CURVE ( 'NONE', #23203, #44669, #17634, .T. ) ;
#16666 = DIRECTION ( 'NONE',  ( -0.000000000000000000, 1.000000000000000000, -0.000000000000000000 ) ) ;
#16667 = CARTESIAN_POINT ( 'NONE',  ( 74.77174840718836890, -183.6283474603465606, 20.83798868929603998 ) ) ;
#16668 = ADVANCED_FACE ( 'NONE', ( #22601 ), #14459, .F. ) ;
#16669 = VECTOR ( 'NONE', #18405, 1000.000000000000000 ) ;
#16670 = ORIENTED_EDGE ( 'NONE', *, *, #9633, .F. ) ;
#16671 = ORIENTED_EDGE ( 'NONE', *, *, #8520, .T. ) ;
#16672 = CARTESIAN_POINT ( 'NONE',  ( -113.4314575050762102, -123.5000000000000284, 6.938893903907228378E-15 ) ) ;
#16673 = ADVANCED_FACE ( 'NONE', ( #45738 ), #9731, .T. ) ;
#16674 = LINE ( 'NONE', #36621, #39244 ) ;
#16675 = EDGE_LOOP ( 'NONE', ( #26873, #43280, #8538, #35973 ) ) ;
#16676 = CARTESIAN_POINT ( 'NONE',  ( 75.47134233844786877, -189.7472609257535510, -3.504489105734906129 ) ) ;
#16677 = EDGE_CURVE ( 'NONE', #7946, #809, #25498, .T. ) ;
#16678 = DIRECTION ( 'NONE',  ( 0.000000000000000000, -1.000000000000000000, 0.000000000000000000 ) ) ;
#16679 = ORIENTED_EDGE ( 'NONE', *, *, #37566, .T. ) ;
#16680 = FACE_OUTER_BOUND ( 'NONE', #49607, .T. ) ;
#16681 = EDGE_CURVE ( 'NONE', #41662, #4093, #34162, .T. ) ;
#16682 = CARTESIAN_POINT ( 'NONE',  ( -332.3517673607765914, -106.8245764869328980, 56.65561927337994064 ) ) ;
#16683 = ORIENTED_EDGE ( 'NONE', *, *, #4429, .T. ) ;
#16684 = CARTESIAN_POINT ( 'NONE',  ( -70.42295845586430403, -189.7472609257535510, -123.0587999703025019 ) ) ;
#16685 = EDGE_LOOP ( 'NONE', ( #41648, #19731, #4991, #13422 ) ) ;
#16686 = CIRCLE ( 'NONE', #23386, 5.000000000000001776 ) ;
#16687 = AXIS2_PLACEMENT_3D ( 'NONE', #42282, #10998, #46765 ) ;
#16688 = DIRECTION ( 'NONE',  ( 0.000000000000000000, -0.000000000000000000, -1.000000000000000000 ) ) ;
#16689 = EDGE_LOOP ( 'NONE', ( #1617, #19498, #9809, #26927 ) ) ;
#16690 = VECTOR ( 'NONE', #3376, 1000.000000000000000 ) ;
#16691 = DIRECTION ( 'NONE',  ( 0.000000000000000000, 1.000000000000000000, 0.000000000000000000 ) ) ;
#16692 = PLANE ( 'NONE',  #3724 ) ;
#16693 = DIRECTION ( 'NONE',  ( 0.000000000000000000, 1.000000000000000000, 0.000000000000000000 ) ) ;
#16694 = CARTESIAN_POINT ( 'NONE',  ( -339.1964088526558498, -183.0001959263614424, -7.728304129924259414 ) ) ;
#16695 = ADVANCED_FACE ( 'NONE', ( #46512 ), #10001, .T. ) ;
#16696 = ORIENTED_EDGE ( 'NONE', *, *, #51726, .F. ) ;
#16697 = FACE_OUTER_BOUND ( 'NONE', #7243, .T. ) ;
#16698 = VERTEX_POINT ( 'NONE', #5816 ) ;
#16699 = EDGE_LOOP ( 'NONE', ( #6440, #11737, #24637, #1521 ) ) ;
#16700 = AXIS2_PLACEMENT_3D ( 'NONE', #42752, #43251, #7005 ) ;
#16701 = DIRECTION ( 'NONE',  ( 1.000000000000000000, -0.000000000000000000, -0.000000000000000000 ) ) ;
#16703 = ORIENTED_EDGE ( 'NONE', *, *, #12108, .F. ) ;
#16702 = DIRECTION ( 'NONE',  ( 0.000000000000000000, -1.000000000000000000, -0.000000000000000000 ) ) ;
#16704 = VERTEX_POINT ( 'NONE', #50210 ) ;
#16705 = DIRECTION ( 'NONE',  ( 0.9960498426152171181, 0.000000000000000000, -0.08879589532293157006 ) ) ;
#16706 = VECTOR ( 'NONE', #25958, 1000.000000000000000 ) ;
#16707 = ADVANCED_FACE ( 'NONE', ( #21828 ), #46013, .F. ) ;
#16708 = DIRECTION ( 'NONE',  ( 0.000000000000000000, 0.000000000000000000, 1.000000000000000000 ) ) ;
#16709 = ORIENTED_EDGE ( 'NONE', *, *, #2023, .T. ) ;
#16710 = PLANE ( 'NONE',  #44063 ) ;
#16711 = VERTEX_POINT ( 'NONE', #6577 ) ;
#16712 = CARTESIAN_POINT ( 'NONE',  ( 57.66105628977221897, -193.5000000000000000, 66.02470404298190942 ) ) ;
#16713 = PLANE ( 'NONE',  #22458 ) ;
#16714 = EDGE_CURVE ( 'NONE', #18469, #23765, #50462, .T. ) ;
#16715 = ADVANCED_FACE ( 'NONE', ( #34666 ), #26015, .T. ) ;
#16716 = CARTESIAN_POINT ( 'NONE',  ( -336.3521761649654422, -135.0638248728647852, 57.91551518289418254 ) ) ;
#16717 = DIRECTION ( 'NONE',  ( -0.6528221181905119463, 0.000000000000000000, -0.7575112421616284619 ) ) ;
#16718 = ORIENTED_EDGE ( 'NONE', *, *, #4731, .T. ) ;
#16719 = ORIENTED_EDGE ( 'NONE', *, *, #10367, .F. ) ;
#16720 = ADVANCED_FACE ( 'NONE', ( #6306 ), #38612, .F. ) ;
#16721 = ORIENTED_EDGE ( 'NONE', *, *, #46479, .F. ) ;
#16722 = EDGE_CURVE ( 'NONE', #33480, #13761, #2615, .T. ) ;
#16723 = CARTESIAN_POINT ( 'NONE',  ( 60.00000000000001421, -93.50000000000001421, -51.54700538379269403 ) ) ;
#16724 = FACE_OUTER_BOUND ( 'NONE', #23995, .T. ) ;
#16725 = AXIS2_PLACEMENT_3D ( 'NONE', #48357, #12338, #44420 ) ;
#16726 = DIRECTION ( 'NONE',  ( 0.000000000000000000, -1.000000000000000000, 0.000000000000000000 ) ) ;
#16727 = DIRECTION ( 'NONE',  ( 1.000000000000000000, -0.000000000000000000, -0.000000000000000000 ) ) ;
#16728 = CARTESIAN_POINT ( 'NONE',  ( -33.52607327456454556, -175.3837268820161057, -124.1024020384603119 ) ) ;
#16729 = EDGE_LOOP ( 'NONE', ( #17580, #25340, #45988, #25585 ) ) ;
#16730 = AXIS2_PLACEMENT_3D ( 'NONE', #12499, #16726, #8546 ) ;
#16731 = ORIENTED_EDGE ( 'NONE', *, *, #15427, .F. ) ;
#16733 = ORIENTED_EDGE ( 'NONE', *, *, #48, .T. ) ;
#16732 = DIRECTION ( 'NONE',  ( 0.000000000000000000, -0.6631226582408039638, -0.7485107481710934207 ) ) ;
#16734 = CIRCLE ( 'NONE', #11682, 60.00000000000000000 ) ;
#16735 = CARTESIAN_POINT ( 'NONE',  ( -172.6359455740846442, -193.5000000000000000, -14.49428645563791562 ) ) ;
#16736 = ORIENTED_EDGE ( 'NONE', *, *, #44978, .F. ) ;
#16737 = EDGE_CURVE ( 'NONE', #32906, #50838, #35700, .T. ) ;
#16738 = DIRECTION ( 'NONE',  ( -0.000000000000000000, -1.000000000000000000, -0.000000000000000000 ) ) ;
#16739 = CARTESIAN_POINT ( 'NONE',  ( 11.52087324849114580, -173.5000000000000284, -186.7953921478704729 ) ) ;
#16740 = EDGE_CURVE ( 'NONE', #33166, #33429, #8018, .T. ) ;
#16741 = FACE_OUTER_BOUND ( 'NONE', #15373, .T. ) ;
#16742 = DIRECTION ( 'NONE',  ( 0.000000000000000000, 0.000000000000000000, -1.000000000000000000 ) ) ;
#16743 = ORIENTED_EDGE ( 'NONE', *, *, #30841, .F. ) ;
#16744 = CARTESIAN_POINT ( 'NONE',  ( -41.24387117724851493, -175.3837268820161057, 124.7904286264581231 ) ) ;
#16745 = ORIENTED_EDGE ( 'NONE', *, *, #6680, .T. ) ;
#16746 = EDGE_CURVE ( 'NONE', #20693, #6892, #21413, .T. ) ;
#16747 = VECTOR ( 'NONE', #44986, 1000.000000000000000 ) ;
#16748 = EDGE_LOOP ( 'NONE', ( #49264, #46400, #34836, #19933 ) ) ;
#16749 = CARTESIAN_POINT ( 'NONE',  ( -332.3517673607765914, -123.5000000000000284, 0.000000000000000000 ) ) ;
#16750 = CARTESIAN_POINT ( 'NONE',  ( 51.05451324771860300, -177.1207230881787780, 75.61781872352698031 ) ) ;
#16751 = FACE_OUTER_BOUND ( 'NONE', #49678, .T. ) ;
#16752 = DIRECTION ( 'NONE',  ( -0.000000000000000000, 1.000000000000000000, -0.000000000000000000 ) ) ;
#16753 = DIRECTION ( 'NONE',  ( 0.000000000000000000, 1.000000000000000000, 0.000000000000000000 ) ) ;
#16754 = PLANE ( 'NONE',  #9593 ) ;
#16755 = CARTESIAN_POINT ( 'NONE',  ( -47.57632892154311577, -193.5000000000000000, 0.4300652022765314997 ) ) ;
#16756 = ORIENTED_EDGE ( 'NONE', *, *, #6695, .F. ) ;
#16757 = DIRECTION ( 'NONE',  ( -0.000000000000000000, 1.000000000000000000, -0.000000000000000000 ) ) ;
#16758 = DIRECTION ( 'NONE',  ( -0.000000000000000000, 1.000000000000000000, -0.000000000000000000 ) ) ;
#16759 = DIRECTION ( 'NONE',  ( 0.000000000000000000, 0.000000000000000000, -1.000000000000000000 ) ) ;
#16760 = FACE_BOUND ( 'NONE', #22892, .T. ) ;
#16761 = ORIENTED_EDGE ( 'NONE', *, *, #27407, .T. ) ;
#16762 = VECTOR ( 'NONE', #48505, 1000.000000000000000 ) ;
#16763 = LINE ( 'NONE', #16490, #41572 ) ;
#16764 = VERTEX_POINT ( 'NONE', #46774 ) ;
#16765 = CIRCLE ( 'NONE', #29309, 60.00000000000000000 ) ;
#16766 = PLANE ( 'NONE',  #34527 ) ;
#16767 = ORIENTED_EDGE ( 'NONE', *, *, #28902, .F. ) ;
#16768 = CARTESIAN_POINT ( 'NONE',  ( -260.0000000000000000, -63.50000000000000000, -60.00000000000000711 ) ) ;
#16769 = VERTEX_POINT ( 'NONE', #19941 ) ;
#16770 = CARTESIAN_POINT ( 'NONE',  ( -332.3517673607765914, -78.25545813661345562, 37.90245108779119931 ) ) ;
#16771 = CARTESIAN_POINT ( 'NONE',  ( -9.671950287350391307, -183.6283474603465606, -118.8234112238815641 ) ) ;
#16773 = ORIENTED_EDGE ( 'NONE', *, *, #20144, .T. ) ;
#16772 = LINE ( 'NONE', #12548, #20398 ) ;
#16774 = ADVANCED_FACE ( 'NONE', ( #22848 ), #7349, .T. ) ;
#16775 = EDGE_CURVE ( 'NONE', #975, #17445, #35970, .T. ) ;
#16776 = LINE ( 'NONE', #16240, #36959 ) ;
#16777 = EDGE_LOOP ( 'NONE', ( #8016, #24071, #8778, #49831 ) ) ;
#16778 = VECTOR ( 'NONE', #15677, 1000.000000000000227 ) ;
#16779 = ORIENTED_EDGE ( 'NONE', *, *, #31143, .F. ) ;
#16780 = DIRECTION ( 'NONE',  ( -1.000000000000000000, -0.000000000000000000, -0.000000000000000000 ) ) ;
#16781 = LINE ( 'NONE', #9146, #3327 ) ;
#16782 = ORIENTED_EDGE ( 'NONE', *, *, #38165, .T. ) ;
#16783 = LINE ( 'NONE', #8605, #1599 ) ;
#16784 = DIRECTION ( 'NONE',  ( 0.000000000000000000, -1.000000000000000000, 0.000000000000000000 ) ) ;
#16785 = DIRECTION ( 'NONE',  ( 0.000000000000000000, 0.000000000000000000, 1.000000000000000000 ) ) ;
#16786 = CARTESIAN_POINT ( 'NONE',  ( -332.3517673607765914, -126.1322888500942270, -59.00000000000001421 ) ) ;
#16787 = CARTESIAN_POINT ( 'NONE',  ( -152.8876895714563773, -193.5000000000000000, 66.89437584437911255 ) ) ;
#16788 = ORIENTED_EDGE ( 'NONE', *, *, #24913, .T. ) ;
#16791 = VERTEX_POINT ( 'NONE', #2869 ) ;
#16790 = CARTESIAN_POINT ( 'NONE',  ( -51.83230197877465883, -193.5000000000000000, 123.9551692589637639 ) ) ;
#16789 = DIRECTION ( 'NONE',  ( -1.000000000000000000, 0.000000000000000000, 0.000000000000000000 ) ) ;
#16792 = ORIENTED_EDGE ( 'NONE', *, *, #49922, .F. ) ;
#16793 = VECTOR ( 'NONE', #33625, 1000.000000000000000 ) ;
#16794 = EDGE_CURVE ( 'NONE', #46169, #17312, #26785, .T. ) ;
#16795 = CARTESIAN_POINT ( 'NONE',  ( -339.1964088526558498, -171.7720157143604069, -33.92731199008472487 ) ) ;
#16796 = VERTEX_POINT ( 'NONE', #27806 ) ;
#16797 = DIRECTION ( 'NONE',  ( 0.000000000000000000, 0.000000000000000000, -1.000000000000000000 ) ) ;
#16798 = ORIENTED_EDGE ( 'NONE', *, *, #268, .F. ) ;
#16799 = CARTESIAN_POINT ( 'NONE',  ( -171.5592422664403216, -177.1207230881787780, -21.82395850507255730 ) ) ;
#16800 = CARTESIAN_POINT ( 'NONE',  ( -70.58093260035833794, -193.5000000000000000, 122.0143860769388908 ) ) ;
#16801 = ORIENTED_EDGE ( 'NONE', *, *, #28544, .T. ) ;
#16803 = CARTESIAN_POINT ( 'NONE',  ( 70.02079272397770637, -183.6283474603465606, -36.52255268223056817 ) ) ;
#16802 = DIRECTION ( 'NONE',  ( -0.000000000000000000, -1.000000000000000000, -0.000000000000000000 ) ) ;
#16804 = ORIENTED_EDGE ( 'NONE', *, *, #8391, .T. ) ;
#16805 = EDGE_CURVE ( 'NONE', #9746, #24906, #31772, .T. ) ;
#16806 = ORIENTED_EDGE ( 'NONE', *, *, #9758, .T. ) ;
#16807 = CARTESIAN_POINT ( 'NONE',  ( -339.1964088526558498, -175.5095439275173135, 27.86139516340941213 ) ) ;
#16808 = CARTESIAN_POINT ( 'NONE',  ( -336.3521761649654422, -63.67752800890095699, 4.612141029301496609 ) ) ;
#16809 = CARTESIAN_POINT ( 'NONE',  ( -339.1964088526558498, -123.5000000000000284, 0.000000000000000000 ) ) ;
#16810 = DIRECTION ( 'NONE',  ( -0.000000000000000000, 1.000000000000000000, -0.000000000000000000 ) ) ;
#16811 = EDGE_LOOP ( 'NONE', ( #17310, #49928, #25866, #7322 ) ) ;
#16812 = DIRECTION ( 'NONE',  ( 0.000000000000000000, 1.000000000000000000, 0.000000000000000000 ) ) ;
#16813 = DIRECTION ( 'NONE',  ( 0.000000000000000000, 0.000000000000000000, 1.000000000000000000 ) ) ;
#16814 = FACE_OUTER_BOUND ( 'NONE', #20295, .T. ) ;
#16815 = CARTESIAN_POINT ( 'NONE',  ( -339.1964088526558498, -138.1050951016792681, -57.16590939599323917 ) ) ;
#16816 = DIRECTION ( 'NONE',  ( -0.9890401873221654760, 0.000000000000000000, 0.1476465640024710868 ) ) ;
#16817 = CIRCLE ( 'NONE', #43649, 125.0000000000000000 ) ;
#16818 = AXIS2_PLACEMENT_3D ( 'NONE', #30365, #46673, #26697 ) ;
#16819 = CARTESIAN_POINT ( 'NONE',  ( -48.47912675150885065, -175.3837268820161057, 6.938893903907228378E-15 ) ) ;
#16820 = EDGE_LOOP ( 'NONE', ( #41093, #33690, #5131, #4311 ) ) ;
#16821 = VERTEX_POINT ( 'NONE', #47810 ) ;
#16822 = CARTESIAN_POINT ( 'NONE',  ( -153.7332855749581881, -189.7472609257535510, 67.42819922234390617 ) ) ;
#16823 = CARTESIAN_POINT ( 'NONE',  ( 25.00456841203573077, 45.00000000000000000, 3.062176466986057355E-15 ) ) ;
#16824 = DIRECTION ( 'NONE',  ( 0.4566292373937077542, 0.000000000000000000, 0.8896570909947499883 ) ) ;
#16825 = ORIENTED_EDGE ( 'NONE', *, *, #14880, .T. ) ;
#16826 = ORIENTED_EDGE ( 'NONE', *, *, #51590, .T. ) ;
#16827 = ORIENTED_EDGE ( 'NONE', *, *, #1414, .T. ) ;
#16828 = EDGE_CURVE ( 'NONE', #37393, #46831, #11780, .T. ) ;
#16829 = CARTESIAN_POINT ( 'NONE',  ( -47.78257572244586271, -193.5000000000000000, 0.7175072570443418174 ) ) ;
#16830 = AXIS2_PLACEMENT_3D ( 'NONE', #31479, #6807, #35168 ) ;
#16831 = CARTESIAN_POINT ( 'NONE',  ( 63.39453919430264506, -175.3837268820161057, 53.48161459190911415 ) ) ;
#16832 = CARTESIAN_POINT ( 'NONE',  ( -74.51199343215203896, -177.1207230881787780, -122.2591094863194741 ) ) ;
#16833 = DIRECTION ( 'NONE',  ( 0.000000000000000000, 1.000000000000000000, 0.000000000000000000 ) ) ;
#16834 = ORIENTED_EDGE ( 'NONE', *, *, #27600, .T. ) ;
#16835 = DIRECTION ( 'NONE',  ( 1.000000000000000000, 0.000000000000000000, 0.000000000000000000 ) ) ;
#16836 = EDGE_CURVE ( 'NONE', #32761, #47736, #3384, .T. ) ;
#16837 = DIRECTION ( 'NONE',  ( -0.000000000000000000, -0.8854560256532126861, -0.4647231720437631775 ) ) ;
#16838 = ORIENTED_EDGE ( 'NONE', *, *, #46492, .F. ) ;
#16839 = LINE ( 'NONE', #9206, #19783 ) ;
#16840 = ORIENTED_EDGE ( 'NONE', *, *, #26234, .F. ) ;
#16841 = EDGE_CURVE ( 'NONE', #16447, #26457, #35437, .T. ) ;
#16842 = ORIENTED_EDGE ( 'NONE', *, *, #2583, .F. ) ;
#16843 = CARTESIAN_POINT ( 'NONE',  ( -145.6517069852672535, -193.5000000000000000, 78.62880929222943394 ) ) ;
#16844 = VECTOR ( 'NONE', #37317, 1000.000000000000000 ) ;
#16845 = AXIS2_PLACEMENT_3D ( 'NONE', #28156, #44204, #8204 ) ;
#16846 = CARTESIAN_POINT ( 'NONE',  ( 60.00000000000001421, -43.50000000000000000, -60.00000000000000711 ) ) ;
#16847 = DIRECTION ( 'NONE',  ( -1.000000000000000000, 0.000000000000000000, 0.000000000000000000 ) ) ;
#16850 = ORIENTED_EDGE ( 'NONE', *, *, #9598, .T. ) ;
#16849 = CARTESIAN_POINT ( 'NONE',  ( -339.1964088526558498, -156.6043281241909426, 48.84008046109164525 ) ) ;
#16848 = DIRECTION ( 'NONE',  ( -0.000000000000000000, 1.000000000000000000, 0.000000000000000000 ) ) ;
#16851 = EDGE_CURVE ( 'NONE', #19412, #30801, #6823, .T. ) ;
#16852 = DIRECTION ( 'NONE',  ( -0.000000000000000000, 1.000000000000000000, -0.000000000000000000 ) ) ;
#16853 = ORIENTED_EDGE ( 'NONE', *, *, #46754, .F. ) ;
#16854 = CARTESIAN_POINT ( 'NONE',  ( -122.3978016498073345, -177.1207230881787780, -100.8019320314827070 ) ) ;
#16855 = CARTESIAN_POINT ( 'NONE',  ( -336.3521761649654422, -97.97423230103774472, -54.29949524055093946 ) ) ;
#16856 = ORIENTED_EDGE ( 'NONE', *, *, #38993, .F. ) ;
#16857 = DIRECTION ( 'NONE',  ( -0.8294056854502011022, 0.000000000000000000, -0.5586467658036535777 ) ) ;
#16859 = LINE ( 'NONE', #24729, #23982 ) ;
#16858 = CARTESIAN_POINT ( 'NONE',  ( 10.73478887071926202, -183.6283474603465606, -110.0850225811106924 ) ) ;
#16860 = ORIENTED_EDGE ( 'NONE', *, *, #989, .T. ) ;
#16861 = CARTESIAN_POINT ( 'NONE',  ( -48.47912675150885065, -183.6283474603465606, 6.938893903907228378E-15 ) ) ;
#16862 = PLANE ( 'NONE',  #23641 ) ;
#16864 = AXIS2_PLACEMENT_3D ( 'NONE', #15152, #35890, #20631 ) ;
#16863 = LINE ( 'NONE', #17394, #50858 ) ;
#16865 = ORIENTED_EDGE ( 'NONE', *, *, #8217, .F. ) ;
#16866 = LINE ( 'NONE', #5040, #32516 ) ;
#16867 = CARTESIAN_POINT ( 'NONE',  ( -330.4913330509368166, -123.5000000000000284, 0.000000000000000000 ) ) ;
#16868 = DIRECTION ( 'NONE',  ( -1.000000000000000000, 0.000000000000000000, -0.000000000000000000 ) ) ;
#16869 = ORIENTED_EDGE ( 'NONE', *, *, #49046, .F. ) ;
#16870 = CARTESIAN_POINT ( 'NONE',  ( 15.80042947435468470, -175.3837268820161057, 107.2060569716377927 ) ) ;
#16871 = CARTESIAN_POINT ( 'NONE',  ( -339.1964088526558498, -116.8846903019842927, 58.63009191191280678 ) ) ;
#16872 = ORIENTED_EDGE ( 'NONE', *, *, #15046, .T. ) ;
#16873 = CARTESIAN_POINT ( 'NONE',  ( 46.40005841627164074, -177.1207230881787780, 81.38144888055276738 ) ) ;
#16874 = FACE_OUTER_BOUND ( 'NONE', #6178, .T. ) ;
#16875 = VECTOR ( 'NONE', #46541, 1000.000000000000000 ) ;
#16876 = DIRECTION ( 'NONE',  ( -0.000000000000000000, 1.000000000000000000, -0.000000000000000000 ) ) ;
#16877 = EDGE_CURVE ( 'NONE', #30392, #5462, #23111, .T. ) ;
#16878 = CARTESIAN_POINT ( 'NONE',  ( -60.00000000000000000, 20.00000000000000000, -60.00000000000000711 ) ) ;
#16879 = CARTESIAN_POINT ( 'NONE',  ( -336.3521761649654422, -180.3949349376675855, 15.70448169564087770 ) ) ;
#16880 = EDGE_CURVE ( 'NONE', #12738, #13511, #18901, .T. ) ;
#16881 = AXIS2_PLACEMENT_3D ( 'NONE', #5514, #18105, #2061 ) ;
#16882 = LINE ( 'NONE', #17414, #48962 ) ;
#16883 = DIRECTION ( 'NONE',  ( -0.000000000000000000, 1.000000000000000000, -0.000000000000000000 ) ) ;
#16884 = DIRECTION ( 'NONE',  ( 0.6965510290629982615, 0.000000000000000000, -0.7175072570443298270 ) ) ;
#16886 = ORIENTED_EDGE ( 'NONE', *, *, #24744, .F. ) ;
#16885 = DIRECTION ( 'NONE',  ( -1.000000000000000000, 1.013386094502320512E-14, -2.497772389992655628E-15 ) ) ;
#16887 = ORIENTED_EDGE ( 'NONE', *, *, #13934, .F. ) ;
#16888 = CARTESIAN_POINT ( 'NONE',  ( 56.77503207194101265, -193.5000000000000000, -67.42819922234311036 ) ) ;
#16889 = EDGE_CURVE ( 'NONE', #3837, #4082, #19413, .T. ) ;
#16890 = EDGE_CURVE ( 'NONE', #31952, #17151, #35183, .T. ) ;
#16891 = CARTESIAN_POINT ( 'NONE',  ( 73.03012110230136500, -189.7472609257535510, 24.72869175143112130 ) ) ;
#16892 = EDGE_LOOP ( 'NONE', ( #50807, #43140, #3143, #44430 ) ) ;
#16893 = ORIENTED_EDGE ( 'NONE', *, *, #15418, .F. ) ;
#16894 = EDGE_CURVE ( 'NONE', #49449, #36064, #7079, .T. ) ;
#16895 = VECTOR ( 'NONE', #16373, 1000.000000000000114 ) ;
#16896 = VERTEX_POINT ( 'NONE', #23373 ) ;
#16897 = DIRECTION ( 'NONE',  ( 0.8757349421956345248, 0.000000000000000000, 0.4827922027307490205 ) ) ;
#16898 = DIRECTION ( 'NONE',  ( 0.000000000000000000, 0.000000000000000000, 1.000000000000000000 ) ) ;
#16899 = LINE ( 'NONE', #49222, #10681 ) ;
#16900 = ORIENTED_EDGE ( 'NONE', *, *, #10816, .F. ) ;
#16901 = ORIENTED_EDGE ( 'NONE', *, *, #51658, .T. ) ;
#16902 = CARTESIAN_POINT ( 'NONE',  ( 76.51419089073348800, -183.6283474603465606, -1.292495564988658030 ) ) ;
#16904 = VERTEX_POINT ( 'NONE', #11261 ) ;
#16903 = DIRECTION ( 'NONE',  ( -0.000000000000000000, 1.000000000000000000, -0.000000000000000000 ) ) ;
#16905 = DIRECTION ( 'NONE',  ( 0.4031234292879730674, 0.000000000000000000, -0.9151456172430181280 ) ) ;
#16906 = ORIENTED_EDGE ( 'NONE', *, *, #30478, .T. ) ;
#16907 = DIRECTION ( 'NONE',  ( 0.000000000000000000, 0.000000000000000000, 1.000000000000000000 ) ) ;
#16908 = VECTOR ( 'NONE', #46413, 1000.000000000000000 ) ;
#16909 = ORIENTED_EDGE ( 'NONE', *, *, #41659, .F. ) ;
#16910 = CARTESIAN_POINT ( 'NONE',  ( -169.1033029113419559, -175.3837268820161057, 32.78426643622745473 ) ) ;
#16911 = CARTESIAN_POINT ( 'NONE',  ( 21.49274850782854074, -175.3837268820161057, -103.5805805771126700 ) ) ;
#16912 = LINE ( 'NONE', #15884, #50095 ) ;
#16913 = VECTOR ( 'NONE', #28035, 1000.000000000000227 ) ;
#16914 = VERTEX_POINT ( 'NONE', #51487 ) ;
#16915 = EDGE_LOOP ( 'NONE', ( #21760, #45758 ) ) ;
#16916 = CARTESIAN_POINT ( 'NONE',  ( -339.1964088526558498, -89.57268800991437274, 48.27201571435973904 ) ) ;
#16917 = CARTESIAN_POINT ( 'NONE',  ( -332.3517673607765914, -148.5878911270064009, 53.46519113769075204 ) ) ;
#16918 = ORIENTED_EDGE ( 'NONE', *, *, #31283, .T. ) ;
#16919 = CARTESIAN_POINT ( 'NONE',  ( 74.61260187273137490, -193.5000000000000000, -14.98512977653175682 ) ) ;
#16920 = LINE ( 'NONE', #28722, #41327 ) ;
#16921 = EDGE_LOOP ( 'NONE', ( #10297, #28074, #32477, #47603 ) ) ;
#16922 = FACE_BOUND ( 'NONE', #5121, .T. ) ;
#16923 = CIRCLE ( 'NONE', #32848, 125.0000000000000000 ) ;
#16924 = CARTESIAN_POINT ( 'NONE',  ( -48.47912675150885065, -189.7472609257535510, 6.938893903907228378E-15 ) ) ;
#16925 = EDGE_LOOP ( 'NONE', ( #8767, #41803, #40760, #48710 ) ) ;
#16926 = DIRECTION ( 'NONE',  ( -0.000000000000000000, 1.000000000000000000, -0.000000000000000000 ) ) ;
#16927 = ORIENTED_EDGE ( 'NONE', *, *, #43261, .T. ) ;
#16928 = FACE_BOUND ( 'NONE', #1380, .T. ) ;
#16929 = VECTOR ( 'NONE', #38661, 1000.000000000000000 ) ;
#16930 = CARTESIAN_POINT ( 'NONE',  ( 76.01188277843579044, -175.3837268820161057, 11.26891947860284482 ) ) ;
#16931 = ORIENTED_EDGE ( 'NONE', *, *, #48077, .T. ) ;
#16932 = ADVANCED_FACE ( 'NONE', ( #27294 ), #39379, .T. ) ;
#16933 = FACE_OUTER_BOUND ( 'NONE', #30247, .T. ) ;
#16934 = EDGE_CURVE ( 'NONE', #34425, #7329, #460, .T. ) ;
#16935 = DIRECTION ( 'NONE',  ( 0.000000000000000000, 0.000000000000000000, -1.000000000000000000 ) ) ;
#16936 = FACE_OUTER_BOUND ( 'NONE', #18759, .T. ) ;
#16937 = ADVANCED_FACE ( 'NONE', ( #36468 ), #749, .T. ) ;
#16938 = CARTESIAN_POINT ( 'NONE',  ( -172.9701362814535912, -193.5000000000000000, -11.26891947860193177 ) ) ;
#16939 = ADVANCED_FACE ( 'NONE', ( #21243 ), #20717, .T. ) ;
#16940 = ORIENTED_EDGE ( 'NONE', *, *, #46503, .T. ) ;
#16941 = LINE ( 'NONE', #9059, #16083 ) ;
#16942 = ORIENTED_EDGE ( 'NONE', *, *, #25036, .F. ) ;
#16943 = VERTEX_POINT ( 'NONE', #45176 ) ;
#16944 = DIRECTION ( 'NONE',  ( 0.000000000000000000, 0.000000000000000000, 1.000000000000000000 ) ) ;
#16946 = ORIENTED_EDGE ( 'NONE', *, *, #42376, .T. ) ;
#16945 = DIRECTION ( 'NONE',  ( 0.000000000000000000, 0.000000000000000000, -1.000000000000000000 ) ) ;
#16947 = EDGE_CURVE ( 'NONE', #48520, #16369, #8373, .T. ) ;
#16948 = AXIS2_PLACEMENT_3D ( 'NONE', #8701, #16326, #24466 ) ;
#16949 = ORIENTED_EDGE ( 'NONE', *, *, #8664, .T. ) ;
#16950 = CARTESIAN_POINT ( 'NONE',  ( -336.3521761649654422, -67.75522407825191351, 19.39547174791671935 ) ) ;
#16951 = EDGE_CURVE ( 'NONE', #43961, #31341, #21489, .T. ) ;
#16952 = AXIS2_PLACEMENT_3D ( 'NONE', #27451, #35084, #24031 ) ;
#16953 = ADVANCED_FACE ( 'NONE', ( #16527 ), #24156, .T. ) ;
#16954 = VECTOR ( 'NONE', #48161, 1000.000000000000000 ) ;
#16955 = DIRECTION ( 'NONE',  ( 0.000000000000000000, -0.000000000000000000, 1.000000000000000000 ) ) ;
#16956 = DIRECTION ( 'NONE',  ( 0.6068001458185890984, 0.000000000000000000, 0.7948544414133565938 ) ) ;
#16957 = ORIENTED_EDGE ( 'NONE', *, *, #906, .T. ) ;
#16958 = ADVANCED_FACE ( 'NONE', ( #4177 ), #20984, .T. ) ;
#16959 = CARTESIAN_POINT ( 'NONE',  ( 5.542374969221969039, -183.6283474603465606, 112.7238987608088223 ) ) ;
#16960 = EDGE_LOOP ( 'NONE', ( #23064, #13494, #2183, #2258 ) ) ;
#16961 = CARTESIAN_POINT ( 'NONE',  ( 59.80284513346456521, -183.6283474603465606, 62.45009659481583952 ) ) ;
#16962 = FACE_OUTER_BOUND ( 'NONE', #335, .T. ) ;
#16963 = ADVANCED_FACE ( 'NONE', ( #16008 ), #33054, .T. ) ;
#16964 = DIRECTION ( 'NONE',  ( 1.043714542225393539E-14, -0.8854560256532079121, 0.4647231720437725033 ) ) ;
#16965 = DIRECTION ( 'NONE',  ( 0.000000000000000000, -1.000000000000000000, 0.000000000000000000 ) ) ;
#16966 = VERTEX_POINT ( 'NONE', #12569 ) ;
#16967 = VECTOR ( 'NONE', #7177, 1000.000000000000000 ) ;
#16968 = ORIENTED_EDGE ( 'NONE', *, *, #24024, .T. ) ;
#16969 = ORIENTED_EDGE ( 'NONE', *, *, #11551, .T. ) ;
#16970 = FACE_OUTER_BOUND ( 'NONE', #26429, .T. ) ;
#16971 = CARTESIAN_POINT ( 'NONE',  ( -339.1964088526558498, -157.4273119900853146, -48.27201571435997352 ) ) ;
#16972 = AXIS2_PLACEMENT_3D ( 'NONE', #13111, #40685, #9183 ) ;
#16973 = CIRCLE ( 'NONE', #27858, 125.0000000000000000 ) ;
#16974 = PLANE ( 'NONE',  #767 ) ;
#16975 = FACE_BOUND ( 'NONE', #22913, .T. ) ;
#16976 = CARTESIAN_POINT ( 'NONE',  ( -48.93575598890257794, -189.7472609257535510, 0.8896570909947506545 ) ) ;
#16977 = VERTEX_POINT ( 'NONE', #28844 ) ;
#16978 = EDGE_CURVE ( 'NONE', #11613, #2690, #36217, .T. ) ;
#16979 = ORIENTED_EDGE ( 'NONE', *, *, #33907, .T. ) ;
#16981 = VERTEX_POINT ( 'NONE', #16256 ) ;
#16980 = LINE ( 'NONE', #49034, #5558 ) ;
#16982 = ORIENTED_EDGE ( 'NONE', *, *, #22212, .F. ) ;
#16983 = FACE_OUTER_BOUND ( 'NONE', #25589, .T. ) ;
#16984 = CARTESIAN_POINT ( 'NONE',  ( -172.7479958471414250, -183.6283474603465606, -13.49993235881364129 ) ) ;
#16985 = AXIS2_PLACEMENT_3D ( 'NONE', #7603, #16268, #44118 ) ;
#16986 = DIRECTION ( 'NONE',  ( -0.000000000000000000, 1.000000000000000000, -0.000000000000000000 ) ) ;
#16987 = DIRECTION ( 'NONE',  ( 0.000000000000000000, 0.000000000000000000, 1.000000000000000000 ) ) ;
#16988 = ORIENTED_EDGE ( 'NONE', *, *, #6736, .T. ) ;
#16989 = CARTESIAN_POINT ( 'NONE',  ( -172.0839188101925004, -193.5000000000000000, -18.62405380494756812 ) ) ;
#16990 = ORIENTED_EDGE ( 'NONE', *, *, #49795, .F. ) ;
#16991 = AXIS2_PLACEMENT_3D ( 'NONE', #7879, #20233, #39168 ) ;
#16992 = EDGE_CURVE ( 'NONE', #9008, #1918, #44897, .T. ) ;
#16993 = EDGE_LOOP ( 'NONE', ( #29890, #13700, #1705, #41413 ) ) ;
#16994 = DIRECTION ( 'NONE',  ( -0.6300878435817203194, 0.000000000000000000, 0.7765238627180349740 ) ) ;
#16995 = CARTESIAN_POINT ( 'NONE',  ( -336.3521761649654422, -68.91285928486892942, -22.44790492310182017 ) ) ;
#16996 = EDGE_CURVE ( 'NONE', #13092, #41341, #40164, .T. ) ;
#16997 = EDGE_CURVE ( 'NONE', #21200, #43863, #24827, .T. ) ;
#16998 = PLANE ( 'NONE',  #11377 ) ;
#16999 = ADVANCED_FACE ( 'NONE', ( #41196 ), #4689, .F. ) ;
#17000 = DIRECTION ( 'NONE',  ( 0.000000000000000000, -1.000000000000000000, -0.000000000000000000 ) ) ;
#17001 = CARTESIAN_POINT ( 'NONE',  ( 9.336583202542589888, -193.5000000000000000, 110.8257356506556306 ) ) ;
#17002 = EDGE_CURVE ( 'NONE', #34569, #5750, #48319, .T. ) ;
#17003 = ORIENTED_EDGE ( 'NONE', *, *, #50643, .F. ) ;
#17004 = CARTESIAN_POINT ( 'NONE',  ( -336.3521761649653854, -64.87442053112221174, 12.76876783163883111 ) ) ;
#17005 = FACE_OUTER_BOUND ( 'NONE', #45565, .T. ) ;
#17006 = AXIS2_PLACEMENT_3D ( 'NONE', #11579, #31025, #27604 ) ;
#17007 = EDGE_CURVE ( 'NONE', #11775, #19173, #24396, .T. ) ;
#17008 = DIRECTION ( 'NONE',  ( 0.000000000000000000, 1.000000000000000000, 0.000000000000000000 ) ) ;
#17009 = FACE_BOUND ( 'NONE', #4870, .T. ) ;
#17010 = ORIENTED_EDGE ( 'NONE', *, *, #44359, .F. ) ;
#17011 = VECTOR ( 'NONE', #45127, 1000.000000000000000 ) ;
#17012 = VECTOR ( 'NONE', #14040, 1000.000000000000000 ) ;
#17013 = EDGE_CURVE ( 'NONE', #18653, #39568, #32801, .T. ) ;
#17014 = LINE ( 'NONE', #33021, #15554 ) ;
#17015 = ORIENTED_EDGE ( 'NONE', *, *, #18589, .T. ) ;
#17016 = DIRECTION ( 'NONE',  ( 0.000000000000000000, -1.000000000000000000, 0.000000000000000000 ) ) ;
#17017 = VERTEX_POINT ( 'NONE', #40941 ) ;
#17018 = DIRECTION ( 'NONE',  ( -1.000000000000000000, 0.000000000000000000, 0.000000000000000000 ) ) ;
#17019 = ADVANCED_FACE ( 'NONE', ( #31122 ), #6709, .F. ) ;
#17020 = ORIENTED_EDGE ( 'NONE', *, *, #39545, .F. ) ;
#17021 = EDGE_CURVE ( 'NONE', #5202, #32592, #51130, .T. ) ;
#17022 = DIRECTION ( 'NONE',  ( 0.000000000000000000, 1.000000000000000000, 0.000000000000000000 ) ) ;
#17023 = EDGE_CURVE ( 'NONE', #23880, #1605, #6457, .T. ) ;
#17024 = FACE_OUTER_BOUND ( 'NONE', #26952, .T. ) ;
#17026 = VERTEX_POINT ( 'NONE', #38501 ) ;
#17025 = DIRECTION ( 'NONE',  ( 0.8858462335218260097, -0.000000000000000000, -0.4639789333096864810 ) ) ;
#17027 = AXIS2_PLACEMENT_3D ( 'NONE', #50097, #30106, #42443 ) ;
#17028 = EDGE_CURVE ( 'NONE', #10986, #8881, #34295, .T. ) ;
#17029 = CARTESIAN_POINT ( 'NONE',  ( -171.7589556598192644, -193.5000000000000000, -13.35228579481115574 ) ) ;
#17030 = ORIENTED_EDGE ( 'NONE', *, *, #5067, .F. ) ;
#17031 = EDGE_LOOP ( 'NONE', ( #1273, #23457, #36275, #8007 ) ) ;
#17032 = EDGE_CURVE ( 'NONE', #6808, #48562, #30702, .T. ) ;
#17033 = CIRCLE ( 'NONE', #48081, 60.00000000000000000 ) ;
#17034 = ORIENTED_EDGE ( 'NONE', *, *, #29928, .F. ) ;
#17035 = CARTESIAN_POINT ( 'NONE',  ( -330.4913330509368166, -123.5000000000000284, 0.000000000000000000 ) ) ;
#17036 = DIRECTION ( 'NONE',  ( -0.9993203489176063492, 0.000000000000000000, -0.03686245026030391531 ) ) ;
#17037 = ORIENTED_EDGE ( 'NONE', *, *, #41308, .T. ) ;
#17038 = LINE ( 'NONE', #36456, #46063 ) ;
#17039 = FACE_OUTER_BOUND ( 'NONE', #34081, .T. ) ;
#17040 = CARTESIAN_POINT ( 'NONE',  ( -339.1964088526558498, -78.92247586332028675, -40.16023333901007675 ) ) ;
#17041 = AXIS2_PLACEMENT_3D ( 'NONE', #34694, #11803, #11285 ) ;
#17042 = VECTOR ( 'NONE', #38846, 1000.000000000000000 ) ;
#17043 = ADVANCED_FACE ( 'NONE', ( #50853 ), #10639, .T. ) ;
#17044 = LINE ( 'NONE', #24916, #25894 ) ;
#17045 = DIRECTION ( 'NONE',  ( -0.000000000000000000, 1.000000000000000000, -0.000000000000000000 ) ) ;
#17046 = ORIENTED_EDGE ( 'NONE', *, *, #41754, .T. ) ;
#17049 = ORIENTED_EDGE ( 'NONE', *, *, #33241, .T. ) ;
#17048 = DIRECTION ( 'NONE',  ( 0.000000000000000000, 0.1205366802553337752, 0.9927088740980526405 ) ) ;
#17047 = CARTESIAN_POINT ( 'NONE',  ( -74.33510315702947935, -193.5000000000000000, -121.2748789083718606 ) ) ;
#17050 = AXIS2_PLACEMENT_3D ( 'NONE', #27980, #51927, #24047 ) ;
#17051 = VECTOR ( 'NONE', #2196, 1000.000000000000114 ) ;
#17052 = EDGE_LOOP ( 'NONE', ( #14438, #38483 ) ) ;
#17053 = DIRECTION ( 'NONE',  ( 1.043714542225393223E-14, -0.3546048870425300148, 0.9350162426854169428 ) ) ;
#17054 = ORIENTED_EDGE ( 'NONE', *, *, #42682, .F. ) ;
#17055 = DIRECTION ( 'NONE',  ( 0.000000000000000000, 0.7485107481711089639, 0.6631226582407863113 ) ) ;
#17056 = ORIENTED_EDGE ( 'NONE', *, *, #29075, .F. ) ;
#17057 = LINE ( 'NONE', #49108, #49834 ) ;
#17058 = CLOSED_SHELL ( 'NONE', ( #31400, #24049, #29581, #25027, #51314, #40398, #26693, #31044, #13137, #24343, #26556, #610, #45273, #49490, #44587, #11753, #10425, #50405, #29293, #20482, #25479, #37895, #19524, #31142, #40186, #35954, #43324, #7334, #34253, #29817, #39417, #30173, #41188, #28477 ) ) ;
#17059 = DIRECTION ( 'NONE',  ( 0.000000000000000000, 0.6631226582407911962, -0.7485107481711046340 ) ) ;
#17060 = ORIENTED_EDGE ( 'NONE', *, *, #49362, .F. ) ;
#17061 = DIRECTION ( 'NONE',  ( 0.000000000000000000, 0.000000000000000000, -1.000000000000000000 ) ) ;
#17062 = ORIENTED_EDGE ( 'NONE', *, *, #44831, .F. ) ;
#17063 = VERTEX_POINT ( 'NONE', #30873 ) ;
#17064 = DIRECTION ( 'NONE',  ( -0.000000000000000000, 1.000000000000000000, -0.000000000000000000 ) ) ;
#17065 = DIRECTION ( 'NONE',  ( 0.000000000000000000, 0.000000000000000000, 1.000000000000000000 ) ) ;
#17066 = DIRECTION ( 'NONE',  ( -0.000000000000000000, 1.000000000000000000, 0.000000000000000000 ) ) ;
#17067 = FACE_OUTER_BOUND ( 'NONE', #954, .T. ) ;
#17068 = VERTEX_POINT ( 'NONE', #14860 ) ;
#17069 = VECTOR ( 'NONE', #46535, 1000.000000000000000 ) ;
#17070 = DIRECTION ( 'NONE',  ( 0.000000000000000000, 0.000000000000000000, -1.000000000000000000 ) ) ;
#17071 = ADVANCED_FACE ( 'NONE', ( #22728 ), #38736, .F. ) ;
#17072 = EDGE_CURVE ( 'NONE', #36128, #29872, #34793, .T. ) ;
#17073 = PRODUCT_CONTEXT ( 'NONE', #44796, 'mechanical' ) ;
#17074 = CARTESIAN_POINT ( 'NONE',  ( -336.3521761649654422, -169.4076645216271402, -37.15394033962039089 ) ) ;
#17075 = CARTESIAN_POINT ( 'NONE',  ( -166.8403286750647680, -193.5000000000000000, -40.19484891389966918 ) ) ;
#17076 = DIRECTION ( 'NONE',  ( 0.000000000000000000, 0.9927088740980544168, 0.1205366802553199251 ) ) ;
#17077 = DIRECTION ( 'NONE',  ( 0.000000000000000000, 0.000000000000000000, 1.000000000000000000 ) ) ;
#17078 = AXIS2_PLACEMENT_3D ( 'NONE', #23979, #39489, #43953 ) ;
#17079 = FACE_OUTER_BOUND ( 'NONE', #722, .T. ) ;
#17080 = EDGE_LOOP ( 'NONE', ( #33834, #36318, #42024, #48546 ) ) ;
#17081 = LINE ( 'NONE', #13121, #37835 ) ;
#17082 = DIRECTION ( 'NONE',  ( 0.000000000000000000, 0.6631226582408039638, 0.7485107481710934207 ) ) ;
#17083 = EDGE_LOOP ( 'NONE', ( #51061, #43074, #34220, #37708 ) ) ;
#17084 = ORIENTED_EDGE ( 'NONE', *, *, #50875, .F. ) ;
#17085 = VECTOR ( 'NONE', #10522, 1000.000000000000000 ) ;
#17086 = ORIENTED_EDGE ( 'NONE', *, *, #49179, .T. ) ;
#17087 = LINE ( 'NONE', #20232, #32638 ) ;
#17088 = AXIS2_PLACEMENT_3D ( 'NONE', #32886, #36575, #44732 ) ;
#17089 = CARTESIAN_POINT ( 'NONE',  ( -150.5215542367829471, -193.5000000000000000, -72.19655804061974891 ) ) ;
#17090 = EDGE_CURVE ( 'NONE', #25917, #41928, #26918, .T. ) ;
#17091 = DIRECTION ( 'NONE',  ( 0.000000000000000000, 0.000000000000000000, 1.000000000000000000 ) ) ;
#17092 = CARTESIAN_POINT ( 'NONE',  ( -34.51936650669026818, -175.3837268820161057, -124.2180546213278234 ) ) ;
#17093 = ORIENTED_EDGE ( 'NONE', *, *, #19711, .F. ) ;
#17094 = DIRECTION ( 'NONE',  ( 1.000000000000000000, -0.000000000000000000, -0.000000000000000000 ) ) ;
#17095 = CIRCLE ( 'NONE', #1118, 124.9999999999999858 ) ;
#17096 = DIRECTION ( 'NONE',  ( 0.000000000000000000, 1.000000000000000000, 0.000000000000000000 ) ) ;
#17097 = ORIENTED_EDGE ( 'NONE', *, *, #8354, .T. ) ;
#17098 = EDGE_CURVE ( 'NONE', #2088, #14462, #22986, .T. ) ;
#17099 = CARTESIAN_POINT ( 'NONE',  ( 12.99855592850622443, -183.6283474603465606, 108.8370090194294875 ) ) ;
#17100 = ORIENTED_EDGE ( 'NONE', *, *, #9979, .F. ) ;
#17101 = DIRECTION ( 'NONE',  ( 0.000000000000000000, -1.000000000000000000, 0.000000000000000000 ) ) ;
#17102 = VERTEX_POINT ( 'NONE', #50279 ) ;
#17103 = FACE_OUTER_BOUND ( 'NONE', #6822, .T. ) ;
#17104 = CIRCLE ( 'NONE', #27992, 125.0000000000000000 ) ;
#17105 = VECTOR ( 'NONE', #36854, 999.9999999999998863 ) ;
#17106 = LINE ( 'NONE', #29424, #22533 ) ;
#17107 = CARTESIAN_POINT ( 'NONE',  ( -305.0000000000000568, -156.2279223070262049, 50.28800156563451651 ) ) ;
#17110 = VERTEX_POINT ( 'NONE', #26341 ) ;
#17109 = DIRECTION ( 'NONE',  ( 0.000000000000000000, 0.000000000000000000, -1.000000000000000000 ) ) ;
#17108 = DIRECTION ( 'NONE',  ( -0.000000000000000000, -0.8854560256532126861, -0.4647231720437631775 ) ) ;
#17111 = DIRECTION ( 'NONE',  ( -1.000000000000000000, -0.000000000000000000, -0.000000000000000000 ) ) ;
#17112 = ORIENTED_EDGE ( 'NONE', *, *, #49159, .T. ) ;
#17113 = DIRECTION ( 'NONE',  ( -0.000000000000000000, 1.000000000000000000, -0.000000000000000000 ) ) ;
#17114 = CARTESIAN_POINT ( 'NONE',  ( -339.1964088526558498, -95.63860483659040312, 52.00954392751717847 ) ) ;
#17115 = ORIENTED_EDGE ( 'NONE', *, *, #23536, .T. ) ;
#17116 = DIRECTION ( 'NONE',  ( 0.000000000000000000, 0.000000000000000000, -1.000000000000000000 ) ) ;
#17118 = LINE ( 'NONE', #32086, #27326 ) ;
#17117 = LINE ( 'NONE', #46018, #34989 ) ;
#17119 = AXIS2_PLACEMENT_3D ( 'NONE', #7906, #47098, #35503 ) ;
#17120 = ORIENTED_EDGE ( 'NONE', *, *, #7892, .F. ) ;
#17121 = DIRECTION ( 'NONE',  ( -0.000000000000000000, 1.000000000000000000, -0.000000000000000000 ) ) ;
#17122 = DIRECTION ( 'NONE',  ( 0.000000000000000000, 0.8805628084623552398, -0.4739294676984008858 ) ) ;
#17123 = DIRECTION ( 'NONE',  ( 0.000000000000000000, -0.000000000000000000, 1.000000000000000000 ) ) ;
#17124 = ORIENTED_EDGE ( 'NONE', *, *, #15267, .F. ) ;
#17125 = CARTESIAN_POINT ( 'NONE',  ( -51.89154260666841623, -183.6283474603465606, 124.9534129907280970 ) ) ;
#17126 = DIRECTION ( 'NONE',  ( -0.000000000000000000, -1.000000000000000000, 0.000000000000000000 ) ) ;
#17127 = DIRECTION ( 'NONE',  ( 0.000000000000000000, 0.000000000000000000, 1.000000000000000000 ) ) ;
#17128 = ORIENTED_EDGE ( 'NONE', *, *, #35937, .F. ) ;
#17129 = ADVANCED_FACE ( 'NONE', ( #22409 ), #43142, .T. ) ;
#17130 = CARTESIAN_POINT ( 'NONE',  ( -172.0839188101924719, -189.7472609257535510, -18.62405380494754681 ) ) ;
#17131 = CARTESIAN_POINT ( 'NONE',  ( -170.0000000000000284, -155.0173647354142759, -14.76740078976489201 ) ) ;
#17132 = DIRECTION ( 'NONE',  ( 0.000000000000000000, -1.000000000000000000, 0.000000000000000000 ) ) ;
#17133 = ORIENTED_EDGE ( 'NONE', *, *, #10514, .T. ) ;
#17134 = DIRECTION ( 'NONE',  ( 0.000000000000000000, 0.3546048870425331234, -0.9350162426854158326 ) ) ;
#17135 = PLANE ( 'NONE',  #42890 ) ;
#17136 = VECTOR ( 'NONE', #27586, 1000.000000000000000 ) ;
#17137 = PLANE ( 'NONE',  #21871 ) ;
#17138 = PLANE ( 'NONE',  #41724 ) ;
#17139 = AXIS2_PLACEMENT_3D ( 'NONE', #21453, #17530, #36962 ) ;
#17140 = PLANE ( 'NONE',  #15391 ) ;
#17141 = DIRECTION ( 'NONE',  ( 0.000000000000000000, 0.000000000000000000, 1.000000000000000000 ) ) ;
#17142 = ADVANCED_FACE ( 'NONE', ( #7148 ), #47102, .F. ) ;
#17143 = CARTESIAN_POINT ( 'NONE',  ( -332.3517673607765914, -98.41210887299327226, -53.46519113769058151 ) ) ;
#17145 = ORIENTED_EDGE ( 'NONE', *, *, #45415, .T. ) ;
#17144 = CARTESIAN_POINT ( 'NONE',  ( 52.98246549829696761, -189.7472609257535510, 73.01058346660535392 ) ) ;
#17146 = EDGE_LOOP ( 'NONE', ( #41694, #2385, #23378, #51127 ) ) ;
#17147 = CARTESIAN_POINT ( 'NONE',  ( -153.2421220336517251, -189.7472609257535510, -66.33788548805453900 ) ) ;
#17148 = CIRCLE ( 'NONE', #14598, 125.0000000000000000 ) ;
#17149 = CARTESIAN_POINT ( 'NONE',  ( -170.0000000000000284, -113.5000000000000000, -40.00000000000001421 ) ) ;
#17151 = VERTEX_POINT ( 'NONE', #23945 ) ;
#17150 = CARTESIAN_POINT ( 'NONE',  ( -75.31296732259116311, -177.1207230881787780, -121.0625654437172614 ) ) ;
#17152 = ORIENTED_EDGE ( 'NONE', *, *, #22179, .T. ) ;
#17153 = ORIENTED_EDGE ( 'NONE', *, *, #48831, .F. ) ;
#17154 = PLANE ( 'NONE',  #34267 ) ;
#17155 = DIRECTION ( 'NONE',  ( 1.000000000000000000, 0.000000000000000000, 0.000000000000000000 ) ) ;
#17156 = CARTESIAN_POINT ( 'NONE',  ( -170.9669310976187830, -175.3837268820161057, -24.93467037017131105 ) ) ;
#17157 = VERTEX_POINT ( 'NONE', #19739 ) ;
#17158 = FACE_OUTER_BOUND ( 'NONE', #1195, .T. ) ;
#17160 = ORIENTED_EDGE ( 'NONE', *, *, #16170, .F. ) ;
#17159 = DIRECTION ( 'NONE',  ( 0.000000000000000000, 0.000000000000000000, 1.000000000000000000 ) ) ;
#17161 = DIRECTION ( 'NONE',  ( 0.000000000000000000, 0.000000000000000000, 1.000000000000000000 ) ) ;
#17162 = VECTOR ( 'NONE', #15881, 1000.000000000000114 ) ;
#17163 = ORIENTED_EDGE ( 'NONE', *, *, #46193, .F. ) ;
#17164 = DIRECTION ( 'NONE',  ( -1.000000000000000000, 0.000000000000000000, 0.000000000000000000 ) ) ;
#17165 = VERTEX_POINT ( 'NONE', #39451 ) ;
#17166 = CIRCLE ( 'NONE', #3720, 20.00000000000001776 ) ;
#17167 = EDGE_CURVE ( 'NONE', #29891, #44801, #47626, .T. ) ;
#17168 = CARTESIAN_POINT ( 'NONE',  ( -164.6073096293132494, -193.5000000000000000, 43.47841891815210147 ) ) ;
#17169 = CARTESIAN_POINT ( 'NONE',  ( -48.47912675150885065, -189.7472609257535510, 6.938893903907228378E-15 ) ) ;
#17170 = FACE_OUTER_BOUND ( 'NONE', #13506, .T. ) ;
#17171 = VECTOR ( 'NONE', #9561, 1000.000000000000000 ) ;
#17172 = EDGE_CURVE ( 'NONE', #5492, #25744, #48130, .T. ) ;
#17173 = ORIENTED_EDGE ( 'NONE', *, *, #17253, .T. ) ;
#17174 = ORIENTED_EDGE ( 'NONE', *, *, #7668, .F. ) ;
#17175 = LINE ( 'NONE', #5094, #34846 ) ;
#17176 = CARTESIAN_POINT ( 'NONE',  ( -155.0851258170080769, -177.1207230881787780, 63.33473559879987391 ) ) ;
#17177 = ORIENTED_EDGE ( 'NONE', *, *, #23912, .T. ) ;
#17178 = CARTESIAN_POINT ( 'NONE',  ( -145.4373324222574126, -175.3837268820161057, -78.89300572996837957 ) ) ;
#17179 = LINE ( 'NONE', #12694, #22883 ) ;
#17180 = EDGE_LOOP ( 'NONE', ( #13403, #4495, #42494, #4739 ) ) ;
#17181 = EDGE_CURVE ( 'NONE', #46692, #25869, #15556, .T. ) ;
#17182 = DIRECTION ( 'NONE',  ( -0.000000000000000000, 1.000000000000000000, 0.000000000000000000 ) ) ;
#17183 = VECTOR ( 'NONE', #48775, 1000.000000000000000 ) ;
#17184 = ADVANCED_FACE ( 'NONE', ( #39205 ), #15830, .F. ) ;
#17185 = LINE ( 'NONE', #33200, #47429 ) ;
#17186 = PRODUCT_DEFINITION_SHAPE ( 'NONE', 'NONE',  #8752 ) ;
#17187 = ORIENTED_EDGE ( 'NONE', *, *, #6971, .F. ) ;
#17188 = CARTESIAN_POINT ( 'NONE',  ( -336.3521761649654422, -94.63601285149479736, 51.48334306143172512 ) ) ;
#17189 = ORIENTED_EDGE ( 'NONE', *, *, #49158, .F. ) ;
#17190 = ADVANCED_FACE ( 'NONE', ( #39698 ), #3712, .F. ) ;
#17191 = CARTESIAN_POINT ( 'NONE',  ( 0.000000000000000000, -64.50000000000000000, 0.000000000000000000 ) ) ;
#17192 = CARTESIAN_POINT ( 'NONE',  ( -48.47912675150885065, -175.3837268820161057, 6.938893903907228378E-15 ) ) ;
#17193 = ORIENTED_EDGE ( 'NONE', *, *, #9226, .T. ) ;
#17194 = PLANE ( 'NONE',  #40785 ) ;
#17195 = DIRECTION ( 'NONE',  ( 0.000000000000000000, -1.000000000000000000, 0.000000000000000000 ) ) ;
#17196 = DIRECTION ( 'NONE',  ( 0.000000000000000000, -1.000000000000000000, 0.000000000000000000 ) ) ;
#17197 = LINE ( 'NONE', #13254, #32455 ) ;
#17198 = ORIENTED_EDGE ( 'NONE', *, *, #39121, .T. ) ;
#17199 = DIRECTION ( 'NONE',  ( 0.2348860457809775482, 0.000000000000000000, 0.9720229140804121926 ) ) ;
#17200 = ORIENTED_EDGE ( 'NONE', *, *, #8864, .F. ) ;
#17201 = ORIENTED_EDGE ( 'NONE', *, *, #22086, .T. ) ;
#17202 = EDGE_CURVE ( 'NONE', #23608, #47014, #18116, .T. ) ;
#17203 = CARTESIAN_POINT ( 'NONE',  ( 61.38599058177057799, -189.7472609257535510, 59.62093586438192006 ) ) ;
#17205 = ORIENTED_EDGE ( 'NONE', *, *, #50057, .T. ) ;
#17204 = DIRECTION ( 'NONE',  ( 0.000000000000000000, 0.000000000000000000, 1.000000000000000000 ) ) ;
#17206 = CIRCLE ( 'NONE', #26412, 15.00000000000000000 ) ;
#17207 = AXIS2_PLACEMENT_3D ( 'NONE', #15854, #39989, #39723 ) ;
#17208 = ORIENTED_EDGE ( 'NONE', *, *, #16071, .F. ) ;
#17209 = FACE_OUTER_BOUND ( 'NONE', #11705, .T. ) ;
#17210 = AXIS2_PLACEMENT_3D ( 'NONE', #32881, #6015, #14177 ) ;
#17211 = CARTESIAN_POINT ( 'NONE',  ( -336.3521761649654422, -132.2320517616439020, -58.37307289257706344 ) ) ;
#17212 = CARTESIAN_POINT ( 'NONE',  ( 33.25242634436025213, -189.7472609257535510, -94.57776286494160445 ) ) ;
#17213 = ORIENTED_EDGE ( 'NONE', *, *, #47048, .T. ) ;
#17214 = DIRECTION ( 'NONE',  ( 0.4031234292879665171, 0.000000000000000000, 0.9151456172430210145 ) ) ;
#17215 = AXIS2_PLACEMENT_3D ( 'NONE', #25693, #13868, #21494 ) ;
#17216 = VERTEX_POINT ( 'NONE', #11080 ) ;
#17217 = DIRECTION ( 'NONE',  ( -0.000000000000000000, 1.000000000000000000, -0.000000000000000000 ) ) ;
#17218 = DIRECTION ( 'NONE',  ( -0.9027978299657387629, 0.000000000000000000, -0.4300652022765304450 ) ) ;
#17219 = VECTOR ( 'NONE', #18254, 1000.000000000000000 ) ;
#17221 = CIRCLE ( 'NONE', #32278, 125.0000000000000000 ) ;
#17220 = FACE_OUTER_BOUND ( 'NONE', #22074, .T. ) ;
#17222 = CARTESIAN_POINT ( 'NONE',  ( 60.00000000000001421, -113.5000000000000000, 60.00000000000000711 ) ) ;
#17223 = ORIENTED_EDGE ( 'NONE', *, *, #36956, .T. ) ;
#17224 = ORIENTED_EDGE ( 'NONE', *, *, #22852, .F. ) ;
#17225 = ORIENTED_EDGE ( 'NONE', *, *, #47788, .F. ) ;
#17226 = CARTESIAN_POINT ( 'NONE',  ( 28.02885774092382221, -189.7472609257535510, 98.85104101073332572 ) ) ;
#17227 = DIRECTION ( 'NONE',  ( 0.000000000000000000, 0.000000000000000000, 1.000000000000000000 ) ) ;
#17228 = CARTESIAN_POINT ( 'NONE',  ( -339.1964088526558498, -123.5000000000000284, 0.000000000000000000 ) ) ;
#17229 = DIRECTION ( 'NONE',  ( 0.000000000000000000, -0.000000000000000000, -1.000000000000000000 ) ) ;
#17230 = ORIENTED_EDGE ( 'NONE', *, *, #30765, .T. ) ;
#17231 = EDGE_CURVE ( 'NONE', #25859, #38149, #36290, .T. ) ;
#17232 = EDGE_CURVE ( 'NONE', #4651, #23372, #15298, .T. ) ;
#17233 = EDGE_LOOP ( 'NONE', ( #44143, #15093, #50144, #20846 ) ) ;
#17235 = EDGE_LOOP ( 'NONE', ( #31305, #6523, #44038, #30955 ) ) ;
#17234 = DIRECTION ( 'NONE',  ( 0.000000000000000000, 0.000000000000000000, -1.000000000000000000 ) ) ;
#17236 = ORIENTED_EDGE ( 'NONE', *, *, #13722, .F. ) ;
#17237 = VECTOR ( 'NONE', #41537, 1000.000000000000000 ) ;
#17238 = FACE_OUTER_BOUND ( 'NONE', #29398, .T. ) ;
#17239 = DIRECTION ( 'NONE',  ( 0.000000000000000000, 1.000000000000000000, -0.000000000000000000 ) ) ;
#17240 = AXIS2_PLACEMENT_3D ( 'NONE', #22603, #50984, #18903 ) ;
#17241 = VECTOR ( 'NONE', #23461, 1000.000000000000000 ) ;
#17242 = DIRECTION ( 'NONE',  ( -0.000000000000000000, 1.000000000000000000, -0.000000000000000000 ) ) ;
#17243 = CARTESIAN_POINT ( 'NONE',  ( -330.4913330509368166, -171.7720157143599238, 33.92731199008539278 ) ) ;
#17244 = DIRECTION ( 'NONE',  ( 0.000000000000000000, 0.000000000000000000, -1.000000000000000000 ) ) ;
#17245 = ORIENTED_EDGE ( 'NONE', *, *, #3047, .T. ) ;
#17246 = EDGE_CURVE ( 'NONE', #18753, #43264, #38248, .T. ) ;
#17247 = DIRECTION ( 'NONE',  ( 0.000000000000000000, 0.000000000000000000, -1.000000000000000000 ) ) ;
#17248 = VERTEX_POINT ( 'NONE', #44186 ) ;
#17249 = VECTOR ( 'NONE', #49063, 1000.000000000000000 ) ;
#17250 = ADVANCED_FACE ( 'NONE', ( #23449 ), #47357, .T. ) ;
#17251 = VERTEX_POINT ( 'NONE', #4243 ) ;
#17252 = DIRECTION ( 'NONE',  ( 0.000000000000000000, -0.2393156642875448881, 0.9709418174260553425 ) ) ;
#17253 = EDGE_CURVE ( 'NONE', #48345, #32062, #20263, .T. ) ;
#17254 = AXIS2_PLACEMENT_3D ( 'NONE', #17757, #21947, #32984 ) ;
#17255 = DIRECTION ( 'NONE',  ( 0.000000000000000000, -0.000000000000000000, 1.000000000000000000 ) ) ;
#17256 = VERTEX_POINT ( 'NONE', #288 ) ;
#17257 = AXIS2_PLACEMENT_3D ( 'NONE', #50448, #29939, #45999 ) ;
#17258 = EDGE_CURVE ( 'NONE', #12090, #5922, #31056, .T. ) ;
#17259 = CARTESIAN_POINT ( 'NONE',  ( -330.4913330509368166, -123.5000000000000284, 0.000000000000000000 ) ) ;
#17260 = DIRECTION ( 'NONE',  ( 0.000000000000000000, 0.000000000000000000, 1.000000000000000000 ) ) ;
#17261 = FACE_OUTER_BOUND ( 'NONE', #8525, .T. ) ;
#17262 = CIRCLE ( 'NONE', #47453, 124.9999999999999858 ) ;
#17263 = DIRECTION ( 'NONE',  ( 0.000000000000000000, 0.000000000000000000, -1.000000000000000000 ) ) ;
#17264 = CARTESIAN_POINT ( 'NONE',  ( -180.0000000000000568, -123.5000000000000284, 6.938893903907228378E-15 ) ) ;
#17266 = VECTOR ( 'NONE', #32263, 1000.000000000000000 ) ;
#17265 = LINE ( 'NONE', #33282, #32003 ) ;
#17267 = CYLINDRICAL_SURFACE ( 'NONE', #6461, 4.999999999999997335 ) ;
#17268 = EDGE_LOOP ( 'NONE', ( #51582, #19668, #18867, #43535 ) ) ;
#17269 = CARTESIAN_POINT ( 'NONE',  ( -332.3517673607765914, -146.8829211657874794, -54.23253582808848705 ) ) ;
#17270 = VERTEX_POINT ( 'NONE', #11852 ) ;
#17271 = CARTESIAN_POINT ( 'NONE',  ( -336.3521761649654422, -163.8460225846223466, -43.07972642080364523 ) ) ;
#17272 = ORIENTED_EDGE ( 'NONE', *, *, #15396, .T. ) ;
#17273 = FACE_OUTER_BOUND ( 'NONE', #27730, .T. ) ;
#17274 = ORIENTED_EDGE ( 'NONE', *, *, #10555, .F. ) ;
#17275 = CARTESIAN_POINT ( 'NONE',  ( -53.47502265695599277, -177.1207230881787780, -123.9001241957025883 ) ) ;
#17276 = AXIS2_PLACEMENT_3D ( 'NONE', #3667, #37556, #1550 ) ;
#17277 = DIRECTION ( 'NONE',  ( -0.000000000000000000, 1.000000000000000000, -0.000000000000000000 ) ) ;
#17279 = EDGE_LOOP ( 'NONE', ( #16761, #46333, #25505, #45585 ) ) ;
#17278 = DIRECTION ( 'NONE',  ( 0.000000000000000000, 0.000000000000000000, 1.000000000000000000 ) ) ;
#17280 = AXIS2_PLACEMENT_3D ( 'NONE', #7428, #35007, #27109 ) ;
#17281 = VECTOR ( 'NONE', #38447, 1000.000000000000000 ) ;
#17282 = DIRECTION ( 'NONE',  ( 0.000000000000000000, 0.000000000000000000, 1.000000000000000000 ) ) ;
#17283 = EDGE_LOOP ( 'NONE', ( #32210, #13014, #5152, #31773 ) ) ;
#17284 = ORIENTED_EDGE ( 'NONE', *, *, #26721, .F. ) ;
#17285 = EDGE_LOOP ( 'NONE', ( #50865, #15632, #6986, #50957 ) ) ;
#17286 = EDGE_CURVE ( 'NONE', #19435, #44506, #43917, .T. ) ;
#17287 = FACE_OUTER_BOUND ( 'NONE', #16308, .T. ) ;
#17288 = CARTESIAN_POINT ( 'NONE',  ( -158.1873290247468447, -177.1207230881787780, 57.79541595648306185 ) ) ;
#17289 = VERTEX_POINT ( 'NONE', #20011 ) ;
#17290 = CIRCLE ( 'NONE', #4674, 125.0000000000000000 ) ;
#17291 = LINE ( 'NONE', #44879, #18371 ) ;
#17292 = VECTOR ( 'NONE', #19824, 1000.000000000000000 ) ;
#17293 = CARTESIAN_POINT ( 'NONE',  ( 26.70958190211000982, -189.7472609257535510, -99.85818990449013199 ) ) ;
#17294 = DIRECTION ( 'NONE',  ( 0.000000000000000000, -0.000000000000000000, -1.000000000000000000 ) ) ;
#17295 = EDGE_LOOP ( 'NONE', ( #25711, #14706, #45118, #11644 ) ) ;
#17296 = EDGE_CURVE ( 'NONE', #20535, #23501, #36039, .T. ) ;
#17297 = EDGE_CURVE ( 'NONE', #39416, #37656, #46668, .T. ) ;
#17298 = ADVANCED_FACE ( 'NONE', ( #48918 ), #24732, .T. ) ;
#17299 = VECTOR ( 'NONE', #6955, 1000.000000000000114 ) ;
#17300 = EDGE_CURVE ( 'NONE', #5586, #12962, #4767, .T. ) ;
#17301 = VECTOR ( 'NONE', #26416, 999.9999999999998863 ) ;
#17302 = FACE_OUTER_BOUND ( 'NONE', #39612, .T. ) ;
#17303 = DIRECTION ( 'NONE',  ( -0.9151456172430237901, 0.000000000000000000, 0.4031234292879600778 ) ) ;
#17304 = ORIENTED_EDGE ( 'NONE', *, *, #20244, .F. ) ;
#17307 = ORIENTED_EDGE ( 'NONE', *, *, #6478, .T. ) ;
#17306 = CARTESIAN_POINT ( 'NONE',  ( -339.1964088526558498, -180.9052250602809977, -13.63415328425247885 ) ) ;
#17305 = CARTESIAN_POINT ( 'NONE',  ( -137.9639882952644143, -193.5000000000000000, 87.27805883780241913 ) ) ;
#17308 = ORIENTED_EDGE ( 'NONE', *, *, #27009, .T. ) ;
#17309 = EDGE_CURVE ( 'NONE', #20792, #34352, #25508, .T. ) ;
#17310 = ORIENTED_EDGE ( 'NONE', *, *, #7257, .T. ) ;
#17311 = CARTESIAN_POINT ( 'NONE',  ( -339.1964088526558498, -95.63860483659040312, 52.00954392751717847 ) ) ;
#17312 = VERTEX_POINT ( 'NONE', #9233 ) ;
#17313 = DIRECTION ( 'NONE',  ( 0.000000000000000000, -1.000000000000000000, 0.000000000000000000 ) ) ;
#17314 = PLANE ( 'NONE',  #37628 ) ;
#17315 = ORIENTED_EDGE ( 'NONE', *, *, #35601, .T. ) ;
#17316 = ADVANCED_FACE ( 'NONE', ( #44709 ), #40484, .F. ) ;
#17317 = CARTESIAN_POINT ( 'NONE',  ( -156.7610986364826999, -183.6283474603465606, -62.45009659481510766 ) ) ;
#17318 = EDGE_LOOP ( 'NONE', ( #18483, #4886, #39390, #1768 ) ) ;
#17319 = EDGE_CURVE ( 'NONE', #7465, #1427, #20520, .T. ) ;
#17320 = ORIENTED_EDGE ( 'NONE', *, *, #7257, .F. ) ;
#17321 = DIRECTION ( 'NONE',  ( 0.000000000000000000, 0.000000000000000000, 1.000000000000000000 ) ) ;
#17322 = AXIS2_PLACEMENT_3D ( 'NONE', #47259, #3607, #44347 ) ;
#17323 = LINE ( 'NONE', #28859, #10468 ) ;
#17324 = AXIS2_PLACEMENT_3D ( 'NONE', #16477, #12767, #28795 ) ;
#17325 = EDGE_CURVE ( 'NONE', #10943, #28183, #23990, .T. ) ;
#17326 = DIRECTION ( 'NONE',  ( 0.000000000000000000, 0.6631226582408039638, 0.7485107481710934207 ) ) ;
#17327 = CARTESIAN_POINT ( 'NONE',  ( -166.1003692892502102, -177.1207230881787780, -42.31126686685033889 ) ) ;
#17328 = EDGE_LOOP ( 'NONE', ( #21348, #18535, #46165, #15180 ) ) ;
#17329 = AXIS2_PLACEMENT_3D ( 'NONE', #18667, #42301, #50224 ) ;
#17330 = CARTESIAN_POINT ( 'NONE',  ( -47.82630463331832971, -175.3837268820161057, -0.7575112421616121416 ) ) ;
#17331 = VECTOR ( 'NONE', #44, 1000.000000000000227 ) ;
#17332 = ADVANCED_FACE ( 'NONE', ( #28917 ), #37605, .T. ) ;
#17333 = PRODUCT_CONTEXT ( 'NONE', #20613, 'mechanical' ) ;
#17334 = DIRECTION ( 'NONE',  ( 0.000000000000000000, 0.6631226582407911962, -0.7485107481711046340 ) ) ;
#17335 = LINE ( 'NONE', #27649, #27856 ) ;
#17336 = CARTESIAN_POINT ( 'NONE',  ( -142.3192003680973130, -183.6283474603465606, 82.57748230379306165 ) ) ;
#17337 = CARTESIAN_POINT ( 'NONE',  ( -49.42645310536304493, -183.6283474603465606, 0.3202698538628349079 ) ) ;
#17338 = EDGE_CURVE ( 'NONE', #35535, #46461, #21584, .T. ) ;
#17339 = EDGE_CURVE ( 'NONE', #44669, #13273, #48394, .T. ) ;
#17340 = DIRECTION ( 'NONE',  ( -0.000000000000000000, 1.000000000000000000, -0.000000000000000000 ) ) ;
#17341 = VERTEX_POINT ( 'NONE', #25002 ) ;
#17342 = CIRCLE ( 'NONE', #7266, 60.00000000000000000 ) ;
#17343 = AXIS2_PLACEMENT_3D ( 'NONE', #45448, #38057, #38318 ) ;
#17344 = VECTOR ( 'NONE', #33595, 1000.000000000000114 ) ;
#17345 = CARTESIAN_POINT ( 'NONE',  ( -11.17913199888832487, -175.3837268820161057, 119.3051146910914468 ) ) ;
#17346 = DIRECTION ( 'NONE',  ( 0.000000000000000000, -0.000000000000000000, 1.000000000000000000 ) ) ;
#17347 = ORIENTED_EDGE ( 'NONE', *, *, #7715, .T. ) ;
#17348 = CARTESIAN_POINT ( 'NONE',  ( -47.47956591500005885, -189.7472609257535510, -0.02963332782254939762 ) ) ;
#17349 = CIRCLE ( 'NONE', #1378, 125.0000000000000000 ) ;
#17350 = VERTEX_POINT ( 'NONE', #49176 ) ;
#17351 = EDGE_CURVE ( 'NONE', #42367, #6696, #9487, .T. ) ;
#17352 = AXIS2_PLACEMENT_3D ( 'NONE', #32614, #16601, #8695 ) ;
#17353 = LINE ( 'NONE', #30200, #21733 ) ;
#17354 = LINE ( 'NONE', #32581, #9448 ) ;
#17355 = DIRECTION ( 'NONE',  ( 0.000000000000000000, -0.6631226582407863113, 0.7485107481711089639 ) ) ;
#17356 = DIRECTION ( 'NONE',  ( -8.718379230999705894E-17, -0.5680647467311457088, 0.8229838658936634577 ) ) ;
#17357 = EDGE_LOOP ( 'NONE', ( #21075, #48007, #24141, #26059 ) ) ;
#17358 = CARTESIAN_POINT ( 'NONE',  ( 26.70958190211001337, -193.5000000000000000, -99.85818990449013199 ) ) ;
#17359 = DIRECTION ( 'NONE',  ( -0.9266896074318291543, 0.000000000000000000, -0.3758275821142488260 ) ) ;
#17360 = EDGE_LOOP ( 'NONE', ( #32323, #16151, #35881, #18473 ) ) ;
#17361 = CARTESIAN_POINT ( 'NONE',  ( 69.14211578623219623, -183.6283474603465606, 42.31126686685117022 ) ) ;
#17362 = VERTEX_POINT ( 'NONE', #44452 ) ;
#17363 = CARTESIAN_POINT ( 'NONE',  ( -339.1964088526558498, -89.57268800991514013, -48.27201571436026484 ) ) ;
#17364 = CIRCLE ( 'NONE', #566, 60.00000000000000000 ) ;
#17365 = VECTOR ( 'NONE', #2193, 1000.000000000000000 ) ;
#17366 = VERTEX_POINT ( 'NONE', #818 ) ;
#17367 = PLANE ( 'NONE',  #10004 ) ;
#17368 = VECTOR ( 'NONE', #7277, 1000.000000000000000 ) ;
#17369 = EDGE_CURVE ( 'NONE', #33577, #7787, #32618, .T. ) ;
#17370 = EDGE_LOOP ( 'NONE', ( #4569, #36396, #3898, #29179 ) ) ;
#17371 = EDGE_CURVE ( 'NONE', #6229, #38472, #21050, .T. ) ;
#17372 = ADVANCED_FACE ( 'NONE', ( #29191 ), #37069, .T. ) ;
#17373 = EDGE_CURVE ( 'NONE', #8813, #40221, #5554, .T. ) ;
#17374 = DIRECTION ( 'NONE',  ( 1.000000000000000000, 0.000000000000000000, 0.000000000000000000 ) ) ;
#17375 = EDGE_LOOP ( 'NONE', ( #43409, #22465, #1645, #36516 ) ) ;
#17378 = VERTEX_POINT ( 'NONE', #5296 ) ;
#17377 = DIRECTION ( 'NONE',  ( 0.000000000000000000, 0.000000000000000000, 1.000000000000000000 ) ) ;
#17376 = FACE_OUTER_BOUND ( 'NONE', #23919, .T. ) ;
#17379 = CIRCLE ( 'NONE', #19051, 125.0000000000000000 ) ;
#17380 = AXIS2_PLACEMENT_3D ( 'NONE', #49232, #9287, #33957 ) ;
#17381 = PLANE ( 'NONE',  #12165 ) ;
#17383 = ORIENTED_EDGE ( 'NONE', *, *, #29858, .F. ) ;
#17382 = VECTOR ( 'NONE', #21653, 1000.000000000000000 ) ;
#17384 = DIRECTION ( 'NONE',  ( 0.000000000000000000, 0.000000000000000000, -1.000000000000000000 ) ) ;
#17385 = ORIENTED_EDGE ( 'NONE', *, *, #40564, .F. ) ;
#17386 = CARTESIAN_POINT ( 'NONE',  ( -339.1964088526558498, -180.9052250602807703, 13.63415328425337236 ) ) ;
#17389 = ORIENTED_EDGE ( 'NONE', *, *, #35627, .F. ) ;
#17388 = DIRECTION ( 'NONE',  ( 0.000000000000000000, 0.000000000000000000, 1.000000000000000000 ) ) ;
#17387 = DIRECTION ( 'NONE',  ( 0.000000000000000000, 0.000000000000000000, -1.000000000000000000 ) ) ;
#17390 = EDGE_LOOP ( 'NONE', ( #40555, #1984, #47194, #2697 ) ) ;
#17391 = AXIS2_PLACEMENT_3D ( 'NONE', #221, #31503, #36475 ) ;
#17392 = CARTESIAN_POINT ( 'NONE',  ( -169.9131040279660283, -193.5000000000000000, 29.64437826672835996 ) ) ;
#17393 = DIRECTION ( 'NONE',  ( -0.000000000000000000, 1.000000000000000000, -0.000000000000000000 ) ) ;
#17394 = CARTESIAN_POINT ( 'NONE',  ( -339.1964088526558498, -64.50000000000000000, -0.5000000000000457412 ) ) ;
#17395 = EDGE_CURVE ( 'NONE', #18306, #43135, #16325, .T. ) ;
#17396 = VERTEX_POINT ( 'NONE', #37851 ) ;
#17397 = DIRECTION ( 'NONE',  ( 0.4677363560876406923, 0.000000000000000000, 0.8838680338115276758 ) ) ;
#17398 = FACE_OUTER_BOUND ( 'NONE', #18281, .T. ) ;
#17399 = LINE ( 'NONE', #7988, #24300 ) ;
#17400 = LINE ( 'NONE', #41533, #21559 ) ;
#17401 = ORIENTED_EDGE ( 'NONE', *, *, #19487, .T. ) ;
#17402 = CARTESIAN_POINT ( 'NONE',  ( -339.1964088526558498, -131.1080185721133660, -58.50955523165751515 ) ) ;
#17403 = CARTESIAN_POINT ( 'NONE',  ( -330.4913330509368166, -63.87926739338334414, -6.735595255826711814 ) ) ;
#17404 = EDGE_CURVE ( 'NONE', #49012, #37757, #14214, .T. ) ;
#17405 = CARTESIAN_POINT ( 'NONE',  ( 70.98542830588607444, -193.5000000000000000, -36.78613984829961936 ) ) ;
#17406 = VERTEX_POINT ( 'NONE', #2624 ) ;
#17407 = VECTOR ( 'NONE', #48783, 1000.000000000000114 ) ;
#17408 = AXIS2_PLACEMENT_3D ( 'NONE', #27595, #40194, #36246 ) ;
#17409 = DIRECTION ( 'NONE',  ( -0.000000000000000000, 1.000000000000000000, -0.000000000000000000 ) ) ;
#17410 = CARTESIAN_POINT ( 'NONE',  ( -164.8312043469690593, -183.6283474603465606, -42.87565520599201818 ) ) ;
#17411 = VECTOR ( 'NONE', #45779, 1000.000000000000114 ) ;
#17412 = CARTESIAN_POINT ( 'NONE',  ( -36.09284319799462537, -183.6283474603465606, 124.3848060646152618 ) ) ;
#17413 = DIRECTION ( 'NONE',  ( -0.9027978299657416494, 0.000000000000000000, -0.4300652022765245608 ) ) ;
#17414 = CARTESIAN_POINT ( 'NONE',  ( -139.4082623311986993, -193.5000000000000000, 84.30834960113001841 ) ) ;
#17415 = VECTOR ( 'NONE', #22241, 1000.000000000000000 ) ;
#17416 = AXIS2_PLACEMENT_3D ( 'NONE', #16849, #19995, #23928 ) ;
#17417 = LINE ( 'NONE', #36578, #46332 ) ;
#17418 = CARTESIAN_POINT ( 'NONE',  ( -84.82349129030166068, -175.3837268820161057, -119.5996955107802222 ) ) ;
#17420 = VERTEX_POINT ( 'NONE', #41805 ) ;
#17419 = DIRECTION ( 'NONE',  ( 0.000000000000000000, 1.000000000000000000, -0.000000000000000000 ) ) ;
#17421 = VECTOR ( 'NONE', #17762, 1000.000000000000341 ) ;
#17422 = EDGE_LOOP ( 'NONE', ( #14569, #2791, #41635, #36618 ) ) ;
#17423 = DIRECTION ( 'NONE',  ( 0.4031234292879792847, 0.000000000000000000, -0.9151456172430153524 ) ) ;
#17424 = VECTOR ( 'NONE', #36077, 1000.000000000000114 ) ;
#17425 = VECTOR ( 'NONE', #22656, 1000.000000000000000 ) ;
#17426 = CARTESIAN_POINT ( 'NONE',  ( 0.000000000000000000, -79.33786585790457480, 39.12423683620640702 ) ) ;
#17428 = VERTEX_POINT ( 'NONE', #18411 ) ;
#17427 = DIRECTION ( 'NONE',  ( 0.000000000000000000, 1.000000000000000000, 0.000000000000000000 ) ) ;
#17429 = VERTEX_POINT ( 'NONE', #14468 ) ;
#17430 = ORIENTED_EDGE ( 'NONE', *, *, #50380, .F. ) ;
#17431 = CARTESIAN_POINT ( 'NONE',  ( -332.3517673607765914, -132.2320517616439020, -58.37307289257706344 ) ) ;
#17432 = ADVANCED_FACE ( 'NONE', ( #34677 ), #46787, .F. ) ;
#17433 = CARTESIAN_POINT ( 'NONE',  ( 59.00260725618641544, -183.6283474603465606, -63.81752780152991278 ) ) ;
#17434 = DIRECTION ( 'NONE',  ( 0.000000000000000000, 0.000000000000000000, 1.000000000000000000 ) ) ;
#17435 = ORIENTED_EDGE ( 'NONE', *, *, #20180, .F. ) ;
#17436 = LINE ( 'NONE', #33457, #21839 ) ;
#17437 = AXIS2_PLACEMENT_3D ( 'NONE', #25380, #1468, #25893 ) ;
#17439 = VERTEX_POINT ( 'NONE', #5826 ) ;
#17438 = DIRECTION ( 'NONE',  ( -1.000000000000000000, 0.000000000000000000, 0.000000000000000000 ) ) ;
#17440 = CIRCLE ( 'NONE', #33368, 125.0000000000000000 ) ;
#17441 = CARTESIAN_POINT ( 'NONE',  ( 27.50603775690335695, -175.3837268820161057, -99.25348746834811209 ) ) ;
#17442 = VERTEX_POINT ( 'NONE', #29972 ) ;
#17443 = PLANE ( 'NONE',  #1168 ) ;
#17444 = CIRCLE ( 'NONE', #5700, 125.0000000000000000 ) ;
#17445 = VERTEX_POINT ( 'NONE', #38369 ) ;
#17446 = DIRECTION ( 'NONE',  ( 0.000000000000000000, 1.000000000000000000, 0.000000000000000000 ) ) ;
#17447 = LINE ( 'NONE', #41324, #48997 ) ;
#17448 = CARTESIAN_POINT ( 'NONE',  ( -123.8574911141017623, -189.7472609257535510, 98.45863302693528851 ) ) ;
#17449 = EDGE_LOOP ( 'NONE', ( #37952, #16853, #25170, #39428 ) ) ;
#17450 = VECTOR ( 'NONE', #3313, 1000.000000000000000 ) ;
#17451 = ORIENTED_EDGE ( 'NONE', *, *, #41744, .F. ) ;
#17452 = CARTESIAN_POINT ( 'NONE',  ( -37.67038537088846084, -177.1207230881787780, -124.5318076226586612 ) ) ;
#17453 = DIRECTION ( 'NONE',  ( 1.000000000000000000, -0.000000000000000000, -0.000000000000000000 ) ) ;
#17454 = VECTOR ( 'NONE', #29178, 1000.000000000000000 ) ;
#17455 = VERTEX_POINT ( 'NONE', #18664 ) ;
#17456 = ADVANCED_FACE ( 'NONE', ( #50727 ), #45747, .F. ) ;
#17457 = DIRECTION ( 'NONE',  ( 0.000000000000000000, 0.000000000000000000, 1.000000000000000000 ) ) ;
#17458 = AXIS2_PLACEMENT_3D ( 'NONE', #48385, #12370, #28397 ) ;
#17459 = ORIENTED_EDGE ( 'NONE', *, *, #9874, .T. ) ;
#17460 = FACE_BOUND ( 'NONE', #50306, .T. ) ;
#17461 = PLANE ( 'NONE',  #11320 ) ;
#17462 = EDGE_CURVE ( 'NONE', #41184, #16398, #18147, .T. ) ;
#17463 = AXIS2_PLACEMENT_3D ( 'NONE', #2866, #13930, #38085 ) ;
#17464 = ORIENTED_EDGE ( 'NONE', *, *, #7048, .F. ) ;
#17465 = LINE ( 'NONE', #8252, #532 ) ;
#17466 = ORIENTED_EDGE ( 'NONE', *, *, #40559, .T. ) ;
#17467 = LINE ( 'NONE', #49523, #45558 ) ;
#17468 = CARTESIAN_POINT ( 'NONE',  ( -305.0000000000000568, -123.5000000000000284, 0.000000000000000000 ) ) ;
#17469 = ORIENTED_EDGE ( 'NONE', *, *, #19831, .F. ) ;
#17470 = CARTESIAN_POINT ( 'NONE',  ( -15.48416040178638831, -177.1207230881787780, 119.5301634136914970 ) ) ;
#17471 = LINE ( 'NONE', #9827, #6255 ) ;
#17472 = DIRECTION ( 'NONE',  ( -0.000000000000000000, 1.000000000000000000, -0.000000000000000000 ) ) ;
#17473 = EDGE_CURVE ( 'NONE', #16711, #33847, #33904, .T. ) ;
#17474 = DIRECTION ( 'NONE',  ( 0.4566292373937077542, 0.000000000000000000, 0.8896570909947499883 ) ) ;
#17475 = ORIENTED_EDGE ( 'NONE', *, *, #39886, .F. ) ;
#17476 = CARTESIAN_POINT ( 'NONE',  ( -330.4913330509368166, -180.6659093959932250, 14.60509510167933556 ) ) ;
#17477 = ORIENTED_EDGE ( 'NONE', *, *, #10714, .F. ) ;
#17478 = ORIENTED_EDGE ( 'NONE', *, *, #17550, .T. ) ;
#17479 = VECTOR ( 'NONE', #9098, 1000.000000000000000 ) ;
#17480 = VECTOR ( 'NONE', #11474, 1000.000000000000000 ) ;
#17481 = LINE ( 'NONE', #29283, #24332 ) ;
#17483 = ORIENTED_EDGE ( 'NONE', *, *, #35617, .T. ) ;
#17482 = FACE_OUTER_BOUND ( 'NONE', #21959, .T. ) ;
#17484 = AXIS2_PLACEMENT_3D ( 'NONE', #20560, #44487, #20049 ) ;
#17485 = VERTEX_POINT ( 'NONE', #50219 ) ;
#17486 = CARTESIAN_POINT ( 'NONE',  ( 0.000000000000000000, -53.50000000000000000, 0.000000000000000000 ) ) ;
#17487 = ADVANCED_FACE ( 'NONE', ( #42051 ), #26274, .T. ) ;
#17488 = CARTESIAN_POINT ( 'NONE',  ( -336.3521761649654422, -182.5000000000000568, 1.632288850093980725 ) ) ;
#17489 = VECTOR ( 'NONE', #35172, 1000.000000000000000 ) ;
#17490 = ORIENTED_EDGE ( 'NONE', *, *, #17614, .F. ) ;
#17491 = CARTESIAN_POINT ( 'NONE',  ( -2.429962845726266397E-15, 20.00000000000000355, 0.000000000000000000 ) ) ;
#17492 = EDGE_LOOP ( 'NONE', ( #1464, #36600, #18939, #47511 ) ) ;
#17493 = DIRECTION ( 'NONE',  ( -0.000000000000000000, 0.000000000000000000, -1.000000000000000000 ) ) ;
#17494 = FACE_OUTER_BOUND ( 'NONE', #23555, .T. ) ;
#17495 = EDGE_CURVE ( 'NONE', #32338, #26523, #4726, .T. ) ;
#17496 = DIRECTION ( 'NONE',  ( 0.000000000000000000, -1.000000000000000000, -0.000000000000000000 ) ) ;
#17497 = CARTESIAN_POINT ( 'NONE',  ( -15.81236726369125023, -177.1207230881787780, -120.6560517527615417 ) ) ;
#17498 = VERTEX_POINT ( 'NONE', #6317 ) ;
#17499 = VERTEX_POINT ( 'NONE', #22859 ) ;
#17500 = ORIENTED_EDGE ( 'NONE', *, *, #2230, .T. ) ;
#17501 = CIRCLE ( 'NONE', #46866, 60.00000000000000000 ) ;
#17502 = CARTESIAN_POINT ( 'NONE',  ( 27.23560471289044571, -175.3837268820161057, 99.45993886622845537 ) ) ;
#17503 = CARTESIAN_POINT ( 'NONE',  ( -336.3521761649654422, -64.66963335249506883, 11.78931550685348029 ) ) ;
#17504 = EDGE_CURVE ( 'NONE', #15290, #14977, #14720, .T. ) ;
#17505 = DIRECTION ( 'NONE',  ( 0.000000000000000000, 0.000000000000000000, -1.000000000000000000 ) ) ;
#17506 = LINE ( 'NONE', #16728, #17183 ) ;
#17507 = ORIENTED_EDGE ( 'NONE', *, *, #45472, .F. ) ;
#17508 = EDGE_LOOP ( 'NONE', ( #9320, #39508, #5858, #17015 ) ) ;
#17510 = ORIENTED_EDGE ( 'NONE', *, *, #43523, .F. ) ;
#17509 = CARTESIAN_POINT ( 'NONE',  ( -170.0000000000000284, -173.5000000000000284, 60.00000000000000000 ) ) ;
#17511 = VECTOR ( 'NONE', #49513, 1000.000000000000000 ) ;
#17512 = ORIENTED_EDGE ( 'NONE', *, *, #15568, .F. ) ;
#17513 = VECTOR ( 'NONE', #14084, 1000.000000000000114 ) ;
#17515 = AXIS2_PLACEMENT_3D ( 'NONE', #28903, #33886, #9724 ) ;
#17514 = DIRECTION ( 'NONE',  ( 0.1182731709213523247, 0.000000000000000000, 0.9929810960135185827 ) ) ;
#17516 = EDGE_CURVE ( 'NONE', #42461, #37884, #25774, .T. ) ;
#17517 = LINE ( 'NONE', #20930, #43438 ) ;
#17518 = CIRCLE ( 'NONE', #46888, 125.0000000000000000 ) ;
#17519 = FACE_OUTER_BOUND ( 'NONE', #38770, .T. ) ;
#17520 = CARTESIAN_POINT ( 'NONE',  ( -101.0675409952199999, -177.1207230881787780, 113.3995532942341100 ) ) ;
#17521 = ORIENTED_EDGE ( 'NONE', *, *, #37833, .T. ) ;
#17522 = LINE ( 'NONE', #37729, #30886 ) ;
#17523 = EDGE_LOOP ( 'NONE', ( #24830, #27239, #2942, #2373 ) ) ;
#17524 = CARTESIAN_POINT ( 'NONE',  ( 76.48781641346532467, -189.7472609257535510, 2.874563619424060246 ) ) ;
#17525 = AXIS2_PLACEMENT_3D ( 'NONE', #24635, #24383, #40387 ) ;
#17526 =( NAMED_UNIT ( * ) SI_UNIT ( $, .STERADIAN. ) SOLID_ANGLE_UNIT ( ) );
#17527 = CARTESIAN_POINT ( 'NONE',  ( -49.47517659412407198, -193.5000000000000000, 0.08879589532293177823 ) ) ;
#17528 = ORIENTED_EDGE ( 'NONE', *, *, #18191, .F. ) ;
#17529 = CARTESIAN_POINT ( 'NONE',  ( -33.52607327456454556, -193.5000000000000000, -124.1024020384603119 ) ) ;
#17530 = DIRECTION ( 'NONE',  ( 0.000000000000000000, 1.000000000000000000, 0.000000000000000000 ) ) ;
#17531 = CARTESIAN_POINT ( 'NONE',  ( -332.3517673607765914, -72.67320051506121104, 31.88473700876054551 ) ) ;
#17532 = CARTESIAN_POINT ( 'NONE',  ( -48.47912675150885065, -175.3837268820161057, 6.938893903907228378E-15 ) ) ;
#17533 = VECTOR ( 'NONE', #10250, 1000.000000000000000 ) ;
#17534 = DIRECTION ( 'NONE',  ( 0.000000000000000000, -0.9709418174260493473, 0.2393156642875685913 ) ) ;
#17535 = FACE_BOUND ( 'NONE', #32838, .T. ) ;
#17536 = ORIENTED_EDGE ( 'NONE', *, *, #18432, .F. ) ;
#17537 = DIRECTION ( 'NONE',  ( 0.000000000000000000, 0.000000000000000000, 1.000000000000000000 ) ) ;
#17538 = ORIENTED_EDGE ( 'NONE', *, *, #43998, .T. ) ;
#17539 = EDGE_CURVE ( 'NONE', #34512, #37437, #10501, .T. ) ;
#17540 = ORIENTED_EDGE ( 'NONE', *, *, #42016, .T. ) ;
#17541 = EDGE_CURVE ( 'NONE', #38180, #13416, #14830, .T. ) ;
#17542 = CARTESIAN_POINT ( 'NONE',  ( -82.67254833784559764, -183.6283474603465606, -120.2323164553483963 ) ) ;
#17543 = VERTEX_POINT ( 'NONE', #26534 ) ;
#17544 = FACE_OUTER_BOUND ( 'NONE', #49870, .T. ) ;
#17545 = AXIS2_PLACEMENT_3D ( 'NONE', #24473, #40492, #35516 ) ;
#17546 = CARTESIAN_POINT ( 'NONE',  ( 75.48825557695654709, -189.7472609257535510, 2.844930291601486694 ) ) ;
#17548 = ORIENTED_EDGE ( 'NONE', *, *, #25840, .F. ) ;
#17547 = FACE_OUTER_BOUND ( 'NONE', #28896, .T. ) ;
#17549 = AXIS2_PLACEMENT_3D ( 'NONE', #27284, #15476, #48043 ) ;
#17550 = EDGE_CURVE ( 'NONE', #32204, #22697, #42572, .T. ) ;
#17551 = CARTESIAN_POINT ( 'NONE',  ( 4.109287492203100634, -193.5000000000000000, -113.3995532942336979 ) ) ;
#17552 = EDGE_LOOP ( 'NONE', ( #36814, #49850, #13308, #11156 ) ) ;
#17553 = ORIENTED_EDGE ( 'NONE', *, *, #36834, .T. ) ;
#17554 = ADVANCED_FACE ( 'NONE', ( #6586 ), #38623, .T. ) ;
#17555 = EDGE_LOOP ( 'NONE', ( #16931, #33943 ) ) ;
#17556 = LINE ( 'NONE', #33569, #35958 ) ;
#17557 = CARTESIAN_POINT ( 'NONE',  ( -47.57632892154310866, -177.1207230881787780, -0.4300652022765113491 ) ) ;
#17558 = EDGE_CURVE ( 'NONE', #18768, #1472, #1609, .T. ) ;
#17559 = ORIENTED_EDGE ( 'NONE', *, *, #22815, .T. ) ;
#17560 = CARTESIAN_POINT ( 'NONE',  ( -47.97059563285962724, -175.3837268820161057, -0.8610436117673480050 ) ) ;
#17561 = LINE ( 'NONE', #22535, #48864 ) ;
#17562 = DIRECTION ( 'NONE',  ( 0.6528221181905227155, 0.000000000000000000, -0.7575112421616191360 ) ) ;
#17563 = EDGE_LOOP ( 'NONE', ( #40645, #48314, #26568, #36586 ) ) ;
#17564 = AXIS2_PLACEMENT_3D ( 'NONE', #17764, #5940, #30349 ) ;
#17565 = DIRECTION ( 'NONE',  ( -0.000000000000000000, 1.000000000000000000, -0.000000000000000000 ) ) ;
#17566 = FACE_OUTER_BOUND ( 'NONE', #51633, .T. ) ;
#17567 = ORIENTED_EDGE ( 'NONE', *, *, #28137, .T. ) ;
#17569 = ORIENTED_EDGE ( 'NONE', *, *, #40859, .F. ) ;
#17568 = DIRECTION ( 'NONE',  ( 0.000000000000000000, 0.000000000000000000, 1.000000000000000000 ) ) ;
#17570 = ORIENTED_EDGE ( 'NONE', *, *, #42635, .T. ) ;
#17571 = ORIENTED_EDGE ( 'NONE', *, *, #17952, .F. ) ;
#17572 = CARTESIAN_POINT ( 'NONE',  ( 26.10278175629141373, -193.5000000000000000, -99.06333546307678262 ) ) ;
#17573 = PLANE ( 'NONE',  #2932 ) ;
#17574 = ORIENTED_EDGE ( 'NONE', *, *, #5082, .T. ) ;
#17575 = DIRECTION ( 'NONE',  ( 0.000000000000000000, 0.000000000000000000, 1.000000000000000000 ) ) ;
#17576 = LINE ( 'NONE', #50407, #22587 ) ;
#17577 = VERTEX_POINT ( 'NONE', #26026 ) ;
#17578 = DIRECTION ( 'NONE',  ( 0.000000000000000000, 1.000000000000000000, -0.000000000000000000 ) ) ;
#17579 = ORIENTED_EDGE ( 'NONE', *, *, #4421, .F. ) ;
#17580 = ORIENTED_EDGE ( 'NONE', *, *, #6170, .T. ) ;
#17581 = CYLINDRICAL_SURFACE ( 'NONE', #33777, 124.9999999999999858 ) ;
#17582 = DIRECTION ( 'NONE',  ( -1.000000000000000000, -0.000000000000000000, 0.000000000000000000 ) ) ;
#17583 = AXIS2_PLACEMENT_3D ( 'NONE', #14680, #23590, #47523 ) ;
#17584 = LINE ( 'NONE', #764, #48191 ) ;
#17585 = DIRECTION ( 'NONE',  ( -0.1182731709213660498, 0.000000000000000000, 0.9929810960135169173 ) ) ;
#17586 = ORIENTED_EDGE ( 'NONE', *, *, #18530, .F. ) ;
#17587 = CARTESIAN_POINT ( 'NONE',  ( -332.3517673607765914, -85.59754891220836726, -45.24454186338619621 ) ) ;
#17588 = AXIS2_PLACEMENT_3D ( 'NONE', #50639, #29879, #50137 ) ;
#17589 = DIRECTION ( 'NONE',  ( 0.000000000000000000, -1.000000000000000000, -0.000000000000000000 ) ) ;
#17590 = CARTESIAN_POINT ( 'NONE',  ( 67.42090074966655777, -189.7472609257535510, -46.82076062204440348 ) ) ;
#17591 = DIRECTION ( 'NONE',  ( -0.7765238627180482966, 0.000000000000000000, 0.6300878435817038881 ) ) ;
#17592 = ORIENTED_EDGE ( 'NONE', *, *, #17622, .F. ) ;
#17593 = CARTESIAN_POINT ( 'NONE',  ( 14.94072793302542124, -189.7472609257535510, 107.7168604805791574 ) ) ;
#17594 = CARTESIAN_POINT ( 'NONE',  ( -133.8011377042516301, -193.5000000000000000, -91.35181687837437892 ) ) ;
#17595 = DIRECTION ( 'NONE',  ( 0.9890401873221633666, 0.000000000000000000, 0.1476465640024850756 ) ) ;
#17596 = VERTEX_POINT ( 'NONE', #35195 ) ;
#17597 = ADVANCED_FACE ( 'NONE', ( #11016 ), #7601, .F. ) ;
#17598 = PLANE ( 'NONE',  #10979 ) ;
#17599 = CARTESIAN_POINT ( 'NONE',  ( -115.7878797639662025, -193.5000000000000000, -104.1428419024399545 ) ) ;
#17600 = EDGE_CURVE ( 'NONE', #46515, #30632, #20659, .T. ) ;
#17601 = ORIENTED_EDGE ( 'NONE', *, *, #35550, .T. ) ;
#17602 = EDGE_CURVE ( 'NONE', #34082, #41945, #2881, .T. ) ;
#17603 = ORIENTED_EDGE ( 'NONE', *, *, #43159, .T. ) ;
#17604 = ORIENTED_EDGE ( 'NONE', *, *, #38767, .T. ) ;
#17605 = EDGE_CURVE ( 'NONE', #12957, #1349, #44180, .T. ) ;
#17606 = VECTOR ( 'NONE', #19056, 1000.000000000000000 ) ;
#17607 = DIRECTION ( 'NONE',  ( -0.9266896074318370369, 0.000000000000000000, 0.3758275821142292306 ) ) ;
#17608 = ADVANCED_FACE ( 'NONE', ( #47821 ), #23881, .T. ) ;
#17609 = DIRECTION ( 'NONE',  ( 1.000000000000000000, 0.000000000000000000, -0.000000000000000000 ) ) ;
#17610 = CARTESIAN_POINT ( 'NONE',  ( -332.3517673607765914, -171.1288023355047585, 34.85916744524404720 ) ) ;
#17611 = LINE ( 'NONE', #21801, #51444 ) ;
#17612 = EDGE_CURVE ( 'NONE', #48961, #5269, #9755, .T. ) ;
#17613 = CARTESIAN_POINT ( 'NONE',  ( -339.1964088526558498, -95.17484985463089231, 52.89315522108975642 ) ) ;
#17614 = EDGE_CURVE ( 'NONE', #30219, #38873, #51762, .T. ) ;
#17615 = CARTESIAN_POINT ( 'NONE',  ( -143.2689064740322351, -193.5000000000000000, -79.94433946042764205 ) ) ;
#17616 = ORIENTED_EDGE ( 'NONE', *, *, #6983, .T. ) ;
#17617 = EDGE_CURVE ( 'NONE', #16239, #46127, #47303, .T. ) ;
#17618 = DIRECTION ( 'NONE',  ( 0.000000000000000000, 0.000000000000000000, 1.000000000000000000 ) ) ;
#17619 = EDGE_LOOP ( 'NONE', ( #34868, #34787, #45073, #3902 ) ) ;
#17620 = EDGE_CURVE ( 'NONE', #47120, #23170, #23121, .T. ) ;
#17621 = DIRECTION ( 'NONE',  ( 0.000000000000000000, -1.000000000000000000, 0.000000000000000000 ) ) ;
#17622 = EDGE_CURVE ( 'NONE', #12850, #35564, #51498, .T. ) ;
#17623 = CIRCLE ( 'NONE', #44429, 125.0000000000000000 ) ;
#17624 = ORIENTED_EDGE ( 'NONE', *, *, #18392, .F. ) ;
#17625 = PLANE ( 'NONE',  #24212 ) ;
#17626 = EDGE_CURVE ( 'NONE', #49035, #45874, #27573, .T. ) ;
#17627 = ORIENTED_EDGE ( 'NONE', *, *, #394, .F. ) ;
#17628 = CARTESIAN_POINT ( 'NONE',  ( -332.3517673607765914, -83.15397741537739762, 43.07972642080338233 ) ) ;
#17629 = DIRECTION ( 'NONE',  ( 0.000000000000000000, -1.000000000000000000, 0.000000000000000000 ) ) ;
#17630 = VERTEX_POINT ( 'NONE', #15776 ) ;
#17633 = ORIENTED_EDGE ( 'NONE', *, *, #27334, .F. ) ;
#17632 = CARTESIAN_POINT ( 'NONE',  ( 31.28129687248616619, -177.1207230881787780, 96.24590808611479531 ) ) ;
#17631 = DIRECTION ( 'NONE',  ( 0.000000000000000000, 0.000000000000000000, -1.000000000000000000 ) ) ;
#17634 = LINE ( 'NONE', #13672, #33186 ) ;
#17635 = ORIENTED_EDGE ( 'NONE', *, *, #46418, .F. ) ;
#17636 = CARTESIAN_POINT ( 'NONE',  ( -81.47409310123212833, -177.1207230881787780, -119.5301634136912412 ) ) ;
#17637 = ORIENTED_EDGE ( 'NONE', *, *, #30337, .T. ) ;
#17638 = DIRECTION ( 'NONE',  ( 0.000000000000000000, 0.000000000000000000, -1.000000000000000000 ) ) ;
#17641 = ORIENTED_EDGE ( 'NONE', *, *, #16828, .T. ) ;
#17640 = FACE_OUTER_BOUND ( 'NONE', #49910, .T. ) ;
#17639 = CARTESIAN_POINT ( 'NONE',  ( -47.87232660569025455, -189.7472609257535510, -0.7948544414133454916 ) ) ;
#17642 = EDGE_CURVE ( 'NONE', #41498, #48626, #3145, .T. ) ;
#17643 = ORIENTED_EDGE ( 'NONE', *, *, #966, .F. ) ;
#17644 = AXIS2_PLACEMENT_3D ( 'NONE', #17557, #28827, #17800 ) ;
#17645 = AXIS2_PLACEMENT_3D ( 'NONE', #20100, #16430, #4085 ) ;
#17646 = DIRECTION ( 'NONE',  ( 0.000000000000000000, 0.000000000000000000, 1.000000000000000000 ) ) ;
#17647 = CARTESIAN_POINT ( 'NONE',  ( 71.15591247552653442, -177.1207230881787780, 36.22785377504035154 ) ) ;
#17648 = DIRECTION ( 'NONE',  ( 0.8757349421956345248, 0.000000000000000000, 0.4827922027307490205 ) ) ;
#17649 = VERTEX_POINT ( 'NONE', #43854 ) ;
#17650 = DIRECTION ( 'NONE',  ( -0.08879589532293158394, 0.000000000000000000, -0.9960498426152172291 ) ) ;
#17651 = CARTESIAN_POINT ( 'NONE',  ( -49.25565061422688728, -193.5000000000000000, -0.6300878435817132139 ) ) ;
#17652 = LINE ( 'NONE', #41023, #46118 ) ;
#17653 = CARTESIAN_POINT ( 'NONE',  ( -336.3521761649654422, -123.5000000000000284, 0.000000000000000000 ) ) ;
#17654 = VERTEX_POINT ( 'NONE', #27307 ) ;
#17655 = CARTESIAN_POINT ( 'NONE',  ( 27.23560471289043861, -189.7472609257535510, 99.45993886622846958 ) ) ;
#17656 = CARTESIAN_POINT ( 'NONE',  ( -169.9883746053192795, -193.5000000000000000, -24.72869175143020115 ) ) ;
#17657 = EDGE_CURVE ( 'NONE', #1828, #27213, #23382, .T. ) ;
#17658 = DIRECTION ( 'NONE',  ( -0.6749830015182196608, 0.000000000000000000, 0.7378332790417189146 ) ) ;
#17659 = ORIENTED_EDGE ( 'NONE', *, *, #46479, .T. ) ;
#17660 = AXIS2_PLACEMENT_3D ( 'NONE', #16301, #21284, #8414 ) ;
#17661 = DIRECTION ( 'NONE',  ( -0.000000000000000000, 1.000000000000000000, -0.000000000000000000 ) ) ;
#17662 = DIRECTION ( 'NONE',  ( 0.000000000000000000, 1.000000000000000000, -3.491481338843133355E-15 ) ) ;
#17663 = EDGE_CURVE ( 'NONE', #47785, #27930, #34942, .T. ) ;
#17664 = CARTESIAN_POINT ( 'NONE',  ( 76.46082103836691601, -189.7472609257535510, 3.874202661595774533 ) ) ;
#17665 = LINE ( 'NONE', #29994, #23280 ) ;
#17666 = EDGE_CURVE ( 'NONE', #563, #40551, #31506, .T. ) ;
#17667 = EDGE_CURVE ( 'NONE', #22277, #4055, #46960, .T. ) ;
#17668 = ADVANCED_FACE ( 'NONE', ( #26710 ), #42995, .T. ) ;
#17669 = DIRECTION ( 'NONE',  ( -1.000000000000000000, -9.758900497077134646E-15, 3.701062773504915833E-15 ) ) ;
#17670 = FACE_OUTER_BOUND ( 'NONE', #30615, .T. ) ;
#17671 = CARTESIAN_POINT ( 'NONE',  ( 0.000000000000000000, -71.25809448646064936, -27.41866715058241866 ) ) ;
#17673 = ORIENTED_EDGE ( 'NONE', *, *, #50433, .F. ) ;
#17672 = DIRECTION ( 'NONE',  ( -0.000000000000000000, -0.000000000000000000, 1.000000000000000000 ) ) ;
#17674 = VERTEX_POINT ( 'NONE', #18051 ) ;
#17675 = PLANE ( 'NONE',  #19042 ) ;
#17676 = EDGE_CURVE ( 'NONE', #38746, #47822, #34340, .T. ) ;
#17677 = VECTOR ( 'NONE', #27157, 1000.000000000000000 ) ;
#17678 = VECTOR ( 'NONE', #10595, 1000.000000000000000 ) ;
#17679 = LINE ( 'NONE', #21873, #13715 ) ;
#17681 = ORIENTED_EDGE ( 'NONE', *, *, #9317, .F. ) ;
#17680 = FACE_OUTER_BOUND ( 'NONE', #20116, .T. ) ;
#17682 = ORIENTED_EDGE ( 'NONE', *, *, #38374, .F. ) ;
#17683 = EDGE_CURVE ( 'NONE', #34468, #43598, #14122, .T. ) ;
#17684 = ORIENTED_EDGE ( 'NONE', *, *, #38759, .T. ) ;
#17685 = DIRECTION ( 'NONE',  ( 0.000000000000000000, -1.000000000000000000, 0.000000000000000000 ) ) ;
#17686 = EDGE_CURVE ( 'NONE', #20713, #50002, #50632, .T. ) ;
#17687 = DIRECTION ( 'NONE',  ( 0.000000000000000000, 0.000000000000000000, 1.000000000000000000 ) ) ;
#17688 = DIRECTION ( 'NONE',  ( 0.000000000000000000, 0.000000000000000000, 1.000000000000000000 ) ) ;
#17689 = EDGE_LOOP ( 'NONE', ( #19228, #24454, #31874, #24478 ) ) ;
#17690 = EDGE_CURVE ( 'NONE', #17967, #9413, #2787, .T. ) ;
#17691 = CARTESIAN_POINT ( 'NONE',  ( -332.3517673607765914, -123.5000000000000284, 0.000000000000000000 ) ) ;
#17693 = VERTEX_POINT ( 'NONE', #39038 ) ;
#17692 = FACE_OUTER_BOUND ( 'NONE', #14991, .T. ) ;
#17694 = AXIS2_PLACEMENT_3D ( 'NONE', #38540, #50631, #23299 ) ;
#17695 = DIRECTION ( 'NONE',  ( -0.2920567706369764371, 0.000000000000000000, 0.9564009842765223146 ) ) ;
#17696 = ORIENTED_EDGE ( 'NONE', *, *, #31700, .T. ) ;
#17697 = DIRECTION ( 'NONE',  ( 0.000000000000000000, 0.000000000000000000, 1.000000000000000000 ) ) ;
#17698 = ORIENTED_EDGE ( 'NONE', *, *, #38951, .T. ) ;
#17699 = LINE ( 'NONE', #37909, #38356 ) ;
#17700 = DIRECTION ( 'NONE',  ( 0.000000000000000000, -1.000000000000000000, 0.000000000000000000 ) ) ;
#17701 = DIRECTION ( 'NONE',  ( 0.000000000000000000, 0.000000000000000000, -1.000000000000000000 ) ) ;
#17702 = EDGE_CURVE ( 'NONE', #9413, #15564, #3049, .T. ) ;
#17703 = ORIENTED_EDGE ( 'NONE', *, *, #35594, .T. ) ;
#17704 = ORIENTED_EDGE ( 'NONE', *, *, #42744, .T. ) ;
#17705 = DIRECTION ( 'NONE',  ( 0.000000000000000000, -1.000000000000000000, -0.000000000000000000 ) ) ;
#17706 = DIRECTION ( 'NONE',  ( 0.000000000000000000, 0.000000000000000000, -1.000000000000000000 ) ) ;
#17707 = ORIENTED_EDGE ( 'NONE', *, *, #44895, .F. ) ;
#17708 = CARTESIAN_POINT ( 'NONE',  ( -336.3521761649654422, -119.0014323656137947, -58.88711093124865670 ) ) ;
#17709 = CIRCLE ( 'NONE', #47071, 125.0000000000000000 ) ;
#17710 = ORIENTED_EDGE ( 'NONE', *, *, #42030, .F. ) ;
#17711 = DIRECTION ( 'NONE',  ( -0.000000000000000000, 1.000000000000000000, -0.000000000000000000 ) ) ;
#17712 = CARTESIAN_POINT ( 'NONE',  ( -85.14888725715766782, -189.7472609257535510, 119.5003291395398719 ) ) ;
#17713 = AXIS2_PLACEMENT_3D ( 'NONE', #18937, #39159, #19971 ) ;
#17714 = ORIENTED_EDGE ( 'NONE', *, *, #27782, .F. ) ;
#17715 = PLANE ( 'NONE',  #583 ) ;
#17716 = ORIENTED_EDGE ( 'NONE', *, *, #40767, .F. ) ;
#17717 = DIRECTION ( 'NONE',  ( 0.9960498426152165630, 0.000000000000000000, 0.08879589532293852283 ) ) ;
#17718 = LINE ( 'NONE', #34249, #43222 ) ;
#17719 = CARTESIAN_POINT ( 'NONE',  ( 6.039888445539284056, -193.5000000000000000, 111.3726929437940498 ) ) ;
#17720 = ORIENTED_EDGE ( 'NONE', *, *, #10672, .T. ) ;
#17721 = DIRECTION ( 'NONE',  ( 0.000000000000000000, 0.000000000000000000, 1.000000000000000000 ) ) ;
#17722 = CARTESIAN_POINT ( 'NONE',  ( -49.30901192927172616, -189.7472609257535510, -123.9972451320097093 ) ) ;
#17723 = DIRECTION ( 'NONE',  ( 0.000000000000000000, 0.000000000000000000, 1.000000000000000000 ) ) ;
#17724 = EDGE_CURVE ( 'NONE', #30970, #46519, #33814, .T. ) ;
#17725 = CARTESIAN_POINT ( 'NONE',  ( -330.4913330509368166, -84.00150778970767362, -43.83057281297470098 ) ) ;
#17726 = VERTEX_POINT ( 'NONE', #50129 ) ;
#17727 = CARTESIAN_POINT ( 'NONE',  ( -48.47912675150885065, -177.1207230881787780, 6.938893903907228378E-15 ) ) ;
#17728 = ORIENTED_EDGE ( 'NONE', *, *, #24054, .F. ) ;
#17729 = VECTOR ( 'NONE', #46689, 1000.000000000000114 ) ;
#17730 = CARTESIAN_POINT ( 'NONE',  ( -130.7087404384255080, -193.5000000000000000, -94.14505102712755047 ) ) ;
#17732 = ORIENTED_EDGE ( 'NONE', *, *, #24726, .F. ) ;
#17731 = FACE_OUTER_BOUND ( 'NONE', #5250, .T. ) ;
#17733 = VERTEX_POINT ( 'NONE', #50899 ) ;
#17734 = DIRECTION ( 'NONE',  ( -0.000000000000000000, -0.2393156642875582940, -0.9709418174260519008 ) ) ;
#17735 = DIRECTION ( 'NONE',  ( 0.000000000000000000, 1.000000000000000000, 0.000000000000000000 ) ) ;
#17736 = ORIENTED_EDGE ( 'NONE', *, *, #41383, .T. ) ;
#17737 = DIRECTION ( 'NONE',  ( 0.000000000000000000, 1.000000000000000000, 0.000000000000000000 ) ) ;
#17738 = EDGE_CURVE ( 'NONE', #31384, #9916, #6749, .T. ) ;
#17739 = ORIENTED_EDGE ( 'NONE', *, *, #38223, .T. ) ;
#17740 = FACE_OUTER_BOUND ( 'NONE', #50184, .T. ) ;
#17741 = CARTESIAN_POINT ( 'NONE',  ( -339.1964088526558498, -102.1108035431470427, 54.98865587491797413 ) ) ;
#17742 = VECTOR ( 'NONE', #11354, 1000.000000000000000 ) ;
#17743 = DIRECTION ( 'NONE',  ( 5.399917434947259359E-17, 1.000000000000000000, -0.000000000000000000 ) ) ;
#17744 = DIRECTION ( 'NONE',  ( -1.000000000000000000, 0.000000000000000000, -0.000000000000000000 ) ) ;
#17745 = ORIENTED_EDGE ( 'NONE', *, *, #23709, .T. ) ;
#17746 = ORIENTED_EDGE ( 'NONE', *, *, #29928, .T. ) ;
#17747 = EDGE_CURVE ( 'NONE', #47759, #21174, #17349, .T. ) ;
#17749 = EDGE_LOOP ( 'NONE', ( #17062, #12835, #36686, #31294 ) ) ;
#17748 = VECTOR ( 'NONE', #4930, 1000.000000000000000 ) ;
#17750 = CARTESIAN_POINT ( 'NONE',  ( 6.443011874827240248, -177.1207230881787780, 112.2878385610370771 ) ) ;
#17751 = CARTESIAN_POINT ( 'NONE',  ( -332.3517673607765914, -81.08339623743702873, -41.09453333279329712 ) ) ;
#17752 = AXIS2_PLACEMENT_3D ( 'NONE', #26939, #43231, #7241 ) ;
#17753 = LINE ( 'NONE', #41642, #23660 ) ;
#17754 = CARTESIAN_POINT ( 'NONE',  ( 0.000000000000000000, -157.0158200571378018, 48.55604808772604741 ) ) ;
#17755 = ORIENTED_EDGE ( 'NONE', *, *, #15276, .F. ) ;
#17756 = ORIENTED_EDGE ( 'NONE', *, *, #8503, .T. ) ;
#17758 = ORIENTED_EDGE ( 'NONE', *, *, #27825, .T. ) ;
#17757 = CARTESIAN_POINT ( 'NONE',  ( -48.47912675150885065, -189.7472609257535510, 6.938893903907228378E-15 ) ) ;
#17759 = ORIENTED_EDGE ( 'NONE', *, *, #38752, .F. ) ;
#17760 = AXIS2_PLACEMENT_3D ( 'NONE', #594, #8472, #39740 ) ;
#17761 = DIRECTION ( 'NONE',  ( 0.000000000000000000, 0.8229838658936495799, -0.5680647467311656929 ) ) ;
#17762 = DIRECTION ( 'NONE',  ( -0.9646355819083556327, 0.000000000000000000, -0.2635871660690782825 ) ) ;
#17763 = FACE_OUTER_BOUND ( 'NONE', #30545, .T. ) ;
#17764 = CARTESIAN_POINT ( 'NONE',  ( 46.00000000000000711, 20.00000000000000000, -46.00000000000000000 ) ) ;
#17765 = ORIENTED_EDGE ( 'NONE', *, *, #2217, .T. ) ;
#17766 = DIRECTION ( 'NONE',  ( -1.000000000000000000, -0.000000000000000000, -5.782411586589357392E-17 ) ) ;
#17767 = ORIENTED_EDGE ( 'NONE', *, *, #2505, .F. ) ;
#17768 = ORIENTED_EDGE ( 'NONE', *, *, #22405, .T. ) ;
#17769 = LINE ( 'NONE', #42718, #44737 ) ;
#17770 = CARTESIAN_POINT ( 'NONE',  ( -336.3521761649654422, -126.1322888500942270, -59.00000000000001421 ) ) ;
#17771 = ORIENTED_EDGE ( 'NONE', *, *, #45564, .F. ) ;
#17772 = AXIS2_PLACEMENT_3D ( 'NONE', #19071, #35092, #19330 ) ;
#17773 = CARTESIAN_POINT ( 'NONE',  ( -238.7407812814481076, -193.5000000000000000, -9.999999999999987566 ) ) ;
#17774 = CARTESIAN_POINT ( 'NONE',  ( 53.56330073376472001, -193.5000000000000000, 72.19655804062048787 ) ) ;
#17775 = DIRECTION ( 'NONE',  ( 0.000000000000000000, -1.000000000000000000, 0.000000000000000000 ) ) ;
#17776 = EDGE_CURVE ( 'NONE', #51281, #49340, #32386, .T. ) ;
#17777 = VECTOR ( 'NONE', #6204, 999.9999999999998863 ) ;
#17778 = CARTESIAN_POINT ( 'NONE',  ( -339.1964088526558498, -182.5000000000000568, -0.4999999999999543698 ) ) ;
#17779 = AXIS2_PLACEMENT_3D ( 'NONE', #20548, #5579, #17141 ) ;
#17780 = DIRECTION ( 'NONE',  ( -0.000000000000000000, 1.000000000000000000, -0.000000000000000000 ) ) ;
#17781 = CARTESIAN_POINT ( 'NONE',  ( -330.4913330509368166, -71.49045607248250178, -27.86139516340898581 ) ) ;
#17782 = ORIENTED_EDGE ( 'NONE', *, *, #13134, .F. ) ;
#17783 = DIRECTION ( 'NONE',  ( 0.000000000000000000, 0.000000000000000000, 1.000000000000000000 ) ) ;
#17784 = VERTEX_POINT ( 'NONE', #6499 ) ;
#17785 = ORIENTED_EDGE ( 'NONE', *, *, #27298, .T. ) ;
#17786 = CARTESIAN_POINT ( 'NONE',  ( 67.66641500972446011, -193.5000000000000000, 46.20836643931067300 ) ) ;
#17787 = EDGE_LOOP ( 'NONE', ( #9522, #47857, #13560, #23688 ) ) ;
#17788 = VECTOR ( 'NONE', #19280, 1000.000000000000114 ) ;
#17789 = CARTESIAN_POINT ( 'NONE',  ( -34.51936650669026818, -189.7472609257535510, -124.2180546213278234 ) ) ;
#17790 = AXIS2_PLACEMENT_3D ( 'NONE', #38789, #7778, #43531 ) ;
#17791 = CARTESIAN_POINT ( 'NONE',  ( -166.9492939735806090, -193.5000000000000000, 39.87254040532603483 ) ) ;
#17793 = ORIENTED_EDGE ( 'NONE', *, *, #11114, .T. ) ;
#17792 = DIRECTION ( 'NONE',  ( 0.000000000000000000, 0.000000000000000000, -1.000000000000000000 ) ) ;
#17794 = ADVANCED_FACE ( 'NONE', ( #42747 ), #42209, .T. ) ;
#17795 = CARTESIAN_POINT ( 'NONE',  ( -280.0000000000000000, 0.000000000000000000, 0.000000000000000000 ) ) ;
#17796 = ORIENTED_EDGE ( 'NONE', *, *, #19737, .F. ) ;
#17797 = EDGE_LOOP ( 'NONE', ( #24222, #50606, #47913, #47549 ) ) ;
#17798 = ORIENTED_EDGE ( 'NONE', *, *, #8147, .T. ) ;
#17799 = CARTESIAN_POINT ( 'NONE',  ( -48.47912675150885065, -189.7472609257535510, 6.938893903907228378E-15 ) ) ;
#17800 = DIRECTION ( 'NONE',  ( 0.000000000000000000, 0.000000000000000000, -1.000000000000000000 ) ) ;
#17801 = SURFACE_STYLE_USAGE ( .BOTH. , #22250 ) ;
#17802 = CARTESIAN_POINT ( 'NONE',  ( -160.0000000000000284, -123.5000000000000284, 45.63467731922665394 ) ) ;
#17803 = DIRECTION ( 'NONE',  ( 0.000000000000000000, 0.000000000000000000, 1.000000000000000000 ) ) ;
#17804 = VECTOR ( 'NONE', #38102, 999.9999999999998863 ) ;
#17805 = ORIENTED_EDGE ( 'NONE', *, *, #24509, .T. ) ;
#17806 = CIRCLE ( 'NONE', #48763, 125.0000000000000000 ) ;
#17807 = AXIS2_PLACEMENT_3D ( 'NONE', #7119, #19215, #27338 ) ;
#17808 = DIRECTION ( 'NONE',  ( -0.000000000000000000, 1.000000000000000000, -0.000000000000000000 ) ) ;
#17809 = CARTESIAN_POINT ( 'NONE',  ( -48.47912675150885065, -177.1207230881787780, 6.938893903907228378E-15 ) ) ;
#17810 = ORIENTED_EDGE ( 'NONE', *, *, #51396, .F. ) ;
#17812 = VERTEX_POINT ( 'NONE', #34079 ) ;
#17811 = DIRECTION ( 'NONE',  ( 0.000000000000000000, 0.000000000000000000, -1.000000000000000000 ) ) ;
#17813 = ORIENTED_EDGE ( 'NONE', *, *, #5676, .T. ) ;
#17814 = ORIENTED_EDGE ( 'NONE', *, *, #17369, .T. ) ;
#17815 = DIRECTION ( 'NONE',  ( -8.718379230999705894E-17, 0.3546048870425363986, 0.9350162426854146114 ) ) ;
#17816 = DIRECTION ( 'NONE',  ( 0.000000000000000000, -1.000000000000000000, 0.000000000000000000 ) ) ;
#17817 = ORIENTED_EDGE ( 'NONE', *, *, #36627, .F. ) ;
#17818 = EDGE_CURVE ( 'NONE', #44900, #27780, #45929, .T. ) ;
#17819 = CARTESIAN_POINT ( 'NONE',  ( -336.3521761649654422, -128.9912765084839066, 58.76657425099337928 ) ) ;
#17820 = DIRECTION ( 'NONE',  ( -1.000000000000000000, 0.000000000000000000, 0.000000000000000000 ) ) ;
#17821 = ORIENTED_EDGE ( 'NONE', *, *, #33392, .T. ) ;
#17822 = DIRECTION ( 'NONE',  ( 0.000000000000000000, 0.000000000000000000, -1.000000000000000000 ) ) ;
#17823 = ORIENTED_EDGE ( 'NONE', *, *, #28134, .F. ) ;
#17824 = AXIS2_PLACEMENT_3D ( 'NONE', #20487, #36013, #36513 ) ;
#17825 = VECTOR ( 'NONE', #6772, 1000.000000000000000 ) ;
#17826 = ADVANCED_FACE ( 'NONE', ( #22525 ), #30136, .T. ) ;
#17827 = ORIENTED_EDGE ( 'NONE', *, *, #21604, .F. ) ;
#17828 = PLANE ( 'NONE',  #1023 ) ;
#17829 = CIRCLE ( 'NONE', #1010, 60.00000000000000000 ) ;
#17831 = AXIS2_PLACEMENT_3D ( 'NONE', #26131, #5406, #45866 ) ;
#17830 = LINE ( 'NONE', #37788, #20557 ) ;
#17832 = DIRECTION ( 'NONE',  ( 0.000000000000000000, 1.000000000000000000, 0.000000000000000000 ) ) ;
#17833 = ORIENTED_EDGE ( 'NONE', *, *, #8173, .T. ) ;
#17834 = DIRECTION ( 'NONE',  ( -0.000000000000000000, 0.000000000000000000, -1.000000000000000000 ) ) ;
#17835 = DIRECTION ( 'NONE',  ( -0.8610436117673621048, 0.000000000000000000, 0.5085311186492095237 ) ) ;
#17836 = LINE ( 'NONE', #4985, #49817 ) ;
#17837 = EDGE_CURVE ( 'NONE', #6578, #38717, #10160, .T. ) ;
#17838 = ORIENTED_EDGE ( 'NONE', *, *, #12561, .F. ) ;
#17839 = DIRECTION ( 'NONE',  ( -0.000000000000000000, 1.000000000000000000, 0.000000000000000000 ) ) ;
#17840 = LINE ( 'NONE', #6009, #23162 ) ;
#17841 = ADVANCED_FACE ( 'NONE', ( #26178 ), #6228, .T. ) ;
#17842 = CARTESIAN_POINT ( 'NONE',  ( -365.0000000000001137, -168.5000000000000284, 0.000000000000000000 ) ) ;
#17843 = ORIENTED_EDGE ( 'NONE', *, *, #46587, .F. ) ;
#17844 = EDGE_CURVE ( 'NONE', #50110, #25185, #22772, .T. ) ;
#17845 = CARTESIAN_POINT ( 'NONE',  ( -15.24927435600542402, -177.1207230881787780, 120.5021863277718950 ) ) ;
#17846 = CIRCLE ( 'NONE', #37975, 60.00000000000000000 ) ;
#17847 = DIRECTION ( 'NONE',  ( 0.000000000000000000, 0.000000000000000000, -1.000000000000000000 ) ) ;
#17848 = CARTESIAN_POINT ( 'NONE',  ( -336.3521761649654422, -82.40546666720629787, 42.41660376256258047 ) ) ;
#17849 = ORIENTED_EDGE ( 'NONE', *, *, #13850, .T. ) ;
#17850 = CARTESIAN_POINT ( 'NONE',  ( 58.45385938022562300, -177.1207230881787780, 62.78108192022012446 ) ) ;
#17851 = VERTEX_POINT ( 'NONE', #7523 ) ;
#17852 = VECTOR ( 'NONE', #15526, 1000.000000000000000 ) ;
#17853 = PLANE ( 'NONE',  #5815 ) ;
#17854 = CARTESIAN_POINT ( 'NONE',  ( 1.734723475976807094E-15, 0.000000000000000000, 46.00000000000000711 ) ) ;
#17855 = CARTESIAN_POINT ( 'NONE',  ( -49.44376233341720450, -193.5000000000000000, -0.2635871660690713436 ) ) ;
#17856 = EDGE_CURVE ( 'NONE', #5586, #31784, #35360, .T. ) ;
#17857 = DIRECTION ( 'NONE',  ( 0.000000000000000000, -0.7485107481711089639, -0.6631226582407863113 ) ) ;
#17858 = PLANE ( 'NONE',  #35295 ) ;
#17859 = VECTOR ( 'NONE', #47526, 1000.000000000000000 ) ;
#17860 = EDGE_LOOP ( 'NONE', ( #29554, #44815, #48290, #8793 ) ) ;
#17861 = VECTOR ( 'NONE', #29573, 1000.000000000000000 ) ;
#17862 = CARTESIAN_POINT ( 'NONE',  ( -336.3521761649654422, -177.7325358280884586, 23.38292116578760726 ) ) ;
#17863 = EDGE_LOOP ( 'NONE', ( #23219, #38330, #4217, #17152 ) ) ;
#17864 = LINE ( 'NONE', #33879, #51925 ) ;
#17865 = AXIS2_PLACEMENT_3D ( 'NONE', #51982, #27767, #3350 ) ;
#17866 = AXIS2_PLACEMENT_3D ( 'NONE', #45112, #5892, #37144 ) ;
#17867 = ORIENTED_EDGE ( 'NONE', *, *, #6310, .F. ) ;
#17868 = DIRECTION ( 'NONE',  ( 0.000000000000000000, 0.000000000000000000, -1.000000000000000000 ) ) ;
#17869 = ORIENTED_EDGE ( 'NONE', *, *, #5523, .F. ) ;
#17870 = CLOSED_SHELL ( 'NONE', ( #8562, #9904, #21979, #22293, #26666, #41088, #49623, #34603, #27984, #22646, #14745, #12348, #46832, #51530 ) ) ;
#17871 = DIRECTION ( 'NONE',  ( 0.000000000000000000, -0.000000000000000000, 1.000000000000000000 ) ) ;
#17872 = CARTESIAN_POINT ( 'NONE',  ( 74.68865188374466868, -193.5000000000000000, 14.34663989163627562 ) ) ;
#17873 = ORIENTED_EDGE ( 'NONE', *, *, #25153, .T. ) ;
#17876 = VERTEX_POINT ( 'NONE', #20114 ) ;
#17875 = FACE_OUTER_BOUND ( 'NONE', #47456, .T. ) ;
#17874 = CARTESIAN_POINT ( 'NONE',  ( -40.90423906728908321, -175.3837268820161057, -124.7702732086912221 ) ) ;
#17877 = CARTESIAN_POINT ( 'NONE',  ( -105.7090724259148118, -193.5000000000000000, 111.1293539894142839 ) ) ;
#17878 = VERTEX_POINT ( 'NONE', #39555 ) ;
#17879 = CARTESIAN_POINT ( 'NONE',  ( 4.109287492203100634, -177.1207230881787780, -113.3995532942336979 ) ) ;
#17880 = VECTOR ( 'NONE', #31721, 1000.000000000000000 ) ;
#17881 = ORIENTED_EDGE ( 'NONE', *, *, #7337, .F. ) ;
#17882 = EDGE_CURVE ( 'NONE', #46508, #4562, #51170, .T. ) ;
#17883 = EDGE_CURVE ( 'NONE', #10308, #7533, #11961, .T. ) ;
#17884 = DIRECTION ( 'NONE',  ( 0.000000000000000000, 0.000000000000000000, -1.000000000000000000 ) ) ;
#17887 = ORIENTED_EDGE ( 'NONE', *, *, #13139, .T. ) ;
#17886 = CARTESIAN_POINT ( 'NONE',  ( -330.4913330509368166, -123.5000000000000284, 0.000000000000000000 ) ) ;
#17885 = DIRECTION ( 'NONE',  ( 0.000000000000000000, 1.119474883163699554E-13, 1.000000000000000000 ) ) ;
#17888 = ORIENTED_EDGE ( 'NONE', *, *, #12234, .T. ) ;
#17889 = AXIS2_PLACEMENT_3D ( 'NONE', #42918, #27142, #50317 ) ;
#17890 = DIRECTION ( 'NONE',  ( -0.000000000000000000, 1.000000000000000000, -0.000000000000000000 ) ) ;
#17891 = ORIENTED_EDGE ( 'NONE', *, *, #1695, .T. ) ;
#17892 = PLANE ( 'NONE',  #37076 ) ;
#17893 = LINE ( 'NONE', #49952, #23165 ) ;
#17894 = VERTEX_POINT ( 'NONE', #19858 ) ;
#17895 = DIRECTION ( 'NONE',  ( -0.000000000000000000, -0.8854560256532126861, -0.4647231720437631775 ) ) ;
#17896 = DIRECTION ( 'NONE',  ( 0.000000000000000000, -1.000000000000000000, 0.000000000000000000 ) ) ;
#17897 = DIRECTION ( 'NONE',  ( -0.000000000000000000, 0.6631226582407965253, 0.7485107481711000821 ) ) ;
#17898 = CARTESIAN_POINT ( 'NONE',  ( -305.0000000000000568, -181.8741440471346493, 13.87297036558422647 ) ) ;
#17899 = ORIENTED_EDGE ( 'NONE', *, *, #28332, .F. ) ;
#17900 =( NAMED_UNIT ( * ) PLANE_ANGLE_UNIT ( ) SI_UNIT ( $, .RADIAN. ) );
#17901 = ADVANCED_FACE ( 'NONE', ( #15932 ), #3833, .T. ) ;
#17902 = AXIS2_PLACEMENT_3D ( 'NONE', #49966, #37620, #29715 ) ;
#17903 = DIRECTION ( 'NONE',  ( -0.000000000000000000, 1.000000000000000000, -0.000000000000000000 ) ) ;
#17904 = AXIS2_PLACEMENT_3D ( 'NONE', #4095, #1101, #31933 ) ;
#17905 = CARTESIAN_POINT ( 'NONE',  ( -48.82732838694325750, -189.7472609257535510, 0.9374196611341252261 ) ) ;
#17906 = ADVANCED_FACE ( 'NONE', ( #24321 ), #32199, .F. ) ;
#17907 = LINE ( 'NONE', #49708, #46410 ) ;
#17908 = ORIENTED_EDGE ( 'NONE', *, *, #51554, .F. ) ;
#17909 = CIRCLE ( 'NONE', #18725, 20.00000000000001776 ) ;
#17910 = ADVANCED_FACE ( 'NONE', ( #51418 ), #12221, .F. ) ;
#17911 = LINE ( 'NONE', #37348, #20603 ) ;
#17912 = FACE_OUTER_BOUND ( 'NONE', #37775, .T. ) ;
#17913 = EDGE_CURVE ( 'NONE', #16796, #3069, #27483, .T. ) ;
#17914 = FACE_OUTER_BOUND ( 'NONE', #39913, .T. ) ;
#17915 = DIRECTION ( 'NONE',  ( 1.000000000000000000, -0.000000000000000000, -0.000000000000000000 ) ) ;
#17916 = CIRCLE ( 'NONE', #50620, 125.0000000000000000 ) ;
#17917 = FACE_OUTER_BOUND ( 'NONE', #7263, .T. ) ;
#17918 = CARTESIAN_POINT ( 'NONE',  ( -49.46816693883101124, -193.5000000000000000, -0.1476465640024848536 ) ) ;
#17919 = DIRECTION ( 'NONE',  ( -0.000000000000000000, 1.000000000000000000, -0.000000000000000000 ) ) ;
#17921 = ORIENTED_EDGE ( 'NONE', *, *, #33334, .F. ) ;
#17920 = CARTESIAN_POINT ( 'NONE',  ( -48.47912675150885065, -183.6283474603465606, 6.938893903907228378E-15 ) ) ;
#17922 = ORIENTED_EDGE ( 'NONE', *, *, #45979, .T. ) ;
#17923 = AXIS2_PLACEMENT_3D ( 'NONE', #18855, #23068, #51452 ) ;
#17924 = DIRECTION ( 'NONE',  ( 0.000000000000000000, 0.000000000000000000, 1.000000000000000000 ) ) ;
#17926 = ORIENTED_EDGE ( 'NONE', *, *, #19844, .F. ) ;
#17925 = CARTESIAN_POINT ( 'NONE',  ( -172.0602536473422504, -193.5000000000000000, -10.18383939837523755 ) ) ;
#17927 = ADVANCED_FACE ( 'NONE', ( #27734 ), #8296, .T. ) ;
#17928 = ORIENTED_EDGE ( 'NONE', *, *, #52010, .T. ) ;
#17929 = EDGE_LOOP ( 'NONE', ( #5446, #51532, #24702, #32100 ) ) ;
#17930 = LINE ( 'NONE', #21878, #44330 ) ;
#17931 = CYLINDRICAL_SURFACE ( 'NONE', #32825, 125.0000000000000000 ) ;
#17932 = PLANE ( 'NONE',  #36374 ) ;
#17934 = ORIENTED_EDGE ( 'NONE', *, *, #31389, .T. ) ;
#17933 = VECTOR ( 'NONE', #30534, 1000.000000000000000 ) ;
#17935 = EDGE_CURVE ( 'NONE', #49256, #38482, #19095, .T. ) ;
#17936 = CARTESIAN_POINT ( 'NONE',  ( -48.47912675150885065, -175.3837268820161057, 6.938893903907228378E-15 ) ) ;
#17937 = DIRECTION ( 'NONE',  ( -0.000000000000000000, 1.000000000000000000, -0.000000000000000000 ) ) ;
#17939 = ORIENTED_EDGE ( 'NONE', *, *, #3903, .F. ) ;
#17938 = DIRECTION ( 'NONE',  ( 0.000000000000000000, 0.000000000000000000, -1.000000000000000000 ) ) ;
#17940 = VECTOR ( 'NONE', #11211, 1000.000000000000000 ) ;
#17941 = CARTESIAN_POINT ( 'NONE',  ( -160.0000000000000284, -123.5000000000000284, 45.63467731922665394 ) ) ;
#17942 = VERTEX_POINT ( 'NONE', #47979 ) ;
#17943 = CARTESIAN_POINT ( 'NONE',  ( -336.3521761649654422, -120.8677111499054320, 59.00000000000000000 ) ) ;
#17944 = EDGE_LOOP ( 'NONE', ( #22261, #21063, #35775, #9477 ) ) ;
#17945 = EDGE_CURVE ( 'NONE', #1126, #21250, #5643, .T. ) ;
#17946 = ADVANCED_FACE ( 'NONE', ( #47215 ), #44029, .T. ) ;
#17947 = ADVANCED_FACE ( 'NONE', ( #7771 ), #16184, .F. ) ;
#17948 = ADVANCED_FACE ( 'NONE', ( #39312 ), #4100, .F. ) ;
#17949 = LINE ( 'NONE', #14265, #8130 ) ;
#17950 = CARTESIAN_POINT ( 'NONE',  ( 18.00181100848376303, -177.1207230881787780, -105.8550183720733742 ) ) ;
#17951 = LINE ( 'NONE', #49508, #20701 ) ;
#17952 = EDGE_CURVE ( 'NONE', #50350, #12133, #51778, .T. ) ;
#17953 = ORIENTED_EDGE ( 'NONE', *, *, #617, .F. ) ;
#17954 = ORIENTED_EDGE ( 'NONE', *, *, #43568, .F. ) ;
#17955 = CARTESIAN_POINT ( 'NONE',  ( -8.169009709621407822, -183.6283474603465606, 118.3219948448695504 ) ) ;
#17956 = DIRECTION ( 'NONE',  ( 0.000000000000000000, -1.000000000000000000, 0.000000000000000000 ) ) ;
#17957 = VERTEX_POINT ( 'NONE', #31421 ) ;
#17958 = EDGE_CURVE ( 'NONE', #33929, #24680, #47462, .T. ) ;
#17959 = DIRECTION ( 'NONE',  ( 0.000000000000000000, 0.9927088740980544168, 0.1205366802553199251 ) ) ;
#17960 = AXIS2_PLACEMENT_3D ( 'NONE', #11228, #26221, #10202 ) ;
#17961 = ORIENTED_EDGE ( 'NONE', *, *, #52008, .T. ) ;
#17962 = DIRECTION ( 'NONE',  ( -0.9027978299657477557, 0.000000000000000000, 0.4300652022765115712 ) ) ;
#17963 = EDGE_CURVE ( 'NONE', #20252, #45739, #391, .T. ) ;
#17965 = VECTOR ( 'NONE', #51202, 1000.000000000000114 ) ;
#17964 = CARTESIAN_POINT ( 'NONE',  ( -164.6246685127424882, -175.3837268820161057, -46.20836643930982035 ) ) ;
#17966 = ADVANCED_FACE ( 'NONE', ( #32722 ), #33237, .T. ) ;
#17967 = VERTEX_POINT ( 'NONE', #24836 ) ;
#17968 = LINE ( 'NONE', #41873, #5639 ) ;
#17969 = ORIENTED_EDGE ( 'NONE', *, *, #17612, .T. ) ;
#17970 = ADVANCED_FACE ( 'NONE', ( #918 ), #12734, .T. ) ;
#17971 = CARTESIAN_POINT ( 'NONE',  ( 5.542374969221969039, -193.5000000000000000, 112.7238987608088365 ) ) ;
#17972 = DIRECTION ( 'NONE',  ( 0.000000000000000000, -1.000000000000000000, 0.000000000000000000 ) ) ;
#17973 = ORIENTED_EDGE ( 'NONE', *, *, #36585, .T. ) ;
#17974 = EDGE_CURVE ( 'NONE', #38255, #15864, #42530, .T. ) ;
#17975 = PLANE ( 'NONE',  #46231 ) ;
#17976 = CARTESIAN_POINT ( 'NONE',  ( -336.3521761649654422, -65.58448481710581746, 11.56382487286456140 ) ) ;
#17977 = PLANE ( 'NONE',  #35788 ) ;
#17978 = VECTOR ( 'NONE', #32532, 1000.000000000000227 ) ;
#17979 = DIRECTION ( 'NONE',  ( 0.000000000000000000, 5.851800525628429686E-14, -1.000000000000000000 ) ) ;
#17980 = EDGE_CURVE ( 'NONE', #1552, #31094, #20370, .T. ) ;
#17981 = ORIENTED_EDGE ( 'NONE', *, *, #2760, .T. ) ;
#17982 = LINE ( 'NONE', #34760, #17012 ) ;
#17983 = EDGE_LOOP ( 'NONE', ( #24934, #31619, #31767, #33984 ) ) ;
#17984 = CARTESIAN_POINT ( 'NONE',  ( 46.00000000000000711, 20.00000000000000000, -46.00000000000000000 ) ) ;
#17986 = ORIENTED_EDGE ( 'NONE', *, *, #41504, .F. ) ;
#17985 = DIRECTION ( 'NONE',  ( -0.9027978299657387629, 0.000000000000000000, -0.4300652022765304450 ) ) ;
#17987 = ORIENTED_EDGE ( 'NONE', *, *, #18778, .F. ) ;
#17988 = EDGE_CURVE ( 'NONE', #45870, #12420, #29088, .T. ) ;
#17989 = EDGE_CURVE ( 'NONE', #10439, #6696, #21414, .T. ) ;
#17990 = CARTESIAN_POINT ( 'NONE',  ( -336.3521761649654422, -177.7325358280884586, 23.38292116578760726 ) ) ;
#17991 = ORIENTED_EDGE ( 'NONE', *, *, #32991, .T. ) ;
#17992 = PLANE ( 'NONE',  #11341 ) ;
#17993 = ORIENTED_EDGE ( 'NONE', *, *, #48739, .T. ) ;
#17994 = LINE ( 'NONE', #42677, #20812 ) ;
#17995 = CARTESIAN_POINT ( 'NONE',  ( -339.1964088526558498, -150.4759391377560576, -52.47426709956116042 ) ) ;
#17996 = VECTOR ( 'NONE', #35832, 1000.000000000000114 ) ;
#17997 = VECTOR ( 'NONE', #29384, 1000.000000000000000 ) ;
#17998 = LINE ( 'NONE', #5920, #14343 ) ;
#17999 = CARTESIAN_POINT ( 'NONE',  ( -161.4184887245413904, -177.1207230881787780, 51.19472891551358629 ) ) ;
#18000 = ORIENTED_EDGE ( 'NONE', *, *, #39806, .F. ) ;
#18001 = ORIENTED_EDGE ( 'NONE', *, *, #37233, .T. ) ;
#18002 = AXIS2_PLACEMENT_3D ( 'NONE', #47435, #35339, #16421 ) ;
#18003 = EDGE_LOOP ( 'NONE', ( #5032, #44271, #43419, #19110 ) ) ;
#18004 = DIRECTION ( 'NONE',  ( 0.000000000000000000, -1.000000000000000000, 0.000000000000000000 ) ) ;
#18005 = DIRECTION ( 'NONE',  ( 1.043714542225393381E-14, 0.8229838658936613482, 0.5680647467311485954 ) ) ;
#18006 = CARTESIAN_POINT ( 'NONE',  ( -118.4510020108455706, -189.7472609257535510, 103.5805805771131105 ) ) ;
#18007 = CARTESIAN_POINT ( 'NONE',  ( 48.47907891923915713, -193.5000000000000000, 78.89300572996904748 ) ) ;
#18008 = EDGE_LOOP ( 'NONE', ( #34136, #41151, #43954, #37754 ) ) ;
#18009 = EDGE_CURVE ( 'NONE', #16186, #32301, #541, .T. ) ;
#18010 = ADVANCED_FACE ( 'NONE', ( #4883, #20910 ), #5399, .T. ) ;
#18011 = VECTOR ( 'NONE', #33768, 1000.000000000000114 ) ;
#18012 = EDGE_CURVE ( 'NONE', #34105, #19012, #3939, .T. ) ;
#18013 = ADVANCED_FACE ( 'NONE', ( #37182 ), #8799, .T. ) ;
#18014 = ORIENTED_EDGE ( 'NONE', *, *, #1500, .F. ) ;
#18016 = ORIENTED_EDGE ( 'NONE', *, *, #32778, .F. ) ;
#18015 = PLANE ( 'NONE',  #16463 ) ;
#18017 = CARTESIAN_POINT ( 'NONE',  ( -157.5429198988176438, -193.5000000000000000, 61.07445476073480961 ) ) ;
#18018 = CARTESIAN_POINT ( 'NONE',  ( -305.0000000000000568, -65.92952926200918284, -16.90091414705545247 ) ) ;
#18019 = CARTESIAN_POINT ( 'NONE',  ( -332.3517673607765914, -99.78295912235451226, 55.11353710303931308 ) ) ;
#18020 = CARTESIAN_POINT ( 'NONE',  ( -6.081033889300858419, -175.3837268820161057, -116.5264228893325651 ) ) ;
#18021 = CARTESIAN_POINT ( 'NONE',  ( -305.0000000000000568, -142.2945752170892035, 56.98038208374156000 ) ) ;
#18022 = EDGE_LOOP ( 'NONE', ( #16940, #9396, #19459, #4816 ) ) ;
#18023 = CARTESIAN_POINT ( 'NONE',  ( -332.3517673607765914, -173.5513585866778214, -31.34948880313881503 ) ) ;
#18024 = VERTEX_POINT ( 'NONE', #17222 ) ;
#18025 = ORIENTED_EDGE ( 'NONE', *, *, #44439, .T. ) ;
#18026 = DIRECTION ( 'NONE',  ( 0.000000000000000000, 0.000000000000000000, -1.000000000000000000 ) ) ;
#18027 = DIRECTION ( 'NONE',  ( -0.000000000000000000, 0.4647231720437664526, -0.8854560256532110207 ) ) ;
#18028 = ORIENTED_EDGE ( 'NONE', *, *, #38400, .F. ) ;
#18029 = CIRCLE ( 'NONE', #7916, 125.0000000000000000 ) ;
#18030 = CIRCLE ( 'NONE', #48230, 15.24495751795539000 ) ;
#18031 = CARTESIAN_POINT ( 'NONE',  ( 2.390048994689175825E-16, 100.2299100483172936, -102.2100286647267779 ) ) ;
#18032 = FACE_OUTER_BOUND ( 'NONE', #51962, .T. ) ;
#18033 = DIRECTION ( 'NONE',  ( -0.2348860457809842095, 0.000000000000000000, 0.9720229140804107493 ) ) ;
#18034 = DIRECTION ( 'NONE',  ( 0.000000000000000000, 0.1205366802553268363, 0.9927088740980534176 ) ) ;
#18035 = VECTOR ( 'NONE', #28301, 1000.000000000000000 ) ;
#18036 = EDGE_CURVE ( 'NONE', #46272, #7639, #12325, .T. ) ;
#18037 = FACE_OUTER_BOUND ( 'NONE', #51618, .T. ) ;
#18038 = ORIENTED_EDGE ( 'NONE', *, *, #45435, .T. ) ;
#18039 = VECTOR ( 'NONE', #26781, 1000.000000000000000 ) ;
#18040 = FACE_OUTER_BOUND ( 'NONE', #49187, .T. ) ;
#18041 = ORIENTED_EDGE ( 'NONE', *, *, #44644, .F. ) ;
#18042 = ORIENTED_EDGE ( 'NONE', *, *, #18783, .F. ) ;
#18043 = DIRECTION ( 'NONE',  ( 0.9473263538541899509, 0.000000000000000000, 0.3202698538628415692 ) ) ;
#18044 = VERTEX_POINT ( 'NONE', #21154 ) ;
#18045 = LINE ( 'NONE', #42201, #47809 ) ;
#18046 = LINE ( 'NONE', #34575, #43571 ) ;
#18048 = ORIENTED_EDGE ( 'NONE', *, *, #35305, .T. ) ;
#18047 = DIRECTION ( 'NONE',  ( 1.000000000000000000, -0.000000000000000000, -0.000000000000000000 ) ) ;
#18049 = DIRECTION ( 'NONE',  ( 0.000000000000000000, 0.000000000000000000, 1.000000000000000000 ) ) ;
#18050 = DIRECTION ( 'NONE',  ( 0.000000000000000000, -1.000000000000000000, -0.000000000000000000 ) ) ;
#18051 = CARTESIAN_POINT ( 'NONE',  ( -339.1964088526558498, -68.15673923803898049, 20.45418021416614351 ) ) ;
#18052 = VERTEX_POINT ( 'NONE', #28508 ) ;
#18053 = VERTEX_POINT ( 'NONE', #29298 ) ;
#18054 = ORIENTED_EDGE ( 'NONE', *, *, #41136, .F. ) ;
#18055 = CARTESIAN_POINT ( 'NONE',  ( -48.47912675150885065, -183.6283474603465606, 6.938893903907228378E-15 ) ) ;
#18056 = DIRECTION ( 'NONE',  ( 0.6300878435817148793, 0.000000000000000000, -0.7765238627180394149 ) ) ;
#18057 = AXIS2_PLACEMENT_3D ( 'NONE', #42119, #45818, #1134 ) ;
#18058 = LINE ( 'NONE', #30643, #40211 ) ;
#18059 = AXIS2_PLACEMENT_3D ( 'NONE', #11398, #51619, #43205 ) ;
#18060 = CARTESIAN_POINT ( 'NONE',  ( -15.81236726369125023, -177.1207230881787780, -120.6560517527615417 ) ) ;
#18061 = DIRECTION ( 'NONE',  ( 0.000000000000000000, -0.2393156642875615969, -0.9709418174260511236 ) ) ;
#18062 = VERTEX_POINT ( 'NONE', #8537 ) ;
#18063 = AXIS2_PLACEMENT_3D ( 'NONE', #30423, #50170, #6263 ) ;
#18064 = EDGE_CURVE ( 'NONE', #9404, #21667, #45349, .T. ) ;
#18065 = VECTOR ( 'NONE', #35094, 1000.000000000000000 ) ;
#18066 = CARTESIAN_POINT ( 'NONE',  ( -48.47912675150885065, -189.7472609257535510, 6.938893903907228378E-15 ) ) ;
#18067 = ORIENTED_EDGE ( 'NONE', *, *, #39063, .T. ) ;
#18069 = ORIENTED_EDGE ( 'NONE', *, *, #48803, .T. ) ;
#18068 = PLANE ( 'NONE',  #20574 ) ;
#18070 = ORIENTED_EDGE ( 'NONE', *, *, #51554, .T. ) ;
#18071 = CARTESIAN_POINT ( 'NONE',  ( 52.98246549829695340, -193.5000000000000000, 73.01058346660533971 ) ) ;
#18072 = CIRCLE ( 'NONE', #49970, 125.0000000000000000 ) ;
#18073 = ORIENTED_EDGE ( 'NONE', *, *, #27742, .T. ) ;
#18074 = DIRECTION ( 'NONE',  ( -0.000000000000000000, 1.000000000000000000, -0.000000000000000000 ) ) ;
#18075 = CIRCLE ( 'NONE', #6341, 124.9999999999999858 ) ;
#18076 = ORIENTED_EDGE ( 'NONE', *, *, #30466, .F. ) ;
#18077 = LINE ( 'NONE', #34103, #24524 ) ;
#18078 = FACE_OUTER_BOUND ( 'NONE', #683, .T. ) ;
#18079 = ORIENTED_EDGE ( 'NONE', *, *, #37242, .F. ) ;
#18080 = DIRECTION ( 'NONE',  ( 1.000000000000000000, -0.000000000000000000, -0.000000000000000000 ) ) ;
#18081 = AXIS2_PLACEMENT_3D ( 'NONE', #25243, #17111, #531 ) ;
#18082 = EDGE_LOOP ( 'NONE', ( #42337, #11323, #33106, #1401 ) ) ;
#18083 = VECTOR ( 'NONE', #1831, 1000.000000000000114 ) ;
#18084 = VERTEX_POINT ( 'NONE', #41380 ) ;
#18085 = CARTESIAN_POINT ( 'NONE',  ( -13.05859477122062273, -189.7472609257535510, -118.8334608768479796 ) ) ;
#18086 = DIRECTION ( 'NONE',  ( -0.9473263538541876194, 0.000000000000000000, -0.3202698538628486746 ) ) ;
#18087 = EDGE_CURVE ( 'NONE', #21790, #36146, #26580, .T. ) ;
#18088 = CARTESIAN_POINT ( 'NONE',  ( -48.98765787015808115, -189.7472609257535510, 0.8610436117673582190 ) ) ;
#18089 = VERTEX_POINT ( 'NONE', #29550 ) ;
#18090 = PLANE ( 'NONE',  #48366 ) ;
#18091 = CARTESIAN_POINT ( 'NONE',  ( -41.90263914168912152, -175.3837268820161057, -124.8268793598473536 ) ) ;
#18092 = ITEM_DEFINED_TRANSFORMATION ( 'NONE', 'NONE', #18366,  #31742 ) ;
#18093 = DIRECTION ( 'NONE',  ( 0.000000000000000000, 0.000000000000000000, -1.000000000000000000 ) ) ;
#18094 = CARTESIAN_POINT ( 'NONE',  ( -60.00000000000000000, -63.50000000000000000, -0.000000000000000000 ) ) ;
#18095 = ORIENTED_EDGE ( 'NONE', *, *, #45847, .F. ) ;
#18096 = PLANE ( 'NONE',  #31368 ) ;
#18097 = CARTESIAN_POINT ( 'NONE',  ( 74.48795740376233709, -193.5000000000000000, -15.97798378892164806 ) ) ;
#18098 = LINE ( 'NONE', #9439, #33263 ) ;
#18099 = ORIENTED_EDGE ( 'NONE', *, *, #1467, .F. ) ;
#18100 = ORIENTED_EDGE ( 'NONE', *, *, #42671, .T. ) ;
#18101 = VECTOR ( 'NONE', #31068, 1000.000000000000000 ) ;
#18102 = DIRECTION ( 'NONE',  ( 0.000000000000000000, 0.000000000000000000, 1.000000000000000000 ) ) ;
#18103 = VECTOR ( 'NONE', #22412, 1000.000000000000000 ) ;
#18104 = VECTOR ( 'NONE', #2899, 1000.000000000000000 ) ;
#18105 = DIRECTION ( 'NONE',  ( -0.000000000000000000, -1.000000000000000000, 0.000000000000000000 ) ) ;
#18106 = ORIENTED_EDGE ( 'NONE', *, *, #18496, .F. ) ;
#18107 = LINE ( 'NONE', #45712, #28759 ) ;
#18108 = EDGE_CURVE ( 'NONE', #38792, #8523, #49552, .T. ) ;
#18109 = ORIENTED_EDGE ( 'NONE', *, *, #51972, .F. ) ;
#18110 = DIRECTION ( 'NONE',  ( 0.000000000000000000, 0.000000000000000000, 1.000000000000000000 ) ) ;
#18111 = CARTESIAN_POINT ( 'NONE',  ( -166.9492939735806090, -175.3837268820161057, 39.87254040532603483 ) ) ;
#18112 = VECTOR ( 'NONE', #33126, 1000.000000000000000 ) ;
#18113 = CARTESIAN_POINT ( 'NONE',  ( -6.938893903907228378E-15, -63.50000000000000000, 0.000000000000000000 ) ) ;
#18114 = AXIS2_PLACEMENT_3D ( 'NONE', #18637, #9988, #13920 ) ;
#18115 = DIRECTION ( 'NONE',  ( 0.000000000000000000, 0.9350162426854158326, 0.3546048870425331234 ) ) ;
#18116 = CIRCLE ( 'NONE', #31532, 125.0000000000000000 ) ;
#18117 = CARTESIAN_POINT ( 'NONE',  ( -336.3521761649654422, -64.61288906875131488, 4.498567634385603142 ) ) ;
#18118 = ORIENTED_EDGE ( 'NONE', *, *, #16740, .F. ) ;
#18119 = DIRECTION ( 'NONE',  ( 0.000000000000000000, 0.3546048870425426158, 0.9350162426854121689 ) ) ;
#18120 = EDGE_CURVE ( 'NONE', #4224, #1505, #9852, .T. ) ;
#18121 = ORIENTED_EDGE ( 'NONE', *, *, #26390, .F. ) ;
#18122 = CIRCLE ( 'NONE', #41586, 125.0000000000000000 ) ;
#18123 = DIRECTION ( 'NONE',  ( 0.000000000000000000, 0.000000000000000000, 1.000000000000000000 ) ) ;
#18124 = VERTEX_POINT ( 'NONE', #17999 ) ;
#18125 = LINE ( 'NONE', #34150, #35992 ) ;
#18126 = EDGE_CURVE ( 'NONE', #31030, #50561, #37956, .T. ) ;
#18127 = EDGE_CURVE ( 'NONE', #37502, #16440, #44220, .T. ) ;
#18128 = DIRECTION ( 'NONE',  ( 0.4031234292879730674, 0.000000000000000000, -0.9151456172430181280 ) ) ;
#18129 = DIRECTION ( 'NONE',  ( -0.000000000000000000, 0.000000000000000000, 1.000000000000000000 ) ) ;
#18130 = ORIENTED_EDGE ( 'NONE', *, *, #2522, .T. ) ;
#18133 = VERTEX_POINT ( 'NONE', #21934 ) ;
#18132 = CARTESIAN_POINT ( 'NONE',  ( -339.1964088526558498, -171.7720157143604069, -33.92731199008472487 ) ) ;
#18131 = PLANE ( 'NONE',  #30043 ) ;
#18134 = EDGE_CURVE ( 'NONE', #23565, #32390, #50836, .T. ) ;
#18135 = VECTOR ( 'NONE', #13634, 1000.000000000000000 ) ;
#18136 = CARTESIAN_POINT ( 'NONE',  ( -336.3521761649653854, -65.65568511206123503, -15.93848283698870105 ) ) ;
#18137 = VECTOR ( 'NONE', #26537, 1000.000000000000000 ) ;
#18138 = ORIENTED_EDGE ( 'NONE', *, *, #4612, .T. ) ;
#18139 = CARTESIAN_POINT ( 'NONE',  ( -51.89154260666836649, -177.1207230881787780, 124.9534129907280970 ) ) ;
#18140 = ORIENTED_EDGE ( 'NONE', *, *, #49738, .F. ) ;
#18141 = CIRCLE ( 'NONE', #45828, 125.0000000000000000 ) ;
#18142 = DIRECTION ( 'NONE',  ( -0.000000000000000000, 1.000000000000000000, -0.000000000000000000 ) ) ;
#18145 = ORIENTED_EDGE ( 'NONE', *, *, #45214, .T. ) ;
#18144 = DIRECTION ( 'NONE',  ( 0.000000000000000000, 0.000000000000000000, 1.000000000000000000 ) ) ;
#18143 = CARTESIAN_POINT ( 'NONE',  ( -118.1688136093591908, -189.7472609257535510, -103.7706487676296803 ) ) ;
#18146 = ORIENTED_EDGE ( 'NONE', *, *, #17351, .T. ) ;
#18147 = LINE ( 'NONE', #6833, #18977 ) ;
#18148 = ORIENTED_EDGE ( 'NONE', *, *, #34041, .F. ) ;
#18149 = DIRECTION ( 'NONE',  ( -0.4566292373937200777, 0.000000000000000000, 0.8896570909947436601 ) ) ;
#18150 = FACE_OUTER_BOUND ( 'NONE', #40949, .T. ) ;
#18151 = EDGE_LOOP ( 'NONE', ( #2403, #3405, #6895, #3758 ) ) ;
#18152 = CIRCLE ( 'NONE', #41653, 125.0000000000000000 ) ;
#18153 = EDGE_CURVE ( 'NONE', #42349, #42007, #42150, .T. ) ;
#18154 = DIRECTION ( 'NONE',  ( 0.000000000000000000, 0.000000000000000000, 1.000000000000000000 ) ) ;
#18155 = DIRECTION ( 'NONE',  ( 5.399917434947259359E-17, 1.000000000000000000, -0.000000000000000000 ) ) ;
#18156 = DIRECTION ( 'NONE',  ( -1.000000000000000000, 0.000000000000000000, -0.000000000000000000 ) ) ;
#18157 = PLANE ( 'NONE',  #20127 ) ;
#18158 = VECTOR ( 'NONE', #11685, 999.9999999999998863 ) ;
#18159 = CARTESIAN_POINT ( 'NONE',  ( -23.25236516653334107, -193.5000000000000000, -121.4073237908566512 ) ) ;
#18160 = VERTEX_POINT ( 'NONE', #18511 ) ;
#18161 = VECTOR ( 'NONE', #8969, 1000.000000000000000 ) ;
#18163 = ADVANCED_FACE ( 'NONE', ( #34282 ), #25875, .F. ) ;
#18162 = DIRECTION ( 'NONE',  ( -1.000000000000000000, -1.036104688092335575E-14, 1.258058860540570666E-15 ) ) ;
#18164 = CARTESIAN_POINT ( 'NONE',  ( 27.50603775690333563, -193.5000000000000000, -99.25348746834811209 ) ) ;
#18165 = VECTOR ( 'NONE', #20584, 1000.000000000000000 ) ;
#18166 = LINE ( 'NONE', #42587, #8660 ) ;
#18167 = ORIENTED_EDGE ( 'NONE', *, *, #26595, .T. ) ;
#18168 = DIRECTION ( 'NONE',  ( -0.000000000000000000, 1.000000000000000000, -0.000000000000000000 ) ) ;
#18169 = DIRECTION ( 'NONE',  ( 0.000000000000000000, 1.000000000000000000, -0.000000000000000000 ) ) ;
#18170 = CARTESIAN_POINT ( 'NONE',  ( -4.525132525065792777, -189.7472609257535510, 115.9484881370938325 ) ) ;
#18171 = CARTESIAN_POINT ( 'NONE',  ( -336.3521761649654422, -119.0014323656137947, -58.88711093124865670 ) ) ;
#18172 = AXIS2_PLACEMENT_3D ( 'NONE', #36710, #9375, #48806 ) ;
#18173 = AXIS2_PLACEMENT_3D ( 'NONE', #51978, #48550, #12525 ) ;
#18174 = CYLINDRICAL_SURFACE ( 'NONE', #37082, 125.0000000000000000 ) ;
#18175 = DIRECTION ( 'NONE',  ( -0.2920567706369628924, 0.000000000000000000, -0.9564009842765264224 ) ) ;
#18176 = CARTESIAN_POINT ( 'NONE',  ( -339.1964088526558498, -138.1050951016783301, 57.16590939599346655 ) ) ;
#18177 = AXIS2_PLACEMENT_3D ( 'NONE', #18674, #15245, #22091 ) ;
#18178 = VERTEX_POINT ( 'NONE', #50063 ) ;
#18179 = ADVANCED_FACE ( 'NONE', ( #29809 ), #30855, .T. ) ;
#18180 = ADVANCED_FACE ( 'NONE', ( #14062 ), #5921, .T. ) ;
#18181 = CARTESIAN_POINT ( 'NONE',  ( 0.2952580729112282976, 50.59471834446340210, -21.36672353920345202 ) ) ;
#18182 = DIRECTION ( 'NONE',  ( 0.9266896074318317078, 0.000000000000000000, 0.3758275821142421647 ) ) ;
#18184 = EDGE_LOOP ( 'NONE', ( #17987, #43629, #2658, #27472 ) ) ;
#18183 = DIRECTION ( 'NONE',  ( 1.000000000000000000, 0.000000000000000000, 0.000000000000000000 ) ) ;
#18185 = VECTOR ( 'NONE', #51378, 1000.000000000000000 ) ;
#18186 = VERTEX_POINT ( 'NONE', #10881 ) ;
#18187 = ORIENTED_EDGE ( 'NONE', *, *, #20419, .F. ) ;
#18188 = CARTESIAN_POINT ( 'NONE',  ( 60.19403481868998540, -175.3837268820161057, -59.71720175837096178 ) ) ;
#18189 = CIRCLE ( 'NONE', #50909, 125.0000000000000000 ) ;
#18190 = VECTOR ( 'NONE', #14936, 1000.000000000000114 ) ;
#18191 = EDGE_CURVE ( 'NONE', #42079, #34284, #42418, .T. ) ;
#18193 = AXIS2_PLACEMENT_3D ( 'NONE', #46636, #10621, #27928 ) ;
#18192 = FACE_OUTER_BOUND ( 'NONE', #115, .T. ) ;
#18194 = DIRECTION ( 'NONE',  ( -0.000000000000000000, 1.000000000000000000, -0.000000000000000000 ) ) ;
#18195 = ORIENTED_EDGE ( 'NONE', *, *, #38838, .F. ) ;
#18196 = ADVANCED_FACE ( 'NONE', ( #49805 ), #37707, .F. ) ;
#18197 = VECTOR ( 'NONE', #33188, 1000.000000000000000 ) ;
#18198 = DIRECTION ( 'NONE',  ( 0.000000000000000000, 0.000000000000000000, 1.000000000000000000 ) ) ;
#18199 = CARTESIAN_POINT ( 'NONE',  ( 46.00000000000000711, 33.00000000000000000, -37.00000000000000000 ) ) ;
#18202 = EDGE_LOOP ( 'NONE', ( #718, #14248, #23594, #22272 ) ) ;
#18201 = CARTESIAN_POINT ( 'NONE',  ( -84.53143451966460020, -189.7472609257535510, -118.6432945265037091 ) ) ;
#18200 = CARTESIAN_POINT ( 'NONE',  ( -332.3517673607765914, -159.1821513111375452, -47.06073758877369073 ) ) ;
#18203 = ADVANCED_FACE ( 'NONE', ( #2726 ), #14575, .F. ) ;
#18204 = CARTESIAN_POINT ( 'NONE',  ( -330.4913330509368166, -180.6659093959932250, 14.60509510167933556 ) ) ;
#18205 = ORIENTED_EDGE ( 'NONE', *, *, #28860, .F. ) ;
#18206 = CARTESIAN_POINT ( 'NONE',  ( 38.48673058372652633, -175.3837268820161057, 88.39086586114804334 ) ) ;
#18207 = EDGE_CURVE ( 'NONE', #25337, #46929, #40833, .T. ) ;
#18208 = ORIENTED_EDGE ( 'NONE', *, *, #13394, .F. ) ;
#18209 = DIRECTION ( 'NONE',  ( 0.000000000000000000, 0.000000000000000000, 1.000000000000000000 ) ) ;
#18210 = DIRECTION ( 'NONE',  ( -0.7378332790417333475, 0.000000000000000000, 0.6749830015182038956 ) ) ;
#18211 = DIRECTION ( 'NONE',  ( 0.000000000000000000, 0.8854560256532044704, -0.4647231720437789981 ) ) ;
#18212 = AXIS2_PLACEMENT_3D ( 'NONE', #50874, #50611, #14881 ) ;
#18213 = VERTEX_POINT ( 'NONE', #38210 ) ;
#18214 = CARTESIAN_POINT ( 'NONE',  ( -305.0000000000000568, -176.3931552210903249, -28.32515014536811648 ) ) ;
#18215 = CIRCLE ( 'NONE', #34148, 125.0000000000000000 ) ;
#18216 = DIRECTION ( 'NONE',  ( -1.000000000000000000, 0.000000000000000000, -0.000000000000000000 ) ) ;
#18217 = ORIENTED_EDGE ( 'NONE', *, *, #37892, .T. ) ;
#18218 = CARTESIAN_POINT ( 'NONE',  ( -48.47912675150885065, -183.6283474603465606, 6.938893903907228378E-15 ) ) ;
#18219 = VECTOR ( 'NONE', #42141, 1000.000000000000000 ) ;
#18220 = ORIENTED_EDGE ( 'NONE', *, *, #10944, .F. ) ;
#18221 = FACE_BOUND ( 'NONE', #27162, .T. ) ;
#18222 = DIRECTION ( 'NONE',  ( 1.000000000000000000, -0.000000000000000000, -0.000000000000000000 ) ) ;
#18223 = ORIENTED_EDGE ( 'NONE', *, *, #31698, .T. ) ;
#18224 = CARTESIAN_POINT ( 'NONE',  ( -137.2261550162226911, -193.5000000000000000, 86.60307583628420502 ) ) ;
#18225 = ORIENTED_EDGE ( 'NONE', *, *, #3459, .F. ) ;
#18226 = VECTOR ( 'NONE', #11966, 1000.000000000000114 ) ;
#18227 = CARTESIAN_POINT ( 'NONE',  ( -48.77118352214583297, -193.5000000000000000, 0.9564009842765270886 ) ) ;
#18228 = CIRCLE ( 'NONE', #24939, 60.00000000000000000 ) ;
#18229 = CARTESIAN_POINT ( 'NONE',  ( -339.1964088526558498, -162.9984922102920848, 43.83057281297495678 ) ) ;
#18230 = VERTEX_POINT ( 'NONE', #6437 ) ;
#18231 = CONICAL_SURFACE ( 'NONE', #43395, 4.000000000000003553, 0.7853981633974479459 ) ;
#18232 = VECTOR ( 'NONE', #24746, 1000.000000000000000 ) ;
#18233 = DIRECTION ( 'NONE',  ( -0.000000000000000000, 0.8854560256532043594, -0.4647231720437789981 ) ) ;
#18234 = DIRECTION ( 'NONE',  ( -0.1476465640024779702, 0.000000000000000000, -0.9890401873221644768 ) ) ;
#18235 = CARTESIAN_POINT ( 'NONE',  ( 72.05536924052412928, -175.3837268820161057, 33.11246405730899056 ) ) ;
#18236 = VERTEX_POINT ( 'NONE', #22464 ) ;
#18238 = CIRCLE ( 'NONE', #47610, 60.00000000000000000 ) ;
#18237 = FACE_OUTER_BOUND ( 'NONE', #18558, .T. ) ;
#18239 = VERTEX_POINT ( 'NONE', #34523 ) ;
#18240 = EDGE_CURVE ( 'NONE', #20222, #37538, #50572, .T. ) ;
#18241 = DIRECTION ( 'NONE',  ( -0.000000000000000000, 1.000000000000000000, -0.000000000000000000 ) ) ;
#18242 = CARTESIAN_POINT ( 'NONE',  ( -63.09433862318517328, -193.5000000000000000, -124.1426420773539405 ) ) ;
#18244 = EDGE_LOOP ( 'NONE', ( #4804, #50055, #24012, #46903 ) ) ;
#18243 = CARTESIAN_POINT ( 'NONE',  ( 64.72501964220592185, -189.7472609257535510, 53.00774697410174952 ) ) ;
#18245 = ADVANCED_FACE ( 'NONE', ( #42684 ), #30578, .T. ) ;
#18246 = ORIENTED_EDGE ( 'NONE', *, *, #35255, .F. ) ;
#18247 = EDGE_CURVE ( 'NONE', #4695, #16186, #47917, .T. ) ;
#18248 = EDGE_CURVE ( 'NONE', #47058, #22690, #6936, .T. ) ;
#18249 = DIRECTION ( 'NONE',  ( 0.000000000000000000, 0.000000000000000000, -1.000000000000000000 ) ) ;
#18250 = EDGE_CURVE ( 'NONE', #10838, #17726, #23487, .T. ) ;
#18251 = FACE_OUTER_BOUND ( 'NONE', #16811, .T. ) ;
#18252 = CIRCLE ( 'NONE', #30803, 125.0000000000000000 ) ;
#18253 = ORIENTED_EDGE ( 'NONE', *, *, #44940, .T. ) ;
#18254 = DIRECTION ( 'NONE',  ( -0.000000000000000000, 1.000000000000000000, -0.000000000000000000 ) ) ;
#18255 = EDGE_CURVE ( 'NONE', #23736, #32626, #43960, .T. ) ;
#18256 = ORIENTED_EDGE ( 'NONE', *, *, #4731, .F. ) ;
#18257 = LINE ( 'NONE', #34278, #4003 ) ;
#18258 = CARTESIAN_POINT ( 'NONE',  ( -54.99637373343401237, -175.3837268820161057, 123.8286356280830773 ) ) ;
#18259 = CIRCLE ( 'NONE', #3123, 125.0000000000000000 ) ;
#18260 = EDGE_CURVE ( 'NONE', #22800, #27646, #47671, .T. ) ;
#18261 = CARTESIAN_POINT ( 'NONE',  ( -339.1964088526558498, -64.99044476834248485, -7.608018572113150135 ) ) ;
#18262 = CARTESIAN_POINT ( 'NONE',  ( -41.90263914168912152, -193.5000000000000000, -124.8268793598473536 ) ) ;
#18263 = ORIENTED_EDGE ( 'NONE', *, *, #38521, .F. ) ;
#18264 = VERTEX_POINT ( 'NONE', #40008 ) ;
#18265 = ADVANCED_FACE ( 'NONE', ( #43186 ), #31102, .F. ) ;
#18266 = VERTEX_POINT ( 'NONE', #22968 ) ;
#18267 = CARTESIAN_POINT ( 'NONE',  ( -305.0000000000000568, -179.7763290203208726, -20.80804632820190392 ) ) ;
#18268 = CARTESIAN_POINT ( 'NONE',  ( -51.83230197877470147, -183.6283474603465606, 123.9551692589637639 ) ) ;
#18269 = VECTOR ( 'NONE', #34782, 1000.000000000000000 ) ;
#18270 = EDGE_CURVE ( 'NONE', #16896, #18800, #35301, .T. ) ;
#18271 = VECTOR ( 'NONE', #22397, 1000.000000000000000 ) ;
#18272 = AXIS2_PLACEMENT_3D ( 'NONE', #16984, #25381, #45367 ) ;
#18273 = LINE ( 'NONE', #25882, #46349 ) ;
#18274 = CARTESIAN_POINT ( 'NONE',  ( -336.3521761649654422, -85.59754891220836726, -45.24454186338619621 ) ) ;
#18275 = ORIENTED_EDGE ( 'NONE', *, *, #1857, .T. ) ;
#18276 = ADVANCED_FACE ( 'NONE', ( #11653 ), #11894, .T. ) ;
#18277 = CIRCLE ( 'NONE', #47650, 125.0000000000000000 ) ;
#18278 = LINE ( 'NONE', #994, #23188 ) ;
#18279 = EDGE_CURVE ( 'NONE', #4817, #28748, #42929, .T. ) ;
#18280 = VERTEX_POINT ( 'NONE', #35820 ) ;
#18281 = EDGE_LOOP ( 'NONE', ( #5528, #5645, #48580, #12805 ) ) ;
#18282 = DIRECTION ( 'NONE',  ( 1.000000000000000000, -0.000000000000000000, -0.000000000000000000 ) ) ;
#18283 = CYLINDRICAL_SURFACE ( 'NONE', #12275, 4.999999999999997335 ) ;
#18284 = CARTESIAN_POINT ( 'NONE',  ( -330.4913330509368166, -96.52406086224436876, -52.47426709956133806 ) ) ;
#18285 = LINE ( 'NONE', #1471, #24264 ) ;
#18286 = VERTEX_POINT ( 'NONE', #39498 ) ;
#18287 = CARTESIAN_POINT ( 'NONE',  ( -336.3521761649653854, -152.8183901354257159, -52.34913561719022113 ) ) ;
#18288 = ORIENTED_EDGE ( 'NONE', *, *, #26613, .T. ) ;
#18289 = EDGE_CURVE ( 'NONE', #1436, #15388, #11380, .T. ) ;
#18290 = ORIENTED_EDGE ( 'NONE', *, *, #23464, .T. ) ;
#18291 = CARTESIAN_POINT ( 'NONE',  ( -339.1964088526558498, -108.8949048983213004, -57.16590939599337418 ) ) ;
#18292 = AXIS2_PLACEMENT_3D ( 'NONE', #1917, #17956, #41865 ) ;
#18293 = VECTOR ( 'NONE', #36225, 1000.000000000000000 ) ;
#18294 = CARTESIAN_POINT ( 'NONE',  ( -48.07600332222088468, -177.1207230881787780, 0.9151456172430280089 ) ) ;
#18295 = ORIENTED_EDGE ( 'NONE', *, *, #6677, .F. ) ;
#18296 = CIRCLE ( 'NONE', #28361, 125.0000000000000000 ) ;
#18297 = DIRECTION ( 'NONE',  ( 0.7378332790417239107, 0.000000000000000000, 0.6749830015182142207 ) ) ;
#18298 = FACE_BOUND ( 'NONE', #25541, .T. ) ;
#18299 = CARTESIAN_POINT ( 'NONE',  ( -78.41101675714241992, -189.7472609257535510, -120.3332351033023286 ) ) ;
#18300 = CARTESIAN_POINT ( 'NONE',  ( 21.21056010634070432, -189.7472609257535510, 103.7706487676302061 ) ) ;
#18301 = PLANE ( 'NONE',  #23603 ) ;
#18302 = EDGE_CURVE ( 'NONE', #26407, #46129, #51113, .T. ) ;
#18303 = EDGE_LOOP ( 'NONE', ( #4852, #9195, #50509, #47940 ) ) ;
#18304 = AXIS2_PLACEMENT_3D ( 'NONE', #667, #45346, #44808 ) ;
#18305 = FACE_OUTER_BOUND ( 'NONE', #3550, .T. ) ;
#18306 = VERTEX_POINT ( 'NONE', #51874 ) ;
#18307 = EDGE_CURVE ( 'NONE', #8754, #10566, #47608, .T. ) ;
#18308 = ORIENTED_EDGE ( 'NONE', *, *, #37175, .T. ) ;
#18309 = EDGE_CURVE ( 'NONE', #5120, #19493, #15869, .T. ) ;
#18310 = PLANE ( 'NONE',  #33011 ) ;
#18311 = ADVANCED_FACE ( 'NONE', ( #3261 ), #15100, .T. ) ;
#18312 = ORIENTED_EDGE ( 'NONE', *, *, #16647, .T. ) ;
#18313 = EDGE_CURVE ( 'NONE', #27750, #4, #23235, .T. ) ;
#18314 = AXIS2_PLACEMENT_3D ( 'NONE', #282, #16857, #32613 ) ;
#18315 = DIRECTION ( 'NONE',  ( -0.000000000000000000, -0.000000000000000000, 1.000000000000000000 ) ) ;
#18316 = FACE_OUTER_BOUND ( 'NONE', #19426, .T. ) ;
#18317 = LINE ( 'NONE', #14623, #33826 ) ;
#18318 = VERTEX_POINT ( 'NONE', #47400 ) ;
#18319 = PLANE ( 'NONE',  #42555 ) ;
#18320 = DIRECTION ( 'NONE',  ( -0.3482016354344059095, 0.000000000000000000, 0.9374196611341183427 ) ) ;
#18321 = DIRECTION ( 'NONE',  ( 0.000000000000000000, 0.000000000000000000, 1.000000000000000000 ) ) ;
#18322 = VERTEX_POINT ( 'NONE', #51599 ) ;
#18323 = ORIENTED_EDGE ( 'NONE', *, *, #48386, .F. ) ;
#18324 = ORIENTED_EDGE ( 'NONE', *, *, #14585, .F. ) ;
#18325 = DIRECTION ( 'NONE',  ( 0.000000000000000000, -0.5680647467311485954, 0.8229838658936613482 ) ) ;
#18326 =( GEOMETRIC_REPRESENTATION_CONTEXT ( 3 ) GLOBAL_UNCERTAINTY_ASSIGNED_CONTEXT ( ( #47410 ) ) GLOBAL_UNIT_ASSIGNED_CONTEXT ( ( #36292, #4510, #27641 ) ) REPRESENTATION_CONTEXT ( 'NONE', 'WORKASPACE' ) );
#18327 = CARTESIAN_POINT ( 'NONE',  ( 52.98246549829695340, -175.3837268820161057, 73.01058346660533971 ) ) ;
#18328 = AXIS2_PLACEMENT_3D ( 'NONE', #48003, #20934, #12517 ) ;
#18329 = EDGE_CURVE ( 'NONE', #903, #29300, #2989, .T. ) ;
#18330 = AXIS2_PLACEMENT_3D ( 'NONE', #523, #36023, #40213 ) ;
#18331 = SURFACE_STYLE_FILL_AREA ( #38276 ) ;
#18332 = CARTESIAN_POINT ( 'NONE',  ( 66.49421114223471818, -189.7472609257535510, -46.44493303993017719 ) ) ;
#18333 = PLANE ( 'NONE',  #23023 ) ;
#18334 = ORIENTED_EDGE ( 'NONE', *, *, #21872, .T. ) ;
#18335 = AXIS2_PLACEMENT_3D ( 'NONE', #2421, #18448, #10049 ) ;
#18336 = ADVANCED_FACE ( 'NONE', ( #19029 ), #7464, .F. ) ;
#18337 = ADVANCED_FACE ( 'NONE', ( #28957 ), #9014, .T. ) ;
#18338 = PLANE ( 'NONE',  #41645 ) ;
#18339 = ORIENTED_EDGE ( 'NONE', *, *, #25885, .F. ) ;
#18341 = ORIENTED_EDGE ( 'NONE', *, *, #3686, .T. ) ;
#18340 = CARTESIAN_POINT ( 'NONE',  ( -365.0000000000001137, -78.50000000000002842, -5.000000000000001776 ) ) ;
#18342 = VECTOR ( 'NONE', #47142, 1000.000000000000000 ) ;
#18343 = EDGE_LOOP ( 'NONE', ( #12895, #47356 ) ) ;
#18344 = PLANE ( 'NONE',  #33366 ) ;
#18345 = ORIENTED_EDGE ( 'NONE', *, *, #29205, .F. ) ;
#18346 = CARTESIAN_POINT ( 'NONE',  ( 64.72501964220592185, -193.5000000000000000, 53.00774697410174952 ) ) ;
#18347 = ORIENTED_EDGE ( 'NONE', *, *, #45690, .T. ) ;
#18348 = CARTESIAN_POINT ( 'NONE',  ( 71.44208735029286572, -183.6283474603465606, 35.26900067126700833 ) ) ;
#18349 = LINE ( 'NONE', #45685, #47762 ) ;
#18350 = ORIENTED_EDGE ( 'NONE', *, *, #19340, .F. ) ;
#18351 = DIRECTION ( 'NONE',  ( -1.000000000000000000, -0.000000000000000000, -0.000000000000000000 ) ) ;
#18352 = ORIENTED_EDGE ( 'NONE', *, *, #13172, .T. ) ;
#18353 = VECTOR ( 'NONE', #35440, 1000.000000000000000 ) ;
#18354 = ORIENTED_EDGE ( 'NONE', *, *, #35155, .F. ) ;
#18355 = CARTESIAN_POINT ( 'NONE',  ( -119.6907301311197216, -183.6283474603465606, 101.5140743725400370 ) ) ;
#18356 = CARTESIAN_POINT ( 'NONE',  ( -339.1964088526558498, -123.5000000000000284, 0.000000000000000000 ) ) ;
#18357 = EDGE_LOOP ( 'NONE', ( #38942, #37998, #37791, #15185 ) ) ;
#18358 = CARTESIAN_POINT ( 'NONE',  ( -162.7543581613524282, -177.1207230881787780, 50.65739320402011003 ) ) ;
#18359 = LINE ( 'NONE', #14664, #32298 ) ;
#18360 = DIRECTION ( 'NONE',  ( 0.000000000000000000, 0.9709418174260553425, 0.2393156642875449158 ) ) ;
#18361 = CARTESIAN_POINT ( 'NONE',  ( -118.1688136093591908, -189.7472609257535510, -103.7706487676296803 ) ) ;
#18362 = ORIENTED_EDGE ( 'NONE', *, *, #8409, .F. ) ;
#18363 = CARTESIAN_POINT ( 'NONE',  ( -332.3517673607765914, -87.81784868886214213, 47.06073758877343494 ) ) ;
#18364 = DIRECTION ( 'NONE',  ( 0.000000000000000000, 0.000000000000000000, 1.000000000000000000 ) ) ;
#18365 = CARTESIAN_POINT ( 'NONE',  ( -336.3521761649654422, -105.0395444947681369, -56.09938080879045685 ) ) ;
#18366 = AXIS2_PLACEMENT_3D ( 'NONE', #23393, #39401, #31520 ) ;
#18367 = ORIENTED_EDGE ( 'NONE', *, *, #44895, .T. ) ;
#18368 = VECTOR ( 'NONE', #2503, 1000.000000000000000 ) ;
#18369 = VECTOR ( 'NONE', #47802, 1000.000000000000227 ) ;
#18370 = CYLINDRICAL_SURFACE ( 'NONE', #49920, 125.0000000000000000 ) ;
#18371 = VECTOR ( 'NONE', #28576, 1000.000000000000000 ) ;
#18372 = CARTESIAN_POINT ( 'NONE',  ( 56.77503207194101265, -189.7472609257535510, -67.42819922234311036 ) ) ;
#18373 = ORIENTED_EDGE ( 'NONE', *, *, #22119, .T. ) ;
#18374 = EDGE_CURVE ( 'NONE', #27011, #30763, #39186, .T. ) ;
#18375 = EDGE_CURVE ( 'NONE', #7178, #49884, #5678, .T. ) ;
#18376 = CARTESIAN_POINT ( 'NONE',  ( 0.000000000000000000, -150.9186671505818822, 52.24190551353965617 ) ) ;
#18377 = ORIENTED_EDGE ( 'NONE', *, *, #243, .T. ) ;
#18378 = VECTOR ( 'NONE', #19655, 1000.000000000000114 ) ;
#18379 = FACE_OUTER_BOUND ( 'NONE', #7065, .T. ) ;
#18380 = CARTESIAN_POINT ( 'NONE',  ( -336.3521761649654422, -121.8677111499054320, 59.00000000000001421 ) ) ;
#18381 = DIRECTION ( 'NONE',  ( 0.000000000000000000, 1.000000000000000000, 0.000000000000000000 ) ) ;
#18382 = LINE ( 'NONE', #34401, #20763 ) ;
#18383 = DIRECTION ( 'NONE',  ( 0.000000000000000000, 0.000000000000000000, 1.000000000000000000 ) ) ;
#18384 = ORIENTED_EDGE ( 'NONE', *, *, #11574, .F. ) ;
#18385 = VECTOR ( 'NONE', #11733, 1000.000000000000000 ) ;
#18386 = LINE ( 'NONE', #33877, #42447 ) ;
#18387 = EDGE_LOOP ( 'NONE', ( #51488, #47883 ) ) ;
#18388 = CARTESIAN_POINT ( 'NONE',  ( -48.24424070572787571, -189.7472609257535510, 0.9720229140804191870 ) ) ;
#18389 = VERTEX_POINT ( 'NONE', #20839 ) ;
#18390 = ADVANCED_FACE ( 'NONE', ( #36865 ), #33171, .T. ) ;
#18391 = CARTESIAN_POINT ( 'NONE',  ( 46.00000000000000711, 20.00000000000000000, -41.00000000000000000 ) ) ;
#18392 = EDGE_CURVE ( 'NONE', #48065, #27409, #12146, .T. ) ;
#18393 = CARTESIAN_POINT ( 'NONE',  ( -25.55153130240594450, -193.5000000000000000, 122.8793122007210599 ) ) ;
#18394 = FACE_OUTER_BOUND ( 'NONE', #6387, .T. ) ;
#18395 = ORIENTED_EDGE ( 'NONE', *, *, #41373, .F. ) ;
#18398 = ORIENTED_EDGE ( 'NONE', *, *, #6416, .F. ) ;
#18397 = CARTESIAN_POINT ( 'NONE',  ( -49.44376233341720450, -193.5000000000000000, -0.2635871660690713436 ) ) ;
#18396 = CARTESIAN_POINT ( 'NONE',  ( -2.241711803726597285, 51.04610933365329828, -20.95518423169113831 ) ) ;
#18399 = AXIS2_PLACEMENT_3D ( 'NONE', #45990, #9981, #13393 ) ;
#18400 = DIRECTION ( 'NONE',  ( -0.5338233779648003940, 0.000000000000000000, 0.8455960035018199594 ) ) ;
#18401 = ORIENTED_EDGE ( 'NONE', *, *, #15929, .F. ) ;
#18402 = DIRECTION ( 'NONE',  ( 0.000000000000000000, 0.000000000000000000, -1.000000000000000000 ) ) ;
#18403 = AXIS2_PLACEMENT_3D ( 'NONE', #30144, #33821, #22534 ) ;
#18404 = ORIENTED_EDGE ( 'NONE', *, *, #16347, .F. ) ;
#18405 = DIRECTION ( 'NONE',  ( -0.000000000000000000, 1.000000000000000000, -0.000000000000000000 ) ) ;
#18408 = ORIENTED_EDGE ( 'NONE', *, *, #8991, .F. ) ;
#18407 = DIRECTION ( 'NONE',  ( 0.000000000000000000, 1.000000000000000000, 0.000000000000000000 ) ) ;
#18406 = CARTESIAN_POINT ( 'NONE',  ( -49.40581635894069024, -183.6283474603465606, 0.3758275821142362250 ) ) ;
#18409 = ORIENTED_EDGE ( 'NONE', *, *, #36563, .T. ) ;
#18410 = VECTOR ( 'NONE', #6221, 1000.000000000000000 ) ;
#18411 = CARTESIAN_POINT ( 'NONE',  ( -62.43888699632653072, -189.7472609257535510, 124.2180546213279229 ) ) ;
#18412 = ORIENTED_EDGE ( 'NONE', *, *, #6092, .T. ) ;
#18413 = CYLINDRICAL_SURFACE ( 'NONE', #11071, 125.0000000000000000 ) ;
#18414 = DIRECTION ( 'NONE',  ( 0.000000000000000000, 0.000000000000000000, 1.000000000000000000 ) ) ;
#18415 = EDGE_LOOP ( 'NONE', ( #16225, #32279, #32621, #8112 ) ) ;
#18416 = DIRECTION ( 'NONE',  ( 0.000000000000000000, 0.5680647467311596976, 0.8229838658936536877 ) ) ;
#18417 = LINE ( 'NONE', #50228, #6539 ) ;
#18418 = LINE ( 'NONE', #46283, #14863 ) ;
#18419 = CARTESIAN_POINT ( 'NONE',  ( -48.47912675150885065, -189.7472609257535510, 6.938893903907228378E-15 ) ) ;
#18420 = LINE ( 'NONE', #46532, #46730 ) ;
#18421 = EDGE_LOOP ( 'NONE', ( #15056, #10855, #1265, #51220 ) ) ;
#18422 = DIRECTION ( 'NONE',  ( -1.000000000000000000, 0.000000000000000000, 0.000000000000000000 ) ) ;
#18423 = DIRECTION ( 'NONE',  ( -1.000000000000000000, -0.000000000000000000, 0.000000000000000000 ) ) ;
#18424 = CIRCLE ( 'NONE', #43580, 125.0000000000000000 ) ;
#18425 = EDGE_CURVE ( 'NONE', #50508, #21465, #51809, .T. ) ;
#18426 = DIRECTION ( 'NONE',  ( 0.000000000000000000, -1.000000000000000000, 0.000000000000000000 ) ) ;
#18427 = EDGE_LOOP ( 'NONE', ( #43202, #6486, #20449, #20374 ) ) ;
#18428 = LINE ( 'NONE', #51266, #26492 ) ;
#18429 = DIRECTION ( 'NONE',  ( 0.000000000000000000, 0.000000000000000000, 1.000000000000000000 ) ) ;
#18430 = DIRECTION ( 'NONE',  ( 0.8294056854502049880, 0.000000000000000000, -0.5586467658036476935 ) ) ;
#18431 = DIRECTION ( 'NONE',  ( 0.6068001458185945385, 0.000000000000000000, -0.7948544414133523750 ) ) ;
#18432 = EDGE_CURVE ( 'NONE', #22639, #7756, #16899, .T. ) ;
#18433 = VERTEX_POINT ( 'NONE', #17156 ) ;
#18434 = FACE_OUTER_BOUND ( 'NONE', #17390, .T. ) ;
#18435 = ADVANCED_FACE ( 'NONE', ( #24260 ), #44748, .F. ) ;
#18436 = AXIS2_PLACEMENT_3D ( 'NONE', #5963, #14114, #46173 ) ;
#18437 = LINE ( 'NONE', #34452, #3502 ) ;
#18438 = DIRECTION ( 'NONE',  ( 0.000000000000000000, 1.000000000000000000, -0.000000000000000000 ) ) ;
#18439 = CARTESIAN_POINT ( 'NONE',  ( -305.0000000000000568, -173.7880015656344312, -32.72792230702632565 ) ) ;
#18440 = AXIS2_PLACEMENT_3D ( 'NONE', #26327, #11315, #27352 ) ;
#18441 = ORIENTED_EDGE ( 'NONE', *, *, #26005, .F. ) ;
#18442 = CARTESIAN_POINT ( 'NONE',  ( -48.47912675150885065, -189.7472609257535510, 6.938893903907228378E-15 ) ) ;
#18443 = CARTESIAN_POINT ( 'NONE',  ( 76.46082103836691601, -189.7472609257535510, 3.874202661595774533 ) ) ;
#18444 = ORIENTED_EDGE ( 'NONE', *, *, #32478, .T. ) ;
#18445 = EDGE_LOOP ( 'NONE', ( #26535, #13929, #12875, #13535 ) ) ;
#18446 = EDGE_LOOP ( 'NONE', ( #32893, #28570, #15431, #23420 ) ) ;
#18447 = EDGE_CURVE ( 'NONE', #9912, #9410, #29965, .T. ) ;
#18448 = DIRECTION ( 'NONE',  ( -0.4827922027307427477, 0.000000000000000000, -0.8757349421956379665 ) ) ;
#18449 = CARTESIAN_POINT ( 'NONE',  ( -47.92047998570519951, -193.5000000000000000, -0.8294056854501942189 ) ) ;
#18450 = DIRECTION ( 'NONE',  ( -0.000000000000000000, 1.000000000000000000, -0.000000000000000000 ) ) ;
#18451 = ORIENTED_EDGE ( 'NONE', *, *, #24305, .T. ) ;
#18452 = AXIS2_PLACEMENT_3D ( 'NONE', #23806, #4106, #28262 ) ;
#18453 = DIRECTION ( 'NONE',  ( 0.000000000000000000, -0.3546048870425463906, -0.9350162426854107256 ) ) ;
#18454 = CARTESIAN_POINT ( 'NONE',  ( -27.18512803868275540, -189.7472609257535510, -123.1729094355498262 ) ) ;
#18457 = ORIENTED_EDGE ( 'NONE', *, *, #3295, .F. ) ;
#18456 = DIRECTION ( 'NONE',  ( 0.9374196611341183427, 0.000000000000000000, 0.3482016354344059095 ) ) ;
#18455 = DIRECTION ( 'NONE',  ( -0.3202698538628487301, 0.000000000000000000, 0.9473263538541877304 ) ) ;
#18458 = CYLINDRICAL_SURFACE ( 'NONE', #31460, 125.0000000000000000 ) ;
#18459 = ORIENTED_EDGE ( 'NONE', *, *, #30878, .F. ) ;
#18460 = DIRECTION ( 'NONE',  ( 1.000000000000000000, -0.000000000000000000, -0.000000000000000000 ) ) ;
#18461 = VERTEX_POINT ( 'NONE', #41310 ) ;
#18462 = DIRECTION ( 'NONE',  ( 0.000000000000000000, 0.000000000000000000, -1.000000000000000000 ) ) ;
#18463 = DIRECTION ( 'NONE',  ( -0.000000000000000000, 1.000000000000000000, -0.000000000000000000 ) ) ;
#18464 = LINE ( 'NONE', #10834, #14831 ) ;
#18465 = ORIENTED_EDGE ( 'NONE', *, *, #52003, .T. ) ;
#18466 = CARTESIAN_POINT ( 'NONE',  ( -336.3521761649653854, -177.3662605214052519, -26.42775013958059560 ) ) ;
#18468 = AXIS2_PLACEMENT_3D ( 'NONE', #37304, #8936, #29161 ) ;
#18467 = CARTESIAN_POINT ( 'NONE',  ( -330.4913330509368166, -66.33409060400670398, -14.60509510167892522 ) ) ;
#18469 = VERTEX_POINT ( 'NONE', #37113 ) ;
#18470 = CARTESIAN_POINT ( 'NONE',  ( -145.0195698084541505, -193.5000000000000000, 79.40367028273128369 ) ) ;
#18471 = CARTESIAN_POINT ( 'NONE',  ( 116.9235303384055840, -213.5000000000000000, -9.999999999999971578 ) ) ;
#18472 = EDGE_CURVE ( 'NONE', #43321, #43010, #24772, .T. ) ;
#18473 = ORIENTED_EDGE ( 'NONE', *, *, #17935, .F. ) ;
#18474 = LINE ( 'NONE', #15305, #14993 ) ;
#18475 = FACE_OUTER_BOUND ( 'NONE', #49675, .T. ) ;
#18476 = EDGE_CURVE ( 'NONE', #18911, #23451, #50127, .T. ) ;
#18477 = PRODUCT_DEFINITION_SHAPE ( 'NONE', 'NONE',  #52042 ) ;
#18478 = ORIENTED_EDGE ( 'NONE', *, *, #497, .F. ) ;
#18479 = DIRECTION ( 'NONE',  ( 0.000000000000000000, 0.000000000000000000, -1.000000000000000000 ) ) ;
#18480 = ORIENTED_EDGE ( 'NONE', *, *, #40393, .F. ) ;
#18481 = CARTESIAN_POINT ( 'NONE',  ( -340.0000000000000568, -123.5000000000000284, -60.00000000000000000 ) ) ;
#18482 = CYLINDRICAL_SURFACE ( 'NONE', #37832, 20.00000000000001066 ) ;
#18483 = ORIENTED_EDGE ( 'NONE', *, *, #25665, .T. ) ;
#18484 = DIRECTION ( 'NONE',  ( 1.000000000000000000, 7.175085443855111658E-17, 4.952603889764001357E-17 ) ) ;
#18485 = PLANE ( 'NONE',  #47403 ) ;
#18486 = PLANE ( 'NONE',  #8982 ) ;
#18487 = EDGE_CURVE ( 'NONE', #7752, #15492, #34167, .T. ) ;
#18488 = EDGE_CURVE ( 'NONE', #33164, #7438, #29135, .T. ) ;
#18489 = ADVANCED_FACE ( 'NONE', ( #44489 ), #45290, .F. ) ;
#18490 = VECTOR ( 'NONE', #43192, 999.9999999999998863 ) ;
#18491 = ORIENTED_EDGE ( 'NONE', *, *, #37103, .F. ) ;
#18492 = AXIS2_PLACEMENT_3D ( 'NONE', #42072, #18169, #26295 ) ;
#18493 = DIRECTION ( 'NONE',  ( -1.000000000000000000, -0.000000000000000000, 0.000000000000000000 ) ) ;
#18494 = VERTEX_POINT ( 'NONE', #28442 ) ;
#18495 = EDGE_CURVE ( 'NONE', #19422, #48723, #8473, .T. ) ;
#18496 = EDGE_CURVE ( 'NONE', #46003, #22824, #36598, .T. ) ;
#18497 = CARTESIAN_POINT ( 'NONE',  ( -48.93575598890255662, -193.5000000000000000, -0.8896570909947461026 ) ) ;
#18498 = PLANE ( 'NONE',  #29354 ) ;
#18500 = ORIENTED_EDGE ( 'NONE', *, *, #46210, .F. ) ;
#18499 = DIRECTION ( 'NONE',  ( -1.000000000000000000, 0.000000000000000000, 0.000000000000000000 ) ) ;
#18501 = ORIENTED_EDGE ( 'NONE', *, *, #36103, .T. ) ;
#18502 = PLANE ( 'NONE',  #8985 ) ;
#18503 = DIRECTION ( 'NONE',  ( -0.000000000000000000, 1.000000000000000000, -0.000000000000000000 ) ) ;
#18504 = ORIENTED_EDGE ( 'NONE', *, *, #45593, .F. ) ;
#18505 = VECTOR ( 'NONE', #50964, 1000.000000000000000 ) ;
#18506 = CARTESIAN_POINT ( 'NONE',  ( 76.47090317495664635, -193.5000000000000000, -3.534122433557446374 ) ) ;
#18507 = ORIENTED_EDGE ( 'NONE', *, *, #34019, .T. ) ;
#18508 = CARTESIAN_POINT ( 'NONE',  ( -161.4019114581580823, -193.5000000000000000, 53.60452120946281696 ) ) ;
#18509 = DIRECTION ( 'NONE',  ( -0.000000000000000000, 1.000000000000000000, -0.000000000000000000 ) ) ;
#18510 = DIRECTION ( 'NONE',  ( 0.02963332782256331357, 0.000000000000000000, -0.9995608365087942371 ) ) ;
#18511 = CARTESIAN_POINT ( 'NONE',  ( -339.1964088526558498, -131.2283041299240836, 59.50019592636143528 ) ) ;
#18512 = ORIENTED_EDGE ( 'NONE', *, *, #39092, .T. ) ;
#18513 = ORIENTED_EDGE ( 'NONE', *, *, #19285, .T. ) ;
#18514 = VERTEX_POINT ( 'NONE', #48135 ) ;
#18515 = CARTESIAN_POINT ( 'NONE',  ( -48.47912675150885065, -173.5000000000000284, 6.938893903907228378E-15 ) ) ;
#18516 = DIRECTION ( 'NONE',  ( -0.000000000000000000, 1.000000000000000000, -0.000000000000000000 ) ) ;
#18517 = CARTESIAN_POINT ( 'NONE',  ( -365.0000000000001137, -78.50000000000002842, 0.000000000000000000 ) ) ;
#18518 = CARTESIAN_POINT ( 'NONE',  ( 43.63512310656542326, -193.5000000000000000, 84.49831343337136502 ) ) ;
#18519 = VERTEX_POINT ( 'NONE', #12381 ) ;
#18520 = UNCERTAINTY_MEASURE_WITH_UNIT (LENGTH_MEASURE( 1.000000000000000082E-05 ), #27883, 'distance_accuracy_value', 'NONE');
#18521 = CARTESIAN_POINT ( 'NONE',  ( 70.20858612167234014, -177.1207230881787780, 35.90758392117750475 ) ) ;
#18522 = AXIS2_PLACEMENT_3D ( 'NONE', #44691, #4748, #49161 ) ;
#18523 = CIRCLE ( 'NONE', #10150, 125.0000000000000000 ) ;
#18524 = ORIENTED_EDGE ( 'NONE', *, *, #8802, .T. ) ;
#18525 = EDGE_LOOP ( 'NONE', ( #27917, #27959, #39002, #43174 ) ) ;
#18526 = DIRECTION ( 'NONE',  ( -0.2348860457809911206, 0.000000000000000000, 0.9720229140804089729 ) ) ;
#18527 = CARTESIAN_POINT ( 'NONE',  ( 61.06976976088564157, -189.7472609257535510, -60.19999396110169698 ) ) ;
#18528 = MANIFOLD_SOLID_BREP ( 'Chamfer2', #37139 ) ;
#18529 = FACE_OUTER_BOUND ( 'NONE', #3567, .T. ) ;
#18530 = EDGE_CURVE ( 'NONE', #20432, #28789, #41753, .T. ) ;
#18531 = DIRECTION ( 'NONE',  ( -0.000000000000000000, 1.000000000000000000, -0.000000000000000000 ) ) ;
#18532 = EDGE_CURVE ( 'NONE', #35, #50678, #3991, .T. ) ;
#18533 = EDGE_CURVE ( 'NONE', #36997, #48106, #44263, .T. ) ;
#18534 = LINE ( 'NONE', #35328, #11689 ) ;
#18535 = ORIENTED_EDGE ( 'NONE', *, *, #27958, .T. ) ;
#18536 = CARTESIAN_POINT ( 'NONE',  ( -49.47517659412406488, -189.7472609257535510, -0.08879589532293878651 ) ) ;
#18537 = VERTEX_POINT ( 'NONE', #20801 ) ;
#18538 = LINE ( 'NONE', #14341, #45575 ) ;
#18539 = CIRCLE ( 'NONE', #13515, 15.00000000000000000 ) ;
#18540 = DIRECTION ( 'NONE',  ( 1.000000000000000000, -0.000000000000000000, 0.000000000000000000 ) ) ;
#18541 = ORIENTED_EDGE ( 'NONE', *, *, #2462, .F. ) ;
#18542 = EDGE_CURVE ( 'NONE', #33969, #30895, #16081, .T. ) ;
#18543 = DIRECTION ( 'NONE',  ( -1.060575238724906545E-16, 1.000000000000000000, 0.000000000000000000 ) ) ;
#18544 = CYLINDRICAL_SURFACE ( 'NONE', #20459, 125.0000000000000000 ) ;
#18545 = CARTESIAN_POINT ( 'NONE',  ( -1.230335819511603423, -177.1207230881787780, 115.7261930397108216 ) ) ;
#18546 = EDGE_CURVE ( 'NONE', #39327, #21742, #28141, .T. ) ;
#18547 = DIRECTION ( 'NONE',  ( -0.000000000000000000, -0.3546048870425396182, -0.9350162426854132791 ) ) ;
#18548 = EDGE_CURVE ( 'NONE', #7465, #23874, #44190, .T. ) ;
#18549 = DIRECTION ( 'NONE',  ( -0.000000000000000000, -0.9709418174260534551, -0.2393156642875516327 ) ) ;
#18550 = EDGE_LOOP ( 'NONE', ( #441, #47418, #27584, #28933 ) ) ;
#18551 = ADVANCED_FACE ( 'NONE', ( #48400 ), #42563, .T. ) ;
#18552 = LINE ( 'NONE', #23281, #26452 ) ;
#18553 = EDGE_LOOP ( 'NONE', ( #16801, #27351, #15555, #20968 ) ) ;
#18554 = AXIS2_PLACEMENT_3D ( 'NONE', #24363, #3415, #26558 ) ;
#18555 = EDGE_CURVE ( 'NONE', #16914, #12681, #12637, .T. ) ;
#18556 = ORIENTED_EDGE ( 'NONE', *, *, #48887, .T. ) ;
#18557 = CARTESIAN_POINT ( 'NONE',  ( 7.859956736328458149, -189.7472609257535510, -111.5836353223468649 ) ) ;
#18558 = EDGE_LOOP ( 'NONE', ( #26023, #25953, #33240, #42220 ) ) ;
#18559 = VECTOR ( 'NONE', #2466, 1000.000000000000227 ) ;
#18560 = DIRECTION ( 'NONE',  ( 0.000000000000000000, 0.000000000000000000, -1.000000000000000000 ) ) ;
#18561 = ORIENTED_EDGE ( 'NONE', *, *, #43964, .T. ) ;
#18562 = FACE_OUTER_BOUND ( 'NONE', #6648, .T. ) ;
#18563 = DIRECTION ( 'NONE',  ( 0.000000000000000000, 0.4647231720437789981, 0.8854560256532044704 ) ) ;
#18564 = ORIENTED_EDGE ( 'NONE', *, *, #45888, .F. ) ;
#18565 = CARTESIAN_POINT ( 'NONE',  ( -330.4913330509368166, -182.5000000000000568, 0.4999999999999549249 ) ) ;
#18566 = DIRECTION ( 'NONE',  ( -1.000000000000000000, 0.000000000000000000, 0.000000000000000000 ) ) ;
#18567 = DIRECTION ( 'NONE',  ( -0.000000000000000000, 0.8229838658936556861, -0.5680647467311569221 ) ) ;
#18568 = EDGE_CURVE ( 'NONE', #10098, #2552, #1072, .T. ) ;
#18569 = EDGE_LOOP ( 'NONE', ( #45298, #31057, #23613, #38344 ) ) ;
#18570 = ORIENTED_EDGE ( 'NONE', *, *, #843, .F. ) ;
#18571 = VERTEX_POINT ( 'NONE', #8704 ) ;
#18572 = FACE_OUTER_BOUND ( 'NONE', #49505, .T. ) ;
#18573 = DIRECTION ( 'NONE',  ( -0.000000000000000000, 0.4647231720437573488, -0.8854560256532157947 ) ) ;
#18574 = VECTOR ( 'NONE', #42093, 1000.000000000000000 ) ;
#18575 = LINE ( 'NONE', #21747, #15894 ) ;
#18576 = DIRECTION ( 'NONE',  ( 0.000000000000000000, 0.000000000000000000, -1.000000000000000000 ) ) ;
#18577 = PLANE ( 'NONE',  #23879 ) ;
#18578 = ORIENTED_EDGE ( 'NONE', *, *, #38060, .T. ) ;
#18579 = DIRECTION ( 'NONE',  ( -0.000000000000000000, 1.000000000000000000, -0.000000000000000000 ) ) ;
#18580 = ADVANCED_FACE ( 'NONE', ( #28922 ), #36294, .T. ) ;
#18581 = ORIENTED_EDGE ( 'NONE', *, *, #32534, .T. ) ;
#18583 = ORIENTED_EDGE ( 'NONE', *, *, #38464, .F. ) ;
#18582 = DIRECTION ( 'NONE',  ( -0.000000000000000000, 0.1205366802553337752, 0.9927088740980526405 ) ) ;
#18584 = ORIENTED_EDGE ( 'NONE', *, *, #17690, .T. ) ;
#18585 = CARTESIAN_POINT ( 'NONE',  ( 44.46230746252008004, 28.00000000000000355, -46.05672166561993208 ) ) ;
#18586 = ORIENTED_EDGE ( 'NONE', *, *, #42917, .F. ) ;
#18587 = DIRECTION ( 'NONE',  ( 1.000000000000000000, 0.000000000000000000, 0.000000000000000000 ) ) ;
#18588 = VECTOR ( 'NONE', #5706, 1000.000000000000000 ) ;
#18589 = EDGE_CURVE ( 'NONE', #34528, #13215, #36831, .T. ) ;
#18590 = EDGE_CURVE ( 'NONE', #4651, #50992, #16866, .T. ) ;
#18591 = LINE ( 'NONE', #10705, #38068 ) ;
#18592 = ADVANCED_FACE ( 'NONE', ( #44984 ), #21056, .F. ) ;
#18593 = EDGE_CURVE ( 'NONE', #29662, #49548, #18417, .T. ) ;
#18594 = CARTESIAN_POINT ( 'NONE',  ( -339.1964088526558498, -131.2283041299249930, -59.50019592636133581 ) ) ;
#18595 = ORIENTED_EDGE ( 'NONE', *, *, #44573, .T. ) ;
#18596 = DIRECTION ( 'NONE',  ( 0.000000000000000000, 0.000000000000000000, -1.000000000000000000 ) ) ;
#18597 = AXIS2_PLACEMENT_3D ( 'NONE', #42445, #42181, #50352 ) ;
#18598 = ORIENTED_EDGE ( 'NONE', *, *, #18830, .F. ) ;
#18599 = ADVANCED_FACE ( 'NONE', ( #10020 ), #25778, .T. ) ;
#18600 = EDGE_LOOP ( 'NONE', ( #51774, #14617, #47697, #51067 ) ) ;
#18601 = DIRECTION ( 'NONE',  ( 0.9027978299657446470, 0.000000000000000000, -0.4300652022765183435 ) ) ;
#18602 = DIRECTION ( 'NONE',  ( 0.000000000000000000, 1.000000000000000000, 0.000000000000000000 ) ) ;
#18603 = ADVANCED_FACE ( 'NONE', ( #5559 ), #49182, .T. ) ;
#18604 = CARTESIAN_POINT ( 'NONE',  ( -77.03256798524179771, -175.3837268820161057, 121.6951149130964751 ) ) ;
#18605 = VERTEX_POINT ( 'NONE', #13431 ) ;
#18606 = LINE ( 'NONE', #39843, #34917 ) ;
#18607 = DIRECTION ( 'NONE',  ( -1.000000000000000000, 0.000000000000000000, 0.000000000000000000 ) ) ;
#18608 = DIRECTION ( 'NONE',  ( 0.000000000000000000, 0.7485107481711024136, 0.6631226582407937498 ) ) ;
#18609 = DIRECTION ( 'NONE',  ( 0.000000000000000000, 0.8660254037844378194, 0.5000000000000013323 ) ) ;
#18610 = EDGE_CURVE ( 'NONE', #895, #23734, #13243, .T. ) ;
#18611 = ORIENTED_EDGE ( 'NONE', *, *, #40393, .T. ) ;
#18612 = PLANE ( 'NONE',  #22977 ) ;
#18613 = CARTESIAN_POINT ( 'NONE',  ( -172.1341525481709880, -189.7472609257535510, 18.28755301364335750 ) ) ;
#18614 = VECTOR ( 'NONE', #16166, 1000.000000000000000 ) ;
#18615 = ADVANCED_FACE ( 'NONE', ( #2387 ), #10263, .F. ) ;
#18616 = CARTESIAN_POINT ( 'NONE',  ( -166.8403286750647680, -175.3837268820161057, -40.19484891389966918 ) ) ;
#18617 = ORIENTED_EDGE ( 'NONE', *, *, #50811, .T. ) ;
#18618 = VECTOR ( 'NONE', #37252, 1000.000000000000114 ) ;
#18619 = EDGE_CURVE ( 'NONE', #5479, #48164, #9237, .T. ) ;
#18620 = CARTESIAN_POINT ( 'NONE',  ( 64.86941505090324256, -183.6283474603465606, -50.28156562190504530 ) ) ;
#18621 = CARTESIAN_POINT ( 'NONE',  ( -339.1964088526558498, -176.8578783931336602, 27.43969411971573891 ) ) ;
#18622 = ADVANCED_FACE ( 'NONE', ( #42305 ), #29977, .F. ) ;
#18623 = VERTEX_POINT ( 'NONE', #33910 ) ;
#18624 = CARTESIAN_POINT ( 'NONE',  ( -330.4913330509368166, -167.9936954712150339, 38.74998146212178796 ) ) ;
#18625 = EDGE_LOOP ( 'NONE', ( #45454, #50978, #19219, #11618 ) ) ;
#18626 = EDGE_CURVE ( 'NONE', #4562, #50065, #29048, .T. ) ;
#18627 = APPLICATION_CONTEXT ( 'automotive_design' ) ;
#18628 = DIRECTION ( 'NONE',  ( 1.000000000000000000, 0.000000000000000000, 0.000000000000000000 ) ) ;
#18629 = DIRECTION ( 'NONE',  ( 0.000000000000000000, 0.000000000000000000, -1.000000000000000000 ) ) ;
#18630 = CARTESIAN_POINT ( 'NONE',  ( -336.3521761649654422, -174.9833430614318388, 28.86398714850502856 ) ) ;
#18631 = AXIS2_PLACEMENT_3D ( 'NONE', #819, #17122, #28918 ) ;
#18632 = CARTESIAN_POINT ( 'NONE',  ( -46.00000000000000711, 0.000000000000000000, -46.00000000000000000 ) ) ;
#18633 = AXIS2_PLACEMENT_3D ( 'NONE', #49255, #45323, #41345 ) ;
#18634 = DIRECTION ( 'NONE',  ( 0.000000000000000000, 0.000000000000000000, 1.000000000000000000 ) ) ;
#18635 = EDGE_LOOP ( 'NONE', ( #38272, #38514, #38884, #45810 ) ) ;
#18636 = AXIS2_PLACEMENT_3D ( 'NONE', #7935, #19765, #23472 ) ;
#18638 = EDGE_CURVE ( 'NONE', #7509, #51184, #7354, .T. ) ;
#18637 = CARTESIAN_POINT ( 'NONE',  ( 75.27070168362158142, -189.7472609257535510, 17.63462396184792524 ) ) ;
#18639 = ORIENTED_EDGE ( 'NONE', *, *, #27084, .F. ) ;
#18640 = DIRECTION ( 'NONE',  ( 0.9473263538541899509, 0.000000000000000000, 0.3202698538628415692 ) ) ;
#18641 = EDGE_LOOP ( 'NONE', ( #8972, #31436, #17698, #45940 ) ) ;
#18642 = FACE_OUTER_BOUND ( 'NONE', #18947, .T. ) ;
#18643 = VECTOR ( 'NONE', #1361, 1000.000000000000000 ) ;
#18644 = DIRECTION ( 'NONE',  ( 0.000000000000000000, 1.000000000000000000, 0.000000000000000000 ) ) ;
#18645 = CARTESIAN_POINT ( 'NONE',  ( -136.5246168469702468, -177.1207230881787780, 87.31661597576147926 ) ) ;
#18646 = ORIENTED_EDGE ( 'NONE', *, *, #29102, .F. ) ;
#18649 = VERTEX_POINT ( 'NONE', #26033 ) ;
#18648 = CARTESIAN_POINT ( 'NONE',  ( -330.4913330509368166, -167.3305728129743102, 39.49849221029282376 ) ) ;
#18647 = DIRECTION ( 'NONE',  ( 0.000000000000000000, 0.000000000000000000, 1.000000000000000000 ) ) ;
#18650 = VECTOR ( 'NONE', #46225, 1000.000000000000227 ) ;
#18651 = CONICAL_SURFACE ( 'NONE', #48022, 10.00000000000000711, 0.03490658503988659789 ) ;
#18652 = CARTESIAN_POINT ( 'NONE',  ( -305.0000000000000568, -110.7312321683605916, -58.62557946887767457 ) ) ;
#18653 = VERTEX_POINT ( 'NONE', #46030 ) ;
#18654 = CARTESIAN_POINT ( 'NONE',  ( -140.1460956102404509, -193.5000000000000000, 84.98333260264821831 ) ) ;
#18655 = ORIENTED_EDGE ( 'NONE', *, *, #47091, .T. ) ;
#18656 = EDGE_CURVE ( 'NONE', #18469, #4360, #29197, .T. ) ;
#18657 = EDGE_CURVE ( 'NONE', #51239, #34751, #21317, .T. ) ;
#18658 = CARTESIAN_POINT ( 'NONE',  ( -48.59739992243022755, -193.5000000000000000, 0.9929810960135230236 ) ) ;
#18661 = ORIENTED_EDGE ( 'NONE', *, *, #6310, .T. ) ;
#18660 = CARTESIAN_POINT ( 'NONE',  ( -339.1964088526558498, -122.9999999999993747, 59.00000000000002132 ) ) ;
#18659 = CARTESIAN_POINT ( 'NONE',  ( -49.13194886969936448, -177.1207230881787780, -0.7575112421616214675 ) ) ;
#18662 = ORIENTED_EDGE ( 'NONE', *, *, #39133, .F. ) ;
#18663 = ADVANCED_FACE ( 'NONE', ( #29447 ), #45251, .T. ) ;
#18664 = CARTESIAN_POINT ( 'NONE',  ( -173.3294908491238004, -183.6283474603465606, -6.114457023560984972 ) ) ;
#18665 = VERTEX_POINT ( 'NONE', #37335 ) ;
#18666 = DIRECTION ( 'NONE',  ( -0.000000000000000000, 1.000000000000000000, -0.000000000000000000 ) ) ;
#18667 = CARTESIAN_POINT ( 'NONE',  ( -339.1964088526558498, -123.9999999999993747, 59.00000000000002132 ) ) ;
#18668 = ORIENTED_EDGE ( 'NONE', *, *, #47422, .T. ) ;
#18669 = CARTESIAN_POINT ( 'NONE',  ( -47.87232660569026166, -193.5000000000000000, 0.7948544414133635883 ) ) ;
#18670 = CARTESIAN_POINT ( 'NONE',  ( -141.2664123866436796, -189.7472609257535510, -83.75869879877495805 ) ) ;
#18671 = DIRECTION ( 'NONE',  ( 0.000000000000000000, -0.000000000000000000, -1.000000000000000000 ) ) ;
#18672 = CARTESIAN_POINT ( 'NONE',  ( -339.1964088526558498, -180.9052250602807703, 13.63415328425337236 ) ) ;
#18673 = VECTOR ( 'NONE', #30942, 1000.000000000000000 ) ;
#18674 = CARTESIAN_POINT ( 'NONE',  ( 61.06976976088562026, -175.3837268820161057, -60.19999396110170409 ) ) ;
#18675 = VERTEX_POINT ( 'NONE', #45499 ) ;
#18676 = DIRECTION ( 'NONE',  ( 0.000000000000000000, 0.000000000000000000, 1.000000000000000000 ) ) ;
#18677 = FACE_OUTER_BOUND ( 'NONE', #35837, .T. ) ;
#18678 = CIRCLE ( 'NONE', #42971, 125.0000000000000000 ) ;
#18679 = CARTESIAN_POINT ( 'NONE',  ( -48.77118352214581876, -183.6283474603465606, -0.9564009842765195391 ) ) ;
#18680 = EDGE_LOOP ( 'NONE', ( #31530, #41725, #5143, #32974 ) ) ;
#18681 = DIRECTION ( 'NONE',  ( -0.000000000000000000, 1.000000000000000000, -0.000000000000000000 ) ) ;
#18682 = CARTESIAN_POINT ( 'NONE',  ( -173.4460699164830260, -193.5000000000000000, -2.874563619423202265 ) ) ;
#18683 = EDGE_CURVE ( 'NONE', #10791, #26860, #51854, .T. ) ;
#18684 = DIRECTION ( 'NONE',  ( 0.000000000000000000, 1.000000000000000000, -0.000000000000000000 ) ) ;
#18685 = CARTESIAN_POINT ( 'NONE',  ( -339.1964088526558498, -68.51134412508183402, -21.38919645685240312 ) ) ;
#18686 = ORIENTED_EDGE ( 'NONE', *, *, #22852, .T. ) ;
#18687 = AXIS2_PLACEMENT_3D ( 'NONE', #18113, #49914, #5004 ) ;
#18688 = VECTOR ( 'NONE', #48474, 1000.000000000000114 ) ;
#18689 = ADVANCED_FACE ( 'NONE', ( #33418 ), #38106, .F. ) ;
#18690 = AXIS2_PLACEMENT_3D ( 'NONE', #29586, #30361, #25646 ) ;
#18691 = CARTESIAN_POINT ( 'NONE',  ( -48.47912675150885065, -175.3837268820161057, 6.938893903907228378E-15 ) ) ;
#18692 = VECTOR ( 'NONE', #14753, 1000.000000000000114 ) ;
#18693 = FACE_OUTER_BOUND ( 'NONE', #10819, .T. ) ;
#18694 = CARTESIAN_POINT ( 'NONE',  ( -336.3521761649653854, -132.3499116637027271, -59.34373651485605450 ) ) ;
#18695 = ORIENTED_EDGE ( 'NONE', *, *, #10752, .F. ) ;
#18696 = AXIS2_PLACEMENT_3D ( 'NONE', #10735, #11501, #35160 ) ;
#18697 = LINE ( 'NONE', #36919, #46166 ) ;
#18698 = LINE ( 'NONE', #22375, #9553 ) ;
#18699 = ORIENTED_EDGE ( 'NONE', *, *, #20842, .T. ) ;
#18700 = ORIENTED_EDGE ( 'NONE', *, *, #8990, .F. ) ;
#18701 = VERTEX_POINT ( 'NONE', #41530 ) ;
#18702 = CARTESIAN_POINT ( 'NONE',  ( -330.4913330509368166, -123.5000000000000284, 0.000000000000000000 ) ) ;
#18703 = CIRCLE ( 'NONE', #24582, 60.00000000000000000 ) ;
#18704 = PLANE ( 'NONE',  #41257 ) ;
#18705 = DIRECTION ( 'NONE',  ( -0.000000000000000000, 1.000000000000000000, -0.000000000000000000 ) ) ;
#18706 = ORIENTED_EDGE ( 'NONE', *, *, #33972, .T. ) ;
#18707 = AXIS2_PLACEMENT_3D ( 'NONE', #21279, #29670, #13648 ) ;
#18708 = LINE ( 'NONE', #18964, #36781 ) ;
#18709 = FACE_OUTER_BOUND ( 'NONE', #47936, .T. ) ;
#18712 = ORIENTED_EDGE ( 'NONE', *, *, #36631, .F. ) ;
#18711 = CARTESIAN_POINT ( 'NONE',  ( -46.00000000000000711, 20.00000000000000000, 46.00000000000000000 ) ) ;
#18710 = DIRECTION ( 'NONE',  ( -0.000000000000000000, -1.000000000000000000, 0.000000000000000000 ) ) ;
#18713 = DIRECTION ( 'NONE',  ( 0.000000000000000000, 0.000000000000000000, -1.000000000000000000 ) ) ;
#18714 = ORIENTED_EDGE ( 'NONE', *, *, #48615, .T. ) ;
#18715 = FACE_OUTER_BOUND ( 'NONE', #6268, .T. ) ;
#18716 = ORIENTED_EDGE ( 'NONE', *, *, #18126, .T. ) ;
#18717 = EDGE_CURVE ( 'NONE', #3693, #10327, #4847, .T. ) ;
#18718 = DIRECTION ( 'NONE',  ( -1.000000000000000000, -0.000000000000000000, 0.000000000000000000 ) ) ;
#18719 = LINE ( 'NONE', #26078, #17933 ) ;
#18720 = PLANE ( 'NONE',  #13995 ) ;
#18721 = CIRCLE ( 'NONE', #38848, 125.0000000000000000 ) ;
#18722 = AXIS2_PLACEMENT_3D ( 'NONE', #38594, #3110, #26500 ) ;
#18723 = VERTEX_POINT ( 'NONE', #19432 ) ;
#18724 = ORIENTED_EDGE ( 'NONE', *, *, #14747, .T. ) ;
#18725 = AXIS2_PLACEMENT_3D ( 'NONE', #5054, #37355, #28677 ) ;
#18726 = CARTESIAN_POINT ( 'NONE',  ( 24.07160180756802248, -193.5000000000000000, 100.5610240384924481 ) ) ;
#18727 = CARTESIAN_POINT ( 'NONE',  ( -48.47912675150885065, -188.5000000000000284, 6.938893903907228378E-15 ) ) ;
#18728 = ORIENTED_EDGE ( 'NONE', *, *, #37238, .T. ) ;
#18729 = LINE ( 'NONE', #3222, #8124 ) ;
#18730 = LINE ( 'NONE', #3719, #12233 ) ;
#18731 = ORIENTED_EDGE ( 'NONE', *, *, #17600, .F. ) ;
#18732 = DIRECTION ( 'NONE',  ( 0.000000000000000000, 0.000000000000000000, -1.000000000000000000 ) ) ;
#18733 = VECTOR ( 'NONE', #11754, 1000.000000000000227 ) ;
#18734 = CARTESIAN_POINT ( 'NONE',  ( -172.4728835572423975, -193.5000000000000000, 1.322128892812079792 ) ) ;
#18735 = ORIENTED_EDGE ( 'NONE', *, *, #30099, .T. ) ;
#18736 = CARTESIAN_POINT ( 'NONE',  ( -49.42645310536304493, -189.7472609257535510, 0.3202698538628349079 ) ) ;
#18737 = VERTEX_POINT ( 'NONE', #30485 ) ;
#18738 = DIRECTION ( 'NONE',  ( 0.08879589532293853671, 0.000000000000000000, -0.9960498426152166740 ) ) ;
#18739 = DIRECTION ( 'NONE',  ( -0.000000000000000000, 1.000000000000000000, -0.000000000000000000 ) ) ;
#18740 = EDGE_CURVE ( 'NONE', #36297, #22714, #15641, .T. ) ;
#18741 = ORIENTED_EDGE ( 'NONE', *, *, #36983, .T. ) ;
#18742 = AXIS2_PLACEMENT_3D ( 'NONE', #45259, #13183, #40298 ) ;
#18743 = DIRECTION ( 'NONE',  ( -0.9646355819083556327, 0.000000000000000000, -0.2635871660690782825 ) ) ;
#18744 = DIRECTION ( 'NONE',  ( -1.000000000000000000, 0.000000000000000000, -0.000000000000000000 ) ) ;
#18745 = CARTESIAN_POINT ( 'NONE',  ( -64.08700758308646073, -175.3837268820161057, -124.0217483183786982 ) ) ;
#18746 = AXIS2_PLACEMENT_3D ( 'NONE', #17488, #41627, #45341 ) ;
#18747 = VERTEX_POINT ( 'NONE', #18670 ) ;
#18748 = LINE ( 'NONE', #46612, #47250 ) ;
#18749 = CARTESIAN_POINT ( 'NONE',  ( -330.4913330509368166, -143.9541802141672235, -55.34326076196065003 ) ) ;
#18750 = DIRECTION ( 'NONE',  ( 1.000000000000000000, 0.000000000000000000, 0.000000000000000000 ) ) ;
#18752 = ORIENTED_EDGE ( 'NONE', *, *, #39632, .F. ) ;
#18751 = DIRECTION ( 'NONE',  ( 0.000000000000000000, 0.000000000000000000, -1.000000000000000000 ) ) ;
#18753 = VERTEX_POINT ( 'NONE', #51256 ) ;
#18754 = CARTESIAN_POINT ( 'NONE',  ( -49.08592689732745384, -177.1207230881787780, 0.7948544414133550395 ) ) ;
#18755 = ADVANCED_FACE ( 'NONE', ( #51000 ), #3659, .F. ) ;
#18756 = AXIS2_PLACEMENT_3D ( 'NONE', #34480, #34732, #50013 ) ;
#18757 = PLANE ( 'NONE',  #51465 ) ;
#18758 = VECTOR ( 'NONE', #38294, 999.9999999999998863 ) ;
#18759 = EDGE_LOOP ( 'NONE', ( #11779, #12010, #16611, #36616 ) ) ;
#18760 = LINE ( 'NONE', #10616, #40711 ) ;
#18761 = ORIENTED_EDGE ( 'NONE', *, *, #10878, .F. ) ;
#18762 = LINE ( 'NONE', #26649, #45174 ) ;
#18763 = LINE ( 'NONE', #10358, #41814 ) ;
#18764 = DIRECTION ( 'NONE',  ( -0.000000000000000000, 1.000000000000000000, -0.000000000000000000 ) ) ;
#18765 = CARTESIAN_POINT ( 'NONE',  ( -332.3517673607765914, -135.0638248728647852, 57.91551518289418254 ) ) ;
#18766 = ORIENTED_EDGE ( 'NONE', *, *, #13578, .T. ) ;
#18767 = VERTEX_POINT ( 'NONE', #31512 ) ;
#18768 = VERTEX_POINT ( 'NONE', #46529 ) ;
#18769 = EDGE_CURVE ( 'NONE', #4233, #29477, #49339, .T. ) ;
#18770 = DIRECTION ( 'NONE',  ( -4.884776371667510679E-16, 0.000000000000000000, -1.000000000000000000 ) ) ;
#18771 = PLANE ( 'NONE',  #48691 ) ;
#18772 = PLANE ( 'NONE',  #28717 ) ;
#18773 = DIRECTION ( 'NONE',  ( 0.1768902751225666370, 0.000000000000000000, 0.9842305779475979399 ) ) ;
#18774 = VECTOR ( 'NONE', #46997, 1000.000000000000000 ) ;
#18775 = EDGE_LOOP ( 'NONE', ( #43521, #42817, #18954, #13774 ) ) ;
#18776 = ADVANCED_FACE ( 'NONE', ( #34936 ), #2888, .F. ) ;
#18777 = CARTESIAN_POINT ( 'NONE',  ( -107.1845112550870027, -183.6283474603465606, 109.2239789693437331 ) ) ;
#18778 = EDGE_CURVE ( 'NONE', #48253, #16384, #18277, .T. ) ;
#18779 = VECTOR ( 'NONE', #45782, 1000.000000000000000 ) ;
#18780 = EDGE_LOOP ( 'NONE', ( #25056, #50447, #16020, #10248 ) ) ;
#18781 = ORIENTED_EDGE ( 'NONE', *, *, #21374, .F. ) ;
#18782 = DIRECTION ( 'NONE',  ( 0.000000000000000000, -0.9709418174260553425, -0.2393156642875449158 ) ) ;
#18783 = EDGE_CURVE ( 'NONE', #21100, #14977, #49218, .T. ) ;
#18784 = DIRECTION ( 'NONE',  ( 0.000000000000000000, 0.000000000000000000, -1.000000000000000000 ) ) ;
#18785 = DIRECTION ( 'NONE',  ( 0.000000000000000000, 1.000000000000000000, -0.000000000000000000 ) ) ;
#18786 = DIRECTION ( 'NONE',  ( -1.000000000000000000, -0.000000000000000000, -0.000000000000000000 ) ) ;
#18787 = DIRECTION ( 'NONE',  ( 0.000000000000000000, -0.000000000000000000, -1.000000000000000000 ) ) ;
#18788 = CARTESIAN_POINT ( 'NONE',  ( 46.00000000000000711, 33.00000000000000000, -35.00000000000000000 ) ) ;
#18789 = ORIENTED_EDGE ( 'NONE', *, *, #36507, .T. ) ;
#18790 = CARTESIAN_POINT ( 'NONE',  ( -163.3872488209693472, -177.1207230881787780, -49.20491319441547517 ) ) ;
#18791 = ORIENTED_EDGE ( 'NONE', *, *, #970, .F. ) ;
#18792 = CARTESIAN_POINT ( 'NONE',  ( -88.23625491228469286, -193.5000000000000000, 118.5089480183148254 ) ) ;
#18793 = CARTESIAN_POINT ( 'NONE',  ( -5.732832253866456007, -175.3837268820161057, -117.4638425504666657 ) ) ;
#18794 = EDGE_CURVE ( 'NONE', #45161, #36997, #27050, .T. ) ;
#18795 = ORIENTED_EDGE ( 'NONE', *, *, #17232, .T. ) ;
#18796 = DIRECTION ( 'NONE',  ( 0.000000000000000000, -1.000000000000000000, 0.000000000000000000 ) ) ;
#18797 = DIRECTION ( 'NONE',  ( 0.4031234292879730674, 0.000000000000000000, -0.9151456172430181280 ) ) ;
#18798 = CARTESIAN_POINT ( 'NONE',  ( -48.47912675150885065, -193.5000000000000000, -0.9999999999999931166 ) ) ;
#18799 = DIRECTION ( 'NONE',  ( 0.000000000000000000, 0.000000000000000000, 1.000000000000000000 ) ) ;
#18800 = VERTEX_POINT ( 'NONE', #39645 ) ;
#18801 = DIRECTION ( 'NONE',  ( -0.000000000000000000, 1.000000000000000000, -0.000000000000000000 ) ) ;
#18803 = ORIENTED_EDGE ( 'NONE', *, *, #51891, .T. ) ;
#18802 = DIRECTION ( 'NONE',  ( -0.9266896074318291543, 0.000000000000000000, -0.3758275821142488260 ) ) ;
#18804 = VECTOR ( 'NONE', #24785, 999.9999999999998863 ) ;
#18805 = VECTOR ( 'NONE', #7605, 1000.000000000000000 ) ;
#18806 = ORIENTED_EDGE ( 'NONE', *, *, #42016, .F. ) ;
#18807 = CARTESIAN_POINT ( 'NONE',  ( 72.05536924052414349, -189.7472609257535510, 33.11246405730899056 ) ) ;
#18808 = ORIENTED_EDGE ( 'NONE', *, *, #50403, .F. ) ;
#18809 = LINE ( 'NONE', #10673, #6700 ) ;
#18810 = ORIENTED_EDGE ( 'NONE', *, *, #47163, .F. ) ;
#18811 = DIRECTION ( 'NONE',  ( -0.000000000000000000, 1.000000000000000000, -0.000000000000000000 ) ) ;
#18812 = DIRECTION ( 'NONE',  ( 0.000000000000000000, 0.000000000000000000, -1.000000000000000000 ) ) ;
#18813 = ORIENTED_EDGE ( 'NONE', *, *, #436, .F. ) ;
#18814 = LINE ( 'NONE', #18565, #3131 ) ;
#18815 = EDGE_CURVE ( 'NONE', #26252, #46287, #11276, .T. ) ;
#18816 = ADVANCED_FACE ( 'NONE', ( #30738 ), #18920, .F. ) ;
#18818 = AXIS2_PLACEMENT_3D ( 'NONE', #11970, #23551, #36151 ) ;
#18817 = CARTESIAN_POINT ( 'NONE',  ( 69.99104047056319189, -189.7472609257535510, -39.87254040532513955 ) ) ;
#18819 = CARTESIAN_POINT ( 'NONE',  ( -339.1964088526558498, -74.65991953890826949, 33.10432812419072945 ) ) ;
#18820 = ORIENTED_EDGE ( 'NONE', *, *, #28177, .F. ) ;
#18821 = EDGE_LOOP ( 'NONE', ( #45596, #5425, #42176, #32931 ) ) ;
#18822 = VERTEX_POINT ( 'NONE', #35451 ) ;
#18823 = CARTESIAN_POINT ( 'NONE',  ( 0.000000000000000000, -130.6116641350635064, 58.56982357178529242 ) ) ;
#18824 = DIRECTION ( 'NONE',  ( 0.05924062789371441901, 0.000000000000000000, -0.9982437317643214625 ) ) ;
#18825 = DIRECTION ( 'NONE',  ( -1.000000000000000000, 0.000000000000000000, -0.000000000000000000 ) ) ;
#18826 = CARTESIAN_POINT ( 'NONE',  ( 46.00000000000000711, 20.00000000000000000, -46.00000000000000000 ) ) ;
#18827 = DIRECTION ( 'NONE',  ( -0.000000000000000000, 1.000000000000000000, -0.000000000000000000 ) ) ;
#18828 = VERTEX_POINT ( 'NONE', #31005 ) ;
#18829 = ADVANCED_FACE ( 'NONE', ( #6839 ), #22865, .T. ) ;
#18830 = EDGE_CURVE ( 'NONE', #50211, #25917, #35201, .T. ) ;
#18831 = CARTESIAN_POINT ( 'NONE',  ( -332.3517673607765914, -72.48138011061176655, -29.74944317415788930 ) ) ;
#18832 = EDGE_LOOP ( 'NONE', ( #36355, #37709, #16743, #31218 ) ) ;
#18834 = ORIENTED_EDGE ( 'NONE', *, *, #26882, .F. ) ;
#18833 = CARTESIAN_POINT ( 'NONE',  ( -48.71401279728982558, -177.1207230881787780, -0.9720229140804069745 ) ) ;
#18835 = ORIENTED_EDGE ( 'NONE', *, *, #33442, .F. ) ;
#18836 = EDGE_CURVE ( 'NONE', #49548, #4472, #10508, .T. ) ;
#18837 = CARTESIAN_POINT ( 'NONE',  ( -131.1972941934623975, -193.5000000000000000, 92.37913469314125336 ) ) ;
#18838 = CARTESIAN_POINT ( 'NONE',  ( 42.10477485469927927, -177.1207230881787780, 86.13684908212515268 ) ) ;
#18839 = VECTOR ( 'NONE', #4234, 1000.000000000000000 ) ;
#18840 = EDGE_CURVE ( 'NONE', #31544, #16791, #47529, .T. ) ;
#18841 = VECTOR ( 'NONE', #1792, 1000.000000000000000 ) ;
#18842 = DIRECTION ( 'NONE',  ( 0.000000000000000000, -1.000000000000000000, -1.156482317317871232E-16 ) ) ;
#18843 = CARTESIAN_POINT ( 'NONE',  ( -340.0000000000000568, -168.5000000000000284, 5.000000000000001776 ) ) ;
#18844 = ORIENTED_EDGE ( 'NONE', *, *, #48513, .T. ) ;
#18845 = FACE_OUTER_BOUND ( 'NONE', #24892, .T. ) ;
#18846 = VERTEX_POINT ( 'NONE', #14475 ) ;
#18847 = AXIS2_PLACEMENT_3D ( 'NONE', #26362, #46105, #14814 ) ;
#18848 = ORIENTED_EDGE ( 'NONE', *, *, #46097, .F. ) ;
#18849 = CARTESIAN_POINT ( 'NONE',  ( -99.02518858244150124, -175.3837268820161057, 114.3245189510261497 ) ) ;
#18850 = CARTESIAN_POINT ( 'NONE',  ( -16.00000000000001421, -63.50000000000000000, 0.000000000000000000 ) ) ;
#18851 = DIRECTION ( 'NONE',  ( 0.000000000000000000, 5.851800525628429686E-14, 1.000000000000000000 ) ) ;
#18852 = ORIENTED_EDGE ( 'NONE', *, *, #16040, .T. ) ;
#18853 = DIRECTION ( 'NONE',  ( 0.000000000000000000, 0.8805628084623552398, 0.4739294676984007193 ) ) ;
#18854 = DIRECTION ( 'NONE',  ( 0.000000000000000000, 0.000000000000000000, 1.000000000000000000 ) ) ;
#18855 = CARTESIAN_POINT ( 'NONE',  ( -87.28630321566649286, -193.5000000000000000, 118.8234112238818341 ) ) ;
#18856 = LINE ( 'NONE', #43036, #38815 ) ;
#18857 = EDGE_LOOP ( 'NONE', ( #10736, #6967, #7409, #25692 ) ) ;
#18858 = VECTOR ( 'NONE', #16905, 1000.000000000000000 ) ;
#18859 = DIRECTION ( 'NONE',  ( 0.000000000000000000, -0.000000000000000000, 1.000000000000000000 ) ) ;
#18860 = DIRECTION ( 'NONE',  ( -0.000000000000000000, 1.000000000000000000, -0.000000000000000000 ) ) ;
#18861 = CARTESIAN_POINT ( 'NONE',  ( -8.169009709621407822, -193.5000000000000000, 118.3219948448695504 ) ) ;
#18862 = ORIENTED_EDGE ( 'NONE', *, *, #24708, .F. ) ;
#18863 = CARTESIAN_POINT ( 'NONE',  ( 76.21810084846656252, -183.6283474603465606, -8.694908215727989997 ) ) ;
#18864 = CARTESIAN_POINT ( 'NONE',  ( -170.4669447856608997, -193.5000000000000000, 22.25084316132122453 ) ) ;
#18865 = ORIENTED_EDGE ( 'NONE', *, *, #40185, .F. ) ;
#18866 = CARTESIAN_POINT ( 'NONE',  ( -172.0839188101925004, -193.5000000000000000, -18.62405380494756812 ) ) ;
#18867 = ORIENTED_EDGE ( 'NONE', *, *, #51118, .F. ) ;
#18868 = EDGE_CURVE ( 'NONE', #47538, #10327, #11553, .T. ) ;
#18869 = FACE_OUTER_BOUND ( 'NONE', #47016, .T. ) ;
#18870 = AXIS2_PLACEMENT_3D ( 'NONE', #23333, #11480, #31197 ) ;
#18871 = FACE_BOUND ( 'NONE', #16689, .T. ) ;
#18872 = CARTESIAN_POINT ( 'NONE',  ( -47.57632892154311577, -175.3837268820161057, 0.4300652022765314997 ) ) ;
#18873 = CARTESIAN_POINT ( 'NONE',  ( -160.2705093830644216, -177.1207230881787780, -55.92572546981521242 ) ) ;
#18874 = VECTOR ( 'NONE', #48058, 1000.000000000000000 ) ;
#18875 = AXIS2_PLACEMENT_3D ( 'NONE', #20404, #32229, #31454 ) ;
#18876 = EDGE_CURVE ( 'NONE', #9572, #44523, #23628, .T. ) ;
#18877 = EDGE_CURVE ( 'NONE', #28248, #6855, #24941, .T. ) ;
#18878 = EDGE_CURVE ( 'NONE', #30289, #23283, #40179, .T. ) ;
#18879 = PLANE ( 'NONE',  #38639 ) ;
#18880 = VERTEX_POINT ( 'NONE', #16271 ) ;
#18881 = VECTOR ( 'NONE', #11235, 1000.000000000000114 ) ;
#18882 = ADVANCED_FACE ( 'NONE', ( #48866 ), #23887, .F. ) ;
#18883 = EDGE_LOOP ( 'NONE', ( #43401, #39571, #49288, #42576 ) ) ;
#18884 = CARTESIAN_POINT ( 'NONE',  ( 73.32083127613157103, -183.6283474603465606, 28.10285082451656535 ) ) ;
#18885 = ORIENTED_EDGE ( 'NONE', *, *, #38165, .F. ) ;
#18886 = ADVANCED_FACE ( 'NONE', ( #12319 ), #24670, .T. ) ;
#18887 = AXIS2_PLACEMENT_3D ( 'NONE', #4424, #36464, #19935 ) ;
#18888 = DIRECTION ( 'NONE',  ( 0.000000000000000000, 0.000000000000000000, 1.000000000000000000 ) ) ;
#18889 = AXIS2_PLACEMENT_3D ( 'NONE', #44022, #36132, #4094 ) ;
#18890 = ADVANCED_FACE ( 'NONE', ( #28079 ), #35990, .F. ) ;
#18891 = VECTOR ( 'NONE', #3204, 1000.000000000000000 ) ;
#18892 = ADVANCED_FACE ( 'NONE', ( #44652 ), #43859, .T. ) ;
#18893 = VECTOR ( 'NONE', #23605, 1000.000000000000000 ) ;
#18894 = DIRECTION ( 'NONE',  ( -1.000000000000000000, 0.000000000000000000, 0.000000000000000000 ) ) ;
#18895 = PLANE ( 'NONE',  #45891 ) ;
#18896 = ORIENTED_EDGE ( 'NONE', *, *, #38484, .F. ) ;
#18899 = VERTEX_POINT ( 'NONE', #3932 ) ;
#18898 = SURFACE_STYLE_FILL_AREA ( #2867 ) ;
#18897 = CARTESIAN_POINT ( 'NONE',  ( 74.00867759460086859, -189.7472609257535510, 24.93467037017222410 ) ) ;
#18900 = EDGE_CURVE ( 'NONE', #10499, #40286, #52038, .T. ) ;
#18901 = LINE ( 'NONE', #19168, #23150 ) ;
#18902 = ORIENTED_EDGE ( 'NONE', *, *, #22279, .T. ) ;
#18903 = DIRECTION ( 'NONE',  ( 0.000000000000000000, 0.000000000000000000, -1.000000000000000000 ) ) ;
#18904 = ORIENTED_EDGE ( 'NONE', *, *, #43924, .T. ) ;
#18905 = EDGE_CURVE ( 'NONE', #1914, #28854, #2204, .T. ) ;
#18906 = FACE_OUTER_BOUND ( 'NONE', #21106, .T. ) ;
#18907 = VERTEX_POINT ( 'NONE', #8128 ) ;
#18910 = ORIENTED_EDGE ( 'NONE', *, *, #10754, .T. ) ;
#18909 = CARTESIAN_POINT ( 'NONE',  ( -67.10529315269987194, -193.5000000000000000, -122.5936119678274281 ) ) ;
#18908 = DIRECTION ( 'NONE',  ( 0.000000000000000000, 1.000000000000000000, 0.000000000000000000 ) ) ;
#18911 = VERTEX_POINT ( 'NONE', #24170 ) ;
#18912 = ADVANCED_FACE ( 'NONE', ( #47826 ), #19956, .T. ) ;
#18913 = CARTESIAN_POINT ( 'NONE',  ( -305.0000000000000568, -117.8908635894569272, -59.73723787327232060 ) ) ;
#18914 = EDGE_LOOP ( 'NONE', ( #48804, #6433, #11692, #12511 ) ) ;
#18915 = PLANE ( 'NONE',  #32870 ) ;
#18916 = VECTOR ( 'NONE', #27057, 1000.000000000000000 ) ;
#18917 = DIRECTION ( 'NONE',  ( -1.000000000000000000, -0.000000000000000000, -0.000000000000000000 ) ) ;
#18918 = ORIENTED_EDGE ( 'NONE', *, *, #6729, .T. ) ;
#18919 = DIRECTION ( 'NONE',  ( 0.000000000000000000, 0.000000000000000000, 1.000000000000000000 ) ) ;
#18920 = PLANE ( 'NONE',  #632 ) ;
#18921 = DIRECTION ( 'NONE',  ( -0.000000000000000000, 0.9350162426854146114, -0.3546048870425363986 ) ) ;
#18922 = AXIS2_PLACEMENT_3D ( 'NONE', #25563, #38162, #45812 ) ;
#18923 = CARTESIAN_POINT ( 'NONE',  ( -49.45768324380835423, -175.3837268820161057, 0.2059786187410958813 ) ) ;
#18924 = VECTOR ( 'NONE', #17661, 1000.000000000000000 ) ;
#18925 = VERTEX_POINT ( 'NONE', #51769 ) ;
#18926 =( NAMED_UNIT ( * ) PLANE_ANGLE_UNIT ( ) SI_UNIT ( $, .RADIAN. ) );
#18927 = CYLINDRICAL_SURFACE ( 'NONE', #16227, 125.0000000000000000 ) ;
#18928 = ADVANCED_FACE ( 'NONE', ( #16024 ), #40681, .F. ) ;
#18930 = VECTOR ( 'NONE', #44857, 1000.000000000000000 ) ;
#18929 = CARTESIAN_POINT ( 'NONE',  ( -127.4665351220365892, -177.1207230881787780, -96.88131563365291754 ) ) ;
#18931 = CARTESIAN_POINT ( 'NONE',  ( -330.4913330509368166, -172.3400804610910200, 33.10432812419180948 ) ) ;
#18932 = ORIENTED_EDGE ( 'NONE', *, *, #21, .F. ) ;
#18933 = CARTESIAN_POINT ( 'NONE',  ( -332.3517673607765914, -123.5000000000000284, 0.000000000000000000 ) ) ;
#18934 = CARTESIAN_POINT ( 'NONE',  ( 71.18041382641612813, -189.7472609257535510, -32.52067927015755089 ) ) ;
#18935 = AXIS2_PLACEMENT_3D ( 'NONE', #33105, #45223, #20496 ) ;
#18936 = CYLINDRICAL_SURFACE ( 'NONE', #33285, 15.00000000000000000 ) ;
#18937 = CARTESIAN_POINT ( 'NONE',  ( 49.03269102277813829, 30.00000000000000355, -50.83217377521822300 ) ) ;
#18938 = DIRECTION ( 'NONE',  ( 1.000000000000000000, 0.000000000000000000, 0.000000000000000000 ) ) ;
#18939 = ORIENTED_EDGE ( 'NONE', *, *, #37816, .T. ) ;
#18940 = VECTOR ( 'NONE', #10898, 1000.000000000000114 ) ;
#18941 = AXIS2_PLACEMENT_3D ( 'NONE', #33829, #47164, #37257 ) ;
#18942 = PLANE ( 'NONE',  #10321 ) ;
#18943 = DIRECTION ( 'NONE',  ( 0.000000000000000000, -1.000000000000000000, 0.000000000000000000 ) ) ;
#18944 = FACE_OUTER_BOUND ( 'NONE', #36022, .T. ) ;
#18945 = CARTESIAN_POINT ( 'NONE',  ( 12.00000000000000000, 65.00000000000000000, 0.000000000000000000 ) ) ;
#18946 = DIRECTION ( 'NONE',  ( -0.000000000000000000, 1.000000000000000000, -0.000000000000000000 ) ) ;
#18947 = EDGE_LOOP ( 'NONE', ( #49311, #32126, #21727, #10926 ) ) ;
#18948 = ADVANCED_FACE ( 'NONE', ( #44401 ), #40957, .F. ) ;
#18949 = EDGE_CURVE ( 'NONE', #39696, #15921, #12839, .T. ) ;
#18950 = DIRECTION ( 'NONE',  ( -0.000000000000000000, 1.000000000000000000, -0.000000000000000000 ) ) ;
#18951 = EDGE_CURVE ( 'NONE', #39885, #22194, #483, .T. ) ;
#18952 = EDGE_CURVE ( 'NONE', #13133, #22275, #31791, .T. ) ;
#18953 = DIRECTION ( 'NONE',  ( 0.3482016354343928088, 0.000000000000000000, 0.9374196611341231167 ) ) ;
#18954 = ORIENTED_EDGE ( 'NONE', *, *, #47034, .F. ) ;
#18955 = ORIENTED_EDGE ( 'NONE', *, *, #4011, .T. ) ;
#18956 = AXIS2_PLACEMENT_3D ( 'NONE', #23635, #47577, #11560 ) ;
#18957 = VERTEX_POINT ( 'NONE', #765 ) ;
#18958 = MANIFOLD_SOLID_BREP ( 'Fillet1', #17870 ) ;
#18959 = DIRECTION ( 'NONE',  ( -0.000000000000000000, -0.1205366802553130001, 0.9927088740980551940 ) ) ;
#18960 = AXIS2_PLACEMENT_3D ( 'NONE', #761, #29125, #21513 ) ;
#18961 = AXIS2_PLACEMENT_3D ( 'NONE', #27592, #31525, #23640 ) ;
#18962 = LINE ( 'NONE', #43399, #37891 ) ;
#18963 = ORIENTED_EDGE ( 'NONE', *, *, #15279, .T. ) ;
#18964 = CARTESIAN_POINT ( 'NONE',  ( 34.98161733638499982, -193.5000000000000000, -91.70840728318313495 ) ) ;
#18965 = CARTESIAN_POINT ( 'NONE',  ( -332.3517673607765914, -111.9361751271348879, -57.91551518289410438 ) ) ;
#18968 = ORIENTED_EDGE ( 'NONE', *, *, #9575, .F. ) ;
#18967 = LINE ( 'NONE', #7134, #22429 ) ;
#18966 = CARTESIAN_POINT ( 'NONE',  ( -6.081033889300861972, -193.5000000000000000, -116.5264228893325509 ) ) ;
#18969 = ADVANCED_FACE ( 'NONE', ( #9177 ), #19685, .F. ) ;
#18970 = VECTOR ( 'NONE', #44828, 1000.000000000000114 ) ;
#18971 = CIRCLE ( 'NONE', #26502, 60.00000000000000000 ) ;
#18972 = DIRECTION ( 'NONE',  ( 0.000000000000000000, -1.000000000000000000, 0.000000000000000000 ) ) ;
#18973 = ORIENTED_EDGE ( 'NONE', *, *, #40704, .F. ) ;
#18974 = CARTESIAN_POINT ( 'NONE',  ( -336.3521761649653854, -162.0508476703726330, 45.97643030831914501 ) ) ;
#18975 = ORIENTED_EDGE ( 'NONE', *, *, #16404, .T. ) ;
#18976 = DIRECTION ( 'NONE',  ( 0.000000000000000000, 0.000000000000000000, -1.000000000000000000 ) ) ;
#18977 = VECTOR ( 'NONE', #34174, 1000.000000000000000 ) ;
#18978 = DIRECTION ( 'NONE',  ( -0.000000000000000000, 1.000000000000000000, -0.000000000000000000 ) ) ;
#18980 = CYLINDRICAL_SURFACE ( 'NONE', #48347, 125.0000000000000000 ) ;
#18979 = CARTESIAN_POINT ( 'NONE',  ( -104.3615810019516630, -189.7472609257535510, 110.6939782313525455 ) ) ;
#18981 = EDGE_LOOP ( 'NONE', ( #10624, #21725, #47715, #14444 ) ) ;
#18982 = EDGE_CURVE ( 'NONE', #48695, #39147, #25729, .T. ) ;
#18983 = VECTOR ( 'NONE', #16789, 1000.000000000000000 ) ;
#18984 = ORIENTED_EDGE ( 'NONE', *, *, #17090, .F. ) ;
#18985 = CARTESIAN_POINT ( 'NONE',  ( -339.1964088526558498, -84.75001853787875916, -44.49369547121548862 ) ) ;
#18986 = DIRECTION ( 'NONE',  ( 0.9982437317643210184, 0.000000000000000000, 0.05924062789372143423 ) ) ;
#18987 = ORIENTED_EDGE ( 'NONE', *, *, #28681, .F. ) ;
#18988 = LINE ( 'NONE', #26858, #33295 ) ;
#18989 = CARTESIAN_POINT ( 'NONE',  ( -49.03777351731249468, -175.3837268820161057, -0.8294056854502022125 ) ) ;
#18990 = EDGE_LOOP ( 'NONE', ( #47829, #41191, #50160, #5289 ) ) ;
#18991 = FACE_BOUND ( 'NONE', #37638, .T. ) ;
#18992 = PLANE ( 'NONE',  #13901 ) ;
#18993 = VERTEX_POINT ( 'NONE', #17327 ) ;
#18994 = CARTESIAN_POINT ( 'NONE',  ( -339.1964088526558498, -84.75001853787875916, -44.49369547121548862 ) ) ;
#18995 = VERTEX_POINT ( 'NONE', #21257 ) ;
#18996 = AXIS2_PLACEMENT_3D ( 'NONE', #40125, #3875, #35150 ) ;
#18997 = AXIS2_PLACEMENT_3D ( 'NONE', #168, #48794, #32227 ) ;
#18998 = FACE_OUTER_BOUND ( 'NONE', #2318, .T. ) ;
#18999 = ORIENTED_EDGE ( 'NONE', *, *, #40726, .T. ) ;
#19000 = AXIS2_PLACEMENT_3D ( 'NONE', #34618, #29641, #34112 ) ;
#19001 = AXIS2_PLACEMENT_3D ( 'NONE', #22785, #18579, #22258 ) ;
#19002 = CARTESIAN_POINT ( 'NONE',  ( -339.1964088526558498, -89.57268800991514013, -48.27201571436026484 ) ) ;
#19003 = CARTESIAN_POINT ( 'NONE',  ( -332.3517673607765914, -80.37812621821328207, -41.71934804796994456 ) ) ;
#19004 = DIRECTION ( 'NONE',  ( -1.000000000000000000, 0.000000000000000000, 0.000000000000000000 ) ) ;
#19005 = ORIENTED_EDGE ( 'NONE', *, *, #4131, .T. ) ;
#19006 = CARTESIAN_POINT ( 'NONE',  ( -91.22542124915045747, -175.3837268820161057, 117.4638425504669783 ) ) ;
#19007 = AXIS2_PLACEMENT_3D ( 'NONE', #40812, #1127, #45047 ) ;
#19008 = VECTOR ( 'NONE', #43923, 1000.000000000000000 ) ;
#19009 = DIRECTION ( 'NONE',  ( -0.000000000000000000, 1.000000000000000000, -0.000000000000000000 ) ) ;
#19010 = DIRECTION ( 'NONE',  ( -0.000000000000000000, 1.000000000000000000, -0.000000000000000000 ) ) ;
#19012 = VERTEX_POINT ( 'NONE', #29128 ) ;
#19011 = FACE_OUTER_BOUND ( 'NONE', #17944, .T. ) ;
#19013 = AXIS2_PLACEMENT_3D ( 'NONE', #22803, #30420, #46465 ) ;
#19014 = ORIENTED_EDGE ( 'NONE', *, *, #29331, .F. ) ;
#19015 = EDGE_CURVE ( 'NONE', #47856, #16704, #13625, .T. ) ;
#19016 = ADVANCED_FACE ( 'NONE', ( #13890 ), #45190, .F. ) ;
#19017 = CARTESIAN_POINT ( 'NONE',  ( -151.4272465800706016, -193.5000000000000000, 70.89911581792887318 ) ) ;
#19018 = VECTOR ( 'NONE', #31939, 1000.000000000000000 ) ;
#19019 = VECTOR ( 'NONE', #51889, 1000.000000000000000 ) ;
#19020 = DIRECTION ( 'NONE',  ( 0.000000000000000000, 0.4647231720437695057, 0.8854560256532093554 ) ) ;
#19021 = VERTEX_POINT ( 'NONE', #22024 ) ;
#19022 = ORIENTED_EDGE ( 'NONE', *, *, #47365, .F. ) ;
#19023 = DIRECTION ( 'NONE',  ( 0.02963332782254913048, 0.000000000000000000, 0.9995608365087946812 ) ) ;
#19024 = AXIS2_PLACEMENT_3D ( 'NONE', #26010, #37591, #22065 ) ;
#19025 = ORIENTED_EDGE ( 'NONE', *, *, #39677, .T. ) ;
#19026 = DIRECTION ( 'NONE',  ( 0.000000000000000000, 0.000000000000000000, 1.000000000000000000 ) ) ;
#19027 = DIRECTION ( 'NONE',  ( 0.000000000000000000, 1.000000000000000000, -0.000000000000000000 ) ) ;
#19028 = CARTESIAN_POINT ( 'NONE',  ( 1.959434878635765131E-15, -53.50000000000000000, 16.00000000000000000 ) ) ;
#19029 = FACE_OUTER_BOUND ( 'NONE', #199, .T. ) ;
#19030 = ORIENTED_EDGE ( 'NONE', *, *, #32193, .F. ) ;
#19031 = ORIENTED_EDGE ( 'NONE', *, *, #18876, .F. ) ;
#19032 = ORIENTED_EDGE ( 'NONE', *, *, #10584, .F. ) ;
#19033 = DIRECTION ( 'NONE',  ( -0.000000000000000000, 1.000000000000000000, -0.000000000000000000 ) ) ;
#19034 = DIRECTION ( 'NONE',  ( 0.000000000000000000, 1.000000000000000000, 0.000000000000000000 ) ) ;
#19035 = VECTOR ( 'NONE', #43226, 1000.000000000000000 ) ;
#19036 = CARTESIAN_POINT ( 'NONE',  ( 46.00000000000000711, 20.00000000000000000, -51.00000000000000000 ) ) ;
#19037 = VECTOR ( 'NONE', #42391, 1000.000000000000000 ) ;
#19038 = EDGE_CURVE ( 'NONE', #4051, #49012, #14159, .T. ) ;
#19039 = DIRECTION ( 'NONE',  ( -1.000000000000000000, 0.000000000000000000, 0.000000000000000000 ) ) ;
#19040 = FACE_OUTER_BOUND ( 'NONE', #12823, .T. ) ;
#19041 = ORIENTED_EDGE ( 'NONE', *, *, #34971, .T. ) ;
#19042 = AXIS2_PLACEMENT_3D ( 'NONE', #13714, #1098, #33443 ) ;
#19043 = LINE ( 'NONE', #46914, #35693 ) ;
#19044 = ADVANCED_FACE ( 'NONE', ( #37278 ), #29644, .T. ) ;
#19045 = ORIENTED_EDGE ( 'NONE', *, *, #26943, .F. ) ;
#19046 = EDGE_LOOP ( 'NONE', ( #18076, #671, #31236, #26618 ) ) ;
#19047 = VECTOR ( 'NONE', #22673, 1000.000000000000000 ) ;
#19048 = CARTESIAN_POINT ( 'NONE',  ( -332.3517673607765914, -65.24746378767824240, -9.724760635741734660 ) ) ;
#19049 = PLANE ( 'NONE',  #47432 ) ;
#19050 = CYLINDRICAL_SURFACE ( 'NONE', #35907, 125.0000000000000000 ) ;
#19051 = AXIS2_PLACEMENT_3D ( 'NONE', #37612, #2109, #21846 ) ;
#19052 = CARTESIAN_POINT ( 'NONE',  ( -305.0000000000000568, -71.15086438280971493, -29.31839013542551342 ) ) ;
#19053 = AXIS2_PLACEMENT_3D ( 'NONE', #6645, #27632, #23182 ) ;
#19054 = VECTOR ( 'NONE', #2696, 1000.000000000000114 ) ;
#19055 = CARTESIAN_POINT ( 'NONE',  ( 55.03325008324584644, -183.6283474603465606, -70.07273251429357686 ) ) ;
#19056 = DIRECTION ( 'NONE',  ( 1.000000000000000000, -0.000000000000000000, -0.000000000000000000 ) ) ;
#19057 = ORIENTED_EDGE ( 'NONE', *, *, #23168, .T. ) ;
#19059 = EDGE_CURVE ( 'NONE', #10177, #12033, #9954, .T. ) ;
#19058 = LINE ( 'NONE', #6716, #14175 ) ;
#19060 = VECTOR ( 'NONE', #1962, 999.9999999999998863 ) ;
#19061 = CIRCLE ( 'NONE', #25773, 125.0000000000000000 ) ;
#19062 = VERTEX_POINT ( 'NONE', #6001 ) ;
#19063 = DIRECTION ( 'NONE',  ( 0.000000000000000000, 0.000000000000000000, 1.000000000000000000 ) ) ;
#19064 = DIRECTION ( 'NONE',  ( 0.8896570909947499883, 0.000000000000000000, -0.4566292373937077542 ) ) ;
#19065 = VERTEX_POINT ( 'NONE', #29385 ) ;
#19066 = CARTESIAN_POINT ( 'NONE',  ( -162.3451783319732726, -177.1207230881787780, 51.57055649762781968 ) ) ;
#19067 = FACE_OUTER_BOUND ( 'NONE', #40791, .T. ) ;
#19068 = LINE ( 'NONE', #43743, #1347 ) ;
#19069 = CARTESIAN_POINT ( 'NONE',  ( -172.0042974347349229, -193.5000000000000000, 10.84123789944660210 ) ) ;
#19070 = EDGE_CURVE ( 'NONE', #32782, #22041, #8091, .T. ) ;
#19071 = CARTESIAN_POINT ( 'NONE',  ( -48.47912675150885065, -175.3837268820161057, 6.938893903907228378E-15 ) ) ;
#19072 = VERTEX_POINT ( 'NONE', #21516 ) ;
#19073 = VECTOR ( 'NONE', #43014, 1000.000000000000000 ) ;
#19074 = VECTOR ( 'NONE', #48351, 1000.000000000000000 ) ;
#19075 = CARTESIAN_POINT ( 'NONE',  ( 0.000000000000000000, -167.6621341420946578, 39.12423683620730230 ) ) ;
#19077 = ORIENTED_EDGE ( 'NONE', *, *, #17676, .T. ) ;
#19076 = CARTESIAN_POINT ( 'NONE',  ( -332.3517673607765914, -123.5000000000000284, 0.000000000000000000 ) ) ;
#19078 = AXIS2_PLACEMENT_3D ( 'NONE', #20765, #16835, #24440 ) ;
#19079 = VERTEX_POINT ( 'NONE', #50166 ) ;
#19080 = DIRECTION ( 'NONE',  ( 1.000000000000000000, -0.000000000000000000, -0.000000000000000000 ) ) ;
#19081 = ADVANCED_FACE ( 'NONE', ( #38045 ), #5764, .T. ) ;
#19082 = ADVANCED_FACE ( 'NONE', ( #17067 ), #37018, .T. ) ;
#19083 = ORIENTED_EDGE ( 'NONE', *, *, #27480, .T. ) ;
#19084 = LINE ( 'NONE', #23288, #48643 ) ;
#19085 = VECTOR ( 'NONE', #23492, 1000.000000000000114 ) ;
#19086 = EDGE_CURVE ( 'NONE', #7533, #11977, #31603, .T. ) ;
#19087 = ORIENTED_EDGE ( 'NONE', *, *, #51025, .T. ) ;
#19088 = PLANE ( 'NONE',  #23097 ) ;
#19089 = VECTOR ( 'NONE', #24451, 1000.000000000000000 ) ;
#19090 = DIRECTION ( 'NONE',  ( -0.000000000000000000, 0.1205366802553337752, 0.9927088740980526405 ) ) ;
#19091 = ORIENTED_EDGE ( 'NONE', *, *, #46435, .F. ) ;
#19092 = CARTESIAN_POINT ( 'NONE',  ( -173.4291566779743050, -193.5000000000000000, 3.534122433558352760 ) ) ;
#19093 = AXIS2_PLACEMENT_3D ( 'NONE', #9100, #21430, #9356 ) ;
#19094 = LINE ( 'NONE', #31686, #17729 ) ;
#19095 = LINE ( 'NONE', #19598, #19018 ) ;
#19096 = VERTEX_POINT ( 'NONE', #10446 ) ;
#19097 = VERTEX_POINT ( 'NONE', #47947 ) ;
#19098 = ORIENTED_EDGE ( 'NONE', *, *, #37534, .F. ) ;
#19099 = VECTOR ( 'NONE', #23666, 1000.000000000000000 ) ;
#19100 = CARTESIAN_POINT ( 'NONE',  ( -180.0000000000000568, -123.5000000000000284, 45.63467731922665394 ) ) ;
#19101 = CARTESIAN_POINT ( 'NONE',  ( -31.47951320919343488, -193.5000000000000000, -122.8300162461135301 ) ) ;
#19102 = EDGE_CURVE ( 'NONE', #49449, #19466, #14827, .T. ) ;
#19103 = LINE ( 'NONE', #11198, #44433 ) ;
#19104 = DIRECTION ( 'NONE',  ( 0.000000000000000000, 1.000000000000000000, 0.000000000000000000 ) ) ;
#19105 = CARTESIAN_POINT ( 'NONE',  ( -332.3517673607765914, -103.7577981350106313, -56.65902810251876787 ) ) ;
#19106 = ORIENTED_EDGE ( 'NONE', *, *, #9108, .T. ) ;
#19107 = LINE ( 'NONE', #31433, #43386 ) ;
#19108 = ORIENTED_EDGE ( 'NONE', *, *, #41035, .T. ) ;
#19110 = ORIENTED_EDGE ( 'NONE', *, *, #49356, .T. ) ;
#19109 = CARTESIAN_POINT ( 'NONE',  ( -48.71401279728984690, -189.7472609257535510, 0.9720229140804159673 ) ) ;
#19111 = VECTOR ( 'NONE', #41590, 1000.000000000000000 ) ;
#19112 = VERTEX_POINT ( 'NONE', #18604 ) ;
#19113 = VECTOR ( 'NONE', #31504, 1000.000000000000114 ) ;
#19114 = CARTESIAN_POINT ( 'NONE',  ( -330.4913330509368166, -130.1153096980153236, -58.63009191191284941 ) ) ;
#19115 = PLANE ( 'NONE',  #47646 ) ;
#19116 = AXIS2_PLACEMENT_3D ( 'NONE', #20112, #44809, #134 ) ;
#19117 = DIRECTION ( 'NONE',  ( 0.000000000000000000, 0.7485107481711024136, 0.6631226582407937498 ) ) ;
#19118 = DIRECTION ( 'NONE',  ( 0.3482016354343995812, 0.000000000000000000, -0.9374196611341205632 ) ) ;
#19119 = ORIENTED_EDGE ( 'NONE', *, *, #14094, .T. ) ;
#19120 = CARTESIAN_POINT ( 'NONE',  ( -161.6832731452239500, -189.7472609257535510, -53.00774697410101055 ) ) ;
#19121 = VERTEX_POINT ( 'NONE', #16150 ) ;
#19122 = EDGE_LOOP ( 'NONE', ( #30374, #13165, #49229, #24774 ) ) ;
#19123 = DIRECTION ( 'NONE',  ( 0.000000000000000000, -0.8229838658936556861, 0.5680647467311569221 ) ) ;
#19124 = AXIS2_PLACEMENT_3D ( 'NONE', #31417, #23796, #27477 ) ;
#19125 = FACE_OUTER_BOUND ( 'NONE', #15227, .T. ) ;
#19126 = ORIENTED_EDGE ( 'NONE', *, *, #6452, .F. ) ;
#19127 = CIRCLE ( 'NONE', #21647, 125.0000000000000000 ) ;
#19128 = PLANE ( 'NONE',  #21514 ) ;
#19129 = DIRECTION ( 'NONE',  ( 0.6528221181905174975, 0.000000000000000000, 0.7575112421616236880 ) ) ;
#19130 = EDGE_CURVE ( 'NONE', #33399, #21096, #45880, .T. ) ;
#19131 = CARTESIAN_POINT ( 'NONE',  ( -490.0000000000001137, -168.5000000000000284, 0.000000000000000000 ) ) ;
#19132 = DIRECTION ( 'NONE',  ( 0.000000000000000000, 0.000000000000000000, -1.000000000000000000 ) ) ;
#19133 = EDGE_LOOP ( 'NONE', ( #13066, #43600, #18507, #21110 ) ) ;
#19134 = DIRECTION ( 'NONE',  ( -0.000000000000000000, 1.000000000000000000, -0.000000000000000000 ) ) ;
#19135 = DIRECTION ( 'NONE',  ( 0.5085311186492273983, 0.000000000000000000, -0.8610436117673514467 ) ) ;
#19136 = VECTOR ( 'NONE', #48388, 1000.000000000000000 ) ;
#19137 = CARTESIAN_POINT ( 'NONE',  ( -330.4913330509368166, -89.57268800991514013, -48.27201571436026484 ) ) ;
#19138 = ORIENTED_EDGE ( 'NONE', *, *, #28258, .F. ) ;
#19139 = CARTESIAN_POINT ( 'NONE',  ( -173.1763543514842070, -193.5000000000000000, 8.694908215728892387 ) ) ;
#19140 = CARTESIAN_POINT ( 'NONE',  ( -170.0000000000000284, -123.5000000000000284, 45.63467731922665394 ) ) ;
#19141 = EDGE_LOOP ( 'NONE', ( #51518, #41362 ) ) ;
#19142 = DIRECTION ( 'NONE',  ( 0.000000000000000000, 0.000000000000000000, -1.000000000000000000 ) ) ;
#19143 = EDGE_CURVE ( 'NONE', #31601, #43746, #2248, .T. ) ;
#19144 = ORIENTED_EDGE ( 'NONE', *, *, #50049, .F. ) ;
#19145 = EDGE_CURVE ( 'NONE', #43547, #16663, #7270, .T. ) ;
#19146 = AXIS2_PLACEMENT_3D ( 'NONE', #30807, #14271, #6894 ) ;
#19147 = CARTESIAN_POINT ( 'NONE',  ( -336.3521761649654422, -149.4733471526596134, 53.00046796564699036 ) ) ;
#19148 = AXIS2_PLACEMENT_3D ( 'NONE', #25136, #22214, #17247 ) ;
#19149 = EDGE_CURVE ( 'NONE', #39380, #16176, #39777, .T. ) ;
#19150 = FACE_BOUND ( 'NONE', #1426, .T. ) ;
#19152 = ORIENTED_EDGE ( 'NONE', *, *, #47711, .F. ) ;
#19151 = LINE ( 'NONE', #35415, #26243 ) ;
#19153 = AXIS2_PLACEMENT_3D ( 'NONE', #30852, #7192, #42925 ) ;
#19154 = DIRECTION ( 'NONE',  ( 1.000000000000000000, -0.000000000000000000, -0.000000000000000000 ) ) ;
#19155 = ORIENTED_EDGE ( 'NONE', *, *, #16890, .F. ) ;
#19156 = ORIENTED_EDGE ( 'NONE', *, *, #24591, .F. ) ;
#19157 = DIRECTION ( 'NONE',  ( 0.000000000000000000, 0.000000000000000000, 1.000000000000000000 ) ) ;
#19158 = AXIS2_PLACEMENT_3D ( 'NONE', #21028, #43957, #40005 ) ;
#19159 = ORIENTED_EDGE ( 'NONE', *, *, #2739, .F. ) ;
#19160 = CARTESIAN_POINT ( 'NONE',  ( -146.8460685364478593, -177.1207230881787780, 75.49882471933935335 ) ) ;
#19161 = AXIS2_PLACEMENT_3D ( 'NONE', #9674, #46458, #10438 ) ;
#19162 = CARTESIAN_POINT ( 'NONE',  ( -339.1964088526558498, -167.9936954712150339, 38.74998146212178796 ) ) ;
#19163 = LINE ( 'NONE', #34911, #16513 ) ;
#19164 = EDGE_LOOP ( 'NONE', ( #22854, #18570, #48255, #7957 ) ) ;
#19167 = ORIENTED_EDGE ( 'NONE', *, *, #4640, .F. ) ;
#19166 = CARTESIAN_POINT ( 'NONE',  ( 55.92943606843918047, -175.3837268820161057, -66.89437584437831674 ) ) ;
#19165 = CARTESIAN_POINT ( 'NONE',  ( -4.462159545581665832, 54.38183208324189621, -18.37010509431258498 ) ) ;
#19168 = CARTESIAN_POINT ( 'NONE',  ( -18.54723674587610205, -193.5000000000000000, 120.3332351033025844 ) ) ;
#19169 = EDGE_LOOP ( 'NONE', ( #34146, #51321, #45173, #23659 ) ) ;
#19170 = LINE ( 'NONE', #39630, #49958 ) ;
#19171 = EDGE_LOOP ( 'NONE', ( #32409, #11215, #7846, #31781 ) ) ;
#19172 = CARTESIAN_POINT ( 'NONE',  ( -332.3517673607765914, -123.5000000000000284, 0.000000000000000000 ) ) ;
#19173 = VERTEX_POINT ( 'NONE', #10717 ) ;
#19175 = DIRECTION ( 'NONE',  ( 0.000000000000000000, 0.000000000000000000, 1.000000000000000000 ) ) ;
#19174 = DIRECTION ( 'NONE',  ( -1.000000000000000000, 0.000000000000000000, 0.000000000000000000 ) ) ;
#19176 = ORIENTED_EDGE ( 'NONE', *, *, #33377, .F. ) ;
#19177 = CARTESIAN_POINT ( 'NONE',  ( -330.4913330509368166, -96.52406086224436876, -52.47426709956133806 ) ) ;
#19178 = EDGE_CURVE ( 'NONE', #19715, #24408, #40486, .T. ) ;
#19179 = VERTEX_POINT ( 'NONE', #19816 ) ;
#19180 = CARTESIAN_POINT ( 'NONE',  ( -330.4913330509368166, -68.51134412508180560, -21.38919645685231075 ) ) ;
#19181 = CIRCLE ( 'NONE', #30090, 125.0000000000000000 ) ;
#19182 = CARTESIAN_POINT ( 'NONE',  ( 48.66843973345087448, 30.00000000000000355, -40.95752564483601788 ) ) ;
#19183 = ORIENTED_EDGE ( 'NONE', *, *, #39738, .F. ) ;
#19184 = VECTOR ( 'NONE', #43587, 1000.000000000000000 ) ;
#19185 = CARTESIAN_POINT ( 'NONE',  ( -25.55153130240594450, -193.5000000000000000, 122.8793122007210599 ) ) ;
#19186 = DIRECTION ( 'NONE',  ( 0.000000000000000000, 0.000000000000000000, -1.000000000000000000 ) ) ;
#19187 = DIRECTION ( 'NONE',  ( -0.000000000000000000, 1.000000000000000000, 0.000000000000000000 ) ) ;
#19188 = AXIS2_PLACEMENT_3D ( 'NONE', #9211, #29680, #44689 ) ;
#19189 = DIRECTION ( 'NONE',  ( -0.000000000000000000, 1.000000000000000000, -0.000000000000000000 ) ) ;
#19190 = EDGE_CURVE ( 'NONE', #16507, #35850, #29924, .T. ) ;
#19191 = EDGE_CURVE ( 'NONE', #4441, #10029, #37461, .T. ) ;
#19192 = ORIENTED_EDGE ( 'NONE', *, *, #42726, .T. ) ;
#19193 = EDGE_CURVE ( 'NONE', #36633, #38465, #14409, .T. ) ;
#19194 = DIRECTION ( 'NONE',  ( 0.000000000000000000, 0.000000000000000000, 1.000000000000000000 ) ) ;
#19195 = DIRECTION ( 'NONE',  ( -0.7765238627180349740, 0.000000000000000000, -0.6300878435817203194 ) ) ;
#19196 = DIRECTION ( 'NONE',  ( 0.000000000000000000, 0.000000000000000000, -1.000000000000000000 ) ) ;
#19197 = ADVANCED_FACE ( 'NONE', ( #24026 ), #42777, .T. ) ;
#19198 = LINE ( 'NONE', #14738, #11985 ) ;
#19199 = VERTEX_POINT ( 'NONE', #6782 ) ;
#19200 = VECTOR ( 'NONE', #30917, 1000.000000000000000 ) ;
#19201 = EDGE_CURVE ( 'NONE', #2635, #16080, #30944, .T. ) ;
#19202 = EDGE_CURVE ( 'NONE', #27293, #44533, #14661, .T. ) ;
#19203 = CARTESIAN_POINT ( 'NONE',  ( -109.0835867659424565, -177.1207230881787780, -109.3256576763154726 ) ) ;
#19204 = CARTESIAN_POINT ( 'NONE',  ( -46.00000000000000711, 0.000000000000000000, -41.00000000000000000 ) ) ;
#19206 = EDGE_LOOP ( 'NONE', ( #17635, #35639, #8933, #21008 ) ) ;
#19205 = CARTESIAN_POINT ( 'NONE',  ( -336.3521761649654422, -64.50000000000000000, -2.632288850093980503 ) ) ;
#19207 = ORIENTED_EDGE ( 'NONE', *, *, #18656, .F. ) ;
#19208 = EDGE_CURVE ( 'NONE', #39811, #44661, #36110, .T. ) ;
#19209 = EDGE_CURVE ( 'NONE', #49503, #41529, #39993, .T. ) ;
#19210 = CIRCLE ( 'NONE', #32628, 60.00000000000000000 ) ;
#19211 = EDGE_CURVE ( 'NONE', #9678, #39413, #32166, .T. ) ;
#19212 = DIRECTION ( 'NONE',  ( 0.000000000000000000, 0.000000000000000000, -1.000000000000000000 ) ) ;
#19214 = EDGE_CURVE ( 'NONE', #31341, #6500, #26993, .T. ) ;
#19213 = CARTESIAN_POINT ( 'NONE',  ( -48.47912675150885065, -175.3837268820161057, 6.938893903907228378E-15 ) ) ;
#19215 = DIRECTION ( 'NONE',  ( 1.000000000000000000, 0.000000000000000000, 0.000000000000000000 ) ) ;
#19216 = CARTESIAN_POINT ( 'NONE',  ( -47.66663987350317200, -193.5000000000000000, -0.5829794791144634614 ) ) ;
#19217 = DIRECTION ( 'NONE',  ( -0.000000000000000000, 1.000000000000000000, -0.000000000000000000 ) ) ;
#19218 = ADVANCED_FACE ( 'NONE', ( #23063 ), #26475, .F. ) ;
#19219 = ORIENTED_EDGE ( 'NONE', *, *, #48206, .T. ) ;
#19220 = DIRECTION ( 'NONE',  ( -0.000000000000000000, -1.000000000000000000, -0.000000000000000000 ) ) ;
#19221 = ORIENTED_EDGE ( 'NONE', *, *, #47787, .F. ) ;
#19222 = ORIENTED_EDGE ( 'NONE', *, *, #32416, .F. ) ;
#19223 = AXIS2_PLACEMENT_3D ( 'NONE', #12068, #20758, #16569 ) ;
#19224 = ORIENTED_EDGE ( 'NONE', *, *, #48522, .T. ) ;
#19225 = DIRECTION ( 'NONE',  ( -0.000000000000000000, 1.000000000000000000, -0.000000000000000000 ) ) ;
#19226 = AXIS2_PLACEMENT_3D ( 'NONE', #46763, #10751, #42028 ) ;
#19227 = DIRECTION ( 'NONE',  ( 0.000000000000000000, 0.000000000000000000, 1.000000000000000000 ) ) ;
#19228 = ORIENTED_EDGE ( 'NONE', *, *, #47422, .F. ) ;
#19229 = ADVANCED_FACE ( 'NONE', ( #2571 ), #12450, .F. ) ;
#19230 = CARTESIAN_POINT ( 'NONE',  ( 76.46082103836693022, -175.3837268820161057, 3.874202661595785635 ) ) ;
#19231 = CARTESIAN_POINT ( 'NONE',  ( -47.53180039765466347, -183.6283474603465606, 0.3202698538628485636 ) ) ;
#19232 = AXIS2_PLACEMENT_3D ( 'NONE', #30130, #14362, #21472 ) ;
#19235 = VERTEX_POINT ( 'NONE', #25327 ) ;
#19234 = PLANE ( 'NONE',  #26622 ) ;
#19233 = DIRECTION ( 'NONE',  ( -0.000000000000000000, 0.1205366802553095168, -0.9927088740980556381 ) ) ;
#19236 = CARTESIAN_POINT ( 'NONE',  ( -78.00521078983979351, -175.3837268820161057, 121.4627941443857111 ) ) ;
#19237 = VERTEX_POINT ( 'NONE', #24289 ) ;
#19238 = FACE_OUTER_BOUND ( 'NONE', #9580, .T. ) ;
#19239 = VERTEX_POINT ( 'NONE', #36366 ) ;
#19240 = DIRECTION ( 'NONE',  ( -0.000000000000000000, -1.000000000000000000, 0.000000000000000000 ) ) ;
#19241 = CARTESIAN_POINT ( 'NONE',  ( -305.0000000000000568, -176.8578783931336602, 27.43969411971573891 ) ) ;
#19243 = CARTESIAN_POINT ( 'NONE',  ( -49.08592689732743963, -193.5000000000000000, -0.7948544414133539293 ) ) ;
#19242 = FACE_OUTER_BOUND ( 'NONE', #46035, .T. ) ;
#19244 = ORIENTED_EDGE ( 'NONE', *, *, #11696, .F. ) ;
#19245 = VECTOR ( 'NONE', #49571, 1000.000000000000000 ) ;
#19246 = EDGE_CURVE ( 'NONE', #41165, #50970, #4312, .T. ) ;
#19247 = CARTESIAN_POINT ( 'NONE',  ( -330.4913330509368166, -95.63860483659048839, 52.00954392751722111 ) ) ;
#19248 = ORIENTED_EDGE ( 'NONE', *, *, #24000, .F. ) ;
#19249 = LINE ( 'NONE', #11082, #13903 ) ;
#19250 = PLANE ( 'NONE',  #34260 ) ;
#19251 = ORIENTED_EDGE ( 'NONE', *, *, #51913, .T. ) ;
#19252 = LINE ( 'NONE', #47630, #42522 ) ;
#19253 = CYLINDRICAL_SURFACE ( 'NONE', #23166, 125.0000000000000000 ) ;
#19254 = EDGE_CURVE ( 'NONE', #23051, #23027, #8766, .T. ) ;
#19255 = EDGE_CURVE ( 'NONE', #50353, #26805, #5597, .T. ) ;
#19256 = ADVANCED_FACE ( 'NONE', ( #33202 ), #45320, .T. ) ;
#19257 = ORIENTED_EDGE ( 'NONE', *, *, #30184, .T. ) ;
#19258 = EDGE_CURVE ( 'NONE', #16764, #18124, #17465, .T. ) ;
#19259 = FACE_BOUND ( 'NONE', #37471, .T. ) ;
#19260 = CARTESIAN_POINT ( 'NONE',  ( -330.4913330509368166, -138.1050951016783301, 57.16590939599346655 ) ) ;
#19261 = EDGE_CURVE ( 'NONE', #21480, #35003, #24804, .T. ) ;
#19262 = ORIENTED_EDGE ( 'NONE', *, *, #24652, .T. ) ;
#19263 = DIRECTION ( 'NONE',  ( 0.000000000000000000, 0.000000000000000000, -1.000000000000000000 ) ) ;
#19264 = VERTEX_POINT ( 'NONE', #20597 ) ;
#19265 = CIRCLE ( 'NONE', #28462, 125.0000000000000000 ) ;
#19266 = FACE_OUTER_BOUND ( 'NONE', #38225, .T. ) ;
#19267 = EDGE_CURVE ( 'NONE', #15270, #20782, #4574, .T. ) ;
#19268 = DIRECTION ( 'NONE',  ( 0.000000000000000000, -0.000000000000000000, 1.000000000000000000 ) ) ;
#19269 = EDGE_LOOP ( 'NONE', ( #10585, #52018, #4776, #10374 ) ) ;
#19270 = AXIS2_PLACEMENT_3D ( 'NONE', #19356, #47223, #35368 ) ;
#19271 = CARTESIAN_POINT ( 'NONE',  ( -155.9608607592036833, -177.1207230881787780, 63.81752780153064464 ) ) ;
#19272 = PLANE ( 'NONE',  #37345 ) ;
#19273 = LINE ( 'NONE', #42905, #11481 ) ;
#19274 = ADVANCED_FACE ( 'NONE', ( #40819 ), #1137, .T. ) ;
#19275 = EDGE_CURVE ( 'NONE', #31327, #25704, #27398, .T. ) ;
#19276 = LINE ( 'NONE', #4528, #33833 ) ;
#19277 = EDGE_CURVE ( 'NONE', #21480, #12830, #5108, .T. ) ;
#19278 = CARTESIAN_POINT ( 'NONE',  ( -159.8192355313504720, -193.5000000000000000, -56.81883646197830018 ) ) ;
#19279 = DIRECTION ( 'NONE',  ( 0.000000000000000000, 0.000000000000000000, -1.000000000000000000 ) ) ;
#19281 = ORIENTED_EDGE ( 'NONE', *, *, #5502, .F. ) ;
#19280 = DIRECTION ( 'NONE',  ( 0.9266896074318317078, 0.000000000000000000, 0.3758275821142421647 ) ) ;
#19282 = EDGE_CURVE ( 'NONE', #16977, #28018, #12963, .T. ) ;
#19283 = VERTEX_POINT ( 'NONE', #1408 ) ;
#19284 = CARTESIAN_POINT ( 'NONE',  ( -330.4913330509368166, -123.5000000000000284, 0.000000000000000000 ) ) ;
#19285 = EDGE_CURVE ( 'NONE', #46248, #36451, #28471, .T. ) ;
#19286 = AXIS2_PLACEMENT_3D ( 'NONE', #46965, #10946, #26965 ) ;
#19287 = CARTESIAN_POINT ( 'NONE',  ( -339.1964088526558498, -162.9984922102920848, 43.83057281297495678 ) ) ;
#19288 = ORIENTED_EDGE ( 'NONE', *, *, #24520, .F. ) ;
#19289 = VERTEX_POINT ( 'NONE', #25080 ) ;
#19290 = PLANE ( 'NONE',  #34053 ) ;
#19291 = ORIENTED_EDGE ( 'NONE', *, *, #9515, .F. ) ;
#19292 = CARTESIAN_POINT ( 'NONE',  ( -48.82732838694323618, -175.3837268820161057, -0.9374196611341184537 ) ) ;
#19293 = LINE ( 'NONE', #26382, #23324 ) ;
#19294 = LINE ( 'NONE', #7194, #25288 ) ;
#19295 = CARTESIAN_POINT ( 'NONE',  ( -164.2512865680372727, -175.3837268820161057, -47.13604789772046644 ) ) ;
#19296 = EDGE_LOOP ( 'NONE', ( #16165, #10718, #35579, #42822 ) ) ;
#19297 = ORIENTED_EDGE ( 'NONE', *, *, #2266, .F. ) ;
#19298 = ORIENTED_EDGE ( 'NONE', *, *, #1794, .F. ) ;
#19299 = EDGE_CURVE ( 'NONE', #20926, #7384, #12281, .T. ) ;
#19300 = DIRECTION ( 'NONE',  ( 0.000000000000000000, -1.000000000000000000, 0.000000000000000000 ) ) ;
#19301 = PLANE ( 'NONE',  #15125 ) ;
#19302 = FACE_OUTER_BOUND ( 'NONE', #10745, .T. ) ;
#19303 = CIRCLE ( 'NONE', #48675, 125.0000000000000000 ) ;
#19304 = FACE_OUTER_BOUND ( 'NONE', #10189, .T. ) ;
#19305 = CARTESIAN_POINT ( 'NONE',  ( -164.0008810331606526, -189.7472609257535510, 47.74645837849825369 ) ) ;
#19306 = ORIENTED_EDGE ( 'NONE', *, *, #48094, .T. ) ;
#19307 = LINE ( 'NONE', #39756, #50015 ) ;
#19308 = ORIENTED_EDGE ( 'NONE', *, *, #17683, .T. ) ;
#19309 = ORIENTED_EDGE ( 'NONE', *, *, #23406, .F. ) ;
#19310 = PLANE ( 'NONE',  #5468 ) ;
#19311 = CARTESIAN_POINT ( 'NONE',  ( -123.4791267515088435, -173.5000000000000284, 70.00000000000000000 ) ) ;
#19312 = VERTEX_POINT ( 'NONE', #20875 ) ;
#19313 = DIRECTION ( 'NONE',  ( -0.000000000000000000, 0.1205366802553337752, 0.9927088740980526405 ) ) ;
#19314 = CARTESIAN_POINT ( 'NONE',  ( -336.3521761649654422, -179.2447759217480154, -19.39547174791710660 ) ) ;
#19315 = EDGE_CURVE ( 'NONE', #31987, #3363, #34131, .T. ) ;
#19317 = ADVANCED_FACE ( 'NONE', ( #41092 ), #884, .F. ) ;
#19316 = DIRECTION ( 'NONE',  ( 0.000000000000000000, 0.000000000000000000, -1.000000000000000000 ) ) ;
#19318 = EDGE_LOOP ( 'NONE', ( #22875, #25760, #22426, #1462 ) ) ;
#19319 = CARTESIAN_POINT ( 'NONE',  ( 76.04209377433248562, -193.5000000000000000, -10.93003379476866677 ) ) ;
#19320 = AXIS2_PLACEMENT_3D ( 'NONE', #42424, #37964, #10366 ) ;
#19321 = AXIS2_PLACEMENT_3D ( 'NONE', #50558, #14299, #38191 ) ;
#19322 = VERTEX_POINT ( 'NONE', #33481 ) ;
#19323 = CARTESIAN_POINT ( 'NONE',  ( -490.0000000000001137, -168.5000000000000284, 0.000000000000000000 ) ) ;
#19324 = DIRECTION ( 'NONE',  ( 0.000000000000000000, 0.000000000000000000, 1.000000000000000000 ) ) ;
#19325 = ORIENTED_EDGE ( 'NONE', *, *, #26989, .T. ) ;
#19326 = FACE_OUTER_BOUND ( 'NONE', #50106, .T. ) ;
#19327 = CARTESIAN_POINT ( 'NONE',  ( 1.734723475976807094E-15, 20.00000000000000000, 46.00000000000000711 ) ) ;
#19328 = DIRECTION ( 'NONE',  ( -1.000000000000000000, 6.921107616850842615E-15, 7.812315528781815670E-15 ) ) ;
#19329 = LINE ( 'NONE', #47438, #19035 ) ;
#19330 = DIRECTION ( 'NONE',  ( 0.000000000000000000, 0.000000000000000000, -1.000000000000000000 ) ) ;
#19331 = ORIENTED_EDGE ( 'NONE', *, *, #39737, .T. ) ;
#19332 = VERTEX_POINT ( 'NONE', #28217 ) ;
#19333 = AXIS2_PLACEMENT_3D ( 'NONE', #31750, #11246, #27789 ) ;
#19334 = EDGE_CURVE ( 'NONE', #42991, #37560, #51772, .T. ) ;
#19335 = DIRECTION ( 'NONE',  ( -0.000000000000000000, 0.5680647467311656929, 0.8229838658936495799 ) ) ;
#19337 = ORIENTED_EDGE ( 'NONE', *, *, #48870, .F. ) ;
#19336 = CARTESIAN_POINT ( 'NONE',  ( -133.8011377042516301, -183.6283474603465606, -91.35181687837437892 ) ) ;
#19338 = VERTEX_POINT ( 'NONE', #22680 ) ;
#19339 = CARTESIAN_POINT ( 'NONE',  ( 67.42090074966655777, -193.5000000000000000, -46.82076062204441058 ) ) ;
#19340 = EDGE_CURVE ( 'NONE', #9665, #17851, #21907, .T. ) ;
#19341 = CARTESIAN_POINT ( 'NONE',  ( -339.1964088526558498, -96.52406086224443982, -52.47426709956138069 ) ) ;
#19342 = ORIENTED_EDGE ( 'NONE', *, *, #30773, .T. ) ;
#19343 = DIRECTION ( 'NONE',  ( -0.000000000000000000, 1.000000000000000000, -0.000000000000000000 ) ) ;
#19344 = DIRECTION ( 'NONE',  ( -0.000000000000000000, 1.000000000000000000, -0.000000000000000000 ) ) ;
#19345 = ORIENTED_EDGE ( 'NONE', *, *, #24963, .T. ) ;
#19346 = DIRECTION ( 'NONE',  ( 0.000000000000000000, 0.000000000000000000, 1.000000000000000000 ) ) ;
#19347 = CARTESIAN_POINT ( 'NONE',  ( 60.00000000000000000, -63.50000000000000000, -60.00000000000000711 ) ) ;
#19348 = DIRECTION ( 'NONE',  ( 0.000000000000000000, 1.000000000000000000, 0.000000000000000000 ) ) ;
#19349 = ORIENTED_EDGE ( 'NONE', *, *, #43874, .F. ) ;
#19350 = ORIENTED_EDGE ( 'NONE', *, *, #30108, .F. ) ;
#19351 = VECTOR ( 'NONE', #43652, 1000.000000000000227 ) ;
#19353 = ORIENTED_EDGE ( 'NONE', *, *, #45281, .T. ) ;
#19352 = AXIS2_PLACEMENT_3D ( 'NONE', #13965, #18684, #29721 ) ;
#19354 = PLANE ( 'NONE',  #11645 ) ;
#19355 = DIRECTION ( 'NONE',  ( 0.000000000000000000, 0.8854560256532078011, -0.4647231720437724478 ) ) ;
#19356 = CARTESIAN_POINT ( 'NONE',  ( 0.000000000000000000, -71.25809448646064936, -27.41866715058241866 ) ) ;
#19357 = CARTESIAN_POINT ( 'NONE',  ( -171.6469053867624837, -183.6283474603465606, -14.34663989163548514 ) ) ;
#19358 = CARTESIAN_POINT ( 'NONE',  ( -332.3517673607765914, -63.76276212672765809, 5.609136410542459039 ) ) ;
#19359 = EDGE_LOOP ( 'NONE', ( #46236, #5220, #39551, #39953 ) ) ;
#19360 = DIRECTION ( 'NONE',  ( 0.000000000000000000, -0.3546048870425235200, 0.9350162426854194964 ) ) ;
#19361 = ORIENTED_EDGE ( 'NONE', *, *, #5959, .T. ) ;
#19363 = VERTEX_POINT ( 'NONE', #6400 ) ;
#19362 = CARTESIAN_POINT ( 'NONE',  ( -332.3517673607765914, -65.82380048139334860, 12.53476669029061519 ) ) ;
#19364 = ORIENTED_EDGE ( 'NONE', *, *, #45271, .F. ) ;
#19365 = VECTOR ( 'NONE', #389, 1000.000000000000114 ) ;
#19366 = CARTESIAN_POINT ( 'NONE',  ( -170.8336150310144887, -193.5000000000000000, 25.58083653558494319 ) ) ;
#19367 = DIRECTION ( 'NONE',  ( -0.9027978299657446470, 0.000000000000000000, 0.4300652022765183435 ) ) ;
#19368 = CYLINDRICAL_SURFACE ( 'NONE', #34696, 124.9999999999999858 ) ;
#19369 = EDGE_CURVE ( 'NONE', #9644, #9613, #6144, .T. ) ;
#19370 = LINE ( 'NONE', #19882, #51117 ) ;
#19371 = ORIENTED_EDGE ( 'NONE', *, *, #39545, .T. ) ;
#19372 = CARTESIAN_POINT ( 'NONE',  ( -11.17913199888832843, -193.5000000000000000, 119.3051146910914326 ) ) ;
#19373 = EDGE_LOOP ( 'NONE', ( #31446, #37903, #44913, #20329 ) ) ;
#19374 = VERTEX_POINT ( 'NONE', #38175 ) ;
#19375 = CARTESIAN_POINT ( 'NONE',  ( -170.7635349987907603, -193.5000000000000000, -25.91377046305877130 ) ) ;
#19376 = LINE ( 'NONE', #4572, #51630 ) ;
#19377 = DIRECTION ( 'NONE',  ( -0.9960498426152158968, 0.000000000000000000, -0.08879589532294571153 ) ) ;
#19378 = DIRECTION ( 'NONE',  ( -8.718379230999707126E-17, -0.4647231720437755564, -0.8854560256532062468 ) ) ;
#19379 = VECTOR ( 'NONE', #43621, 1000.000000000000000 ) ;
#19380 = DIRECTION ( 'NONE',  ( -0.9842305779475992722, 0.000000000000000000, 0.1768902751225592818 ) ) ;
#19381 = DIRECTION ( 'NONE',  ( -0.000000000000000000, 1.000000000000000000, -0.000000000000000000 ) ) ;
#19382 = EDGE_LOOP ( 'NONE', ( #45076, #1371, #40195, #8287 ) ) ;
#19383 = FACE_OUTER_BOUND ( 'NONE', #43841, .T. ) ;
#19384 = DIRECTION ( 'NONE',  ( 0.8610436117673514467, 0.000000000000000000, 0.5085311186492273983 ) ) ;
#19385 = AXIS2_PLACEMENT_3D ( 'NONE', #51785, #15516, #39411 ) ;
#19386 = CARTESIAN_POINT ( 'NONE',  ( -171.9128728525929262, -175.3837268820161057, 11.83705339977325011 ) ) ;
#19387 = ORIENTED_EDGE ( 'NONE', *, *, #41, .F. ) ;
#19388 = EDGE_CURVE ( 'NONE', #3747, #34815, #17968, .T. ) ;
#19389 = DIRECTION ( 'NONE',  ( -0.000000000000000000, 1.000000000000000000, -0.000000000000000000 ) ) ;
#19390 = CYLINDRICAL_SURFACE ( 'NONE', #27798, 25.00456841203573077 ) ;
#19391 = ORIENTED_EDGE ( 'NONE', *, *, #38603, .F. ) ;
#19392 = FACE_OUTER_BOUND ( 'NONE', #20321, .T. ) ;
#19393 = EDGE_LOOP ( 'NONE', ( #23992, #44077, #5066, #3546, #9528, #43061 ) ) ;
#19394 = CARTESIAN_POINT ( 'NONE',  ( 68.21542617880035664, -193.5000000000000000, 41.93543928473692972 ) ) ;
#19395 = VECTOR ( 'NONE', #13470, 1000.000000000000000 ) ;
#19396 = FACE_BOUND ( 'NONE', #1065, .T. ) ;
#19397 = LINE ( 'NONE', #30968, #17859 ) ;
#19398 = CARTESIAN_POINT ( 'NONE',  ( 58.45385938022562300, -193.5000000000000000, 62.78108192022012446 ) ) ;
#19399 = VERTEX_POINT ( 'NONE', #29516 ) ;
#19400 = VERTEX_POINT ( 'NONE', #45570 ) ;
#19401 = CARTESIAN_POINT ( 'NONE',  ( -305.0000000000000568, -99.78295912235451226, 55.11353710303931308 ) ) ;
#19402 = ORIENTED_EDGE ( 'NONE', *, *, #52011, .T. ) ;
#19403 = CARTESIAN_POINT ( 'NONE',  ( -339.1964088526558498, -124.0000000000002700, -59.00000000000002132 ) ) ;
#19404 = AXIS2_PLACEMENT_3D ( 'NONE', #371, #9319, #36910 ) ;
#19405 = EDGE_CURVE ( 'NONE', #47822, #51761, #1417, .T. ) ;
#19406 = VECTOR ( 'NONE', #33290, 1000.000000000000000 ) ;
#19407 = EDGE_CURVE ( 'NONE', #3041, #42991, #10586, .T. ) ;
#19408 = DIRECTION ( 'NONE',  ( 0.000000000000000000, 0.000000000000000000, 1.000000000000000000 ) ) ;
#19409 = ORIENTED_EDGE ( 'NONE', *, *, #48138, .F. ) ;
#19412 = VERTEX_POINT ( 'NONE', #37673 ) ;
#19411 = SURFACE_SIDE_STYLE ('',( #18898 ) ) ;
#19410 = CARTESIAN_POINT ( 'NONE',  ( -336.3521761649654422, -166.6218737817864621, 41.71934804797023588 ) ) ;
#19413 = LINE ( 'NONE', #50982, #5566 ) ;
#19414 = ORIENTED_EDGE ( 'NONE', *, *, #22584, .T. ) ;
#19415 = FACE_OUTER_BOUND ( 'NONE', #38672, .T. ) ;
#19416 = ORIENTED_EDGE ( 'NONE', *, *, #28865, .T. ) ;
#19417 = EDGE_CURVE ( 'NONE', #28664, #15304, #5630, .T. ) ;
#19418 = FACE_OUTER_BOUND ( 'NONE', #28586, .T. ) ;
#19419 = ORIENTED_EDGE ( 'NONE', *, *, #10349, .T. ) ;
#19421 = DIRECTION ( 'NONE',  ( 0.000000000000000000, 1.000000000000000000, 0.000000000000000000 ) ) ;
#19420 = DIRECTION ( 'NONE',  ( -0.9564009842765223146, 0.000000000000000000, -0.2920567706369764371 ) ) ;
#19422 = VERTEX_POINT ( 'NONE', #22425 ) ;
#19423 = VECTOR ( 'NONE', #35095, 1000.000000000000000 ) ;
#19424 = EDGE_CURVE ( 'NONE', #25561, #45202, #6660, .T. ) ;
#19425 = CARTESIAN_POINT ( 'NONE',  ( -155.4465502054561057, -183.6283474603465606, 64.67588669375881238 ) ) ;
#19426 = EDGE_LOOP ( 'NONE', ( #2304, #13533, #37084, #11584 ) ) ;
#19427 = DIRECTION ( 'NONE',  ( -0.2348860457809775482, 0.000000000000000000, -0.9720229140804121926 ) ) ;
#19428 = EDGE_CURVE ( 'NONE', #4116, #11641, #33979, .T. ) ;
#19430 = AXIS2_PLACEMENT_3D ( 'NONE', #43462, #18764, #30854 ) ;
#19429 = CYLINDRICAL_SURFACE ( 'NONE', #42471, 4.000000000000003553 ) ;
#19431 = DIRECTION ( 'NONE',  ( -0.000000000000000000, 1.000000000000000000, -0.000000000000000000 ) ) ;
#19432 = CARTESIAN_POINT ( 'NONE',  ( -339.1964088526558498, -163.6602333390102331, -44.57752413667962088 ) ) ;
#19433 = DIRECTION ( 'NONE',  ( 0.9890401873221633666, 0.000000000000000000, 0.1476465640024850756 ) ) ;
#19434 = PLANE ( 'NONE',  #49916 ) ;
#19435 = VERTEX_POINT ( 'NONE', #10077 ) ;
#19436 = CARTESIAN_POINT ( 'NONE',  ( 55.35935253854128746, -193.5000000000000000, 69.58857822035042773 ) ) ;
#19437 = DIRECTION ( 'NONE',  ( 0.9995608365087942371, 0.000000000000000000, 0.02963332782256331357 ) ) ;
#19438 = LINE ( 'NONE', #38893, #22919 ) ;
#19439 = ORIENTED_EDGE ( 'NONE', *, *, #30601, .F. ) ;
#19440 = FACE_OUTER_BOUND ( 'NONE', #14167, .T. ) ;
#19441 = DIRECTION ( 'NONE',  ( 0.000000000000000000, 0.000000000000000000, -1.000000000000000000 ) ) ;
#19442 = ADVANCED_FACE ( 'NONE', ( #30550 ), #25572, .F. ) ;
#19443 = VECTOR ( 'NONE', #29193, 1000.000000000000000 ) ;
#19444 = LINE ( 'NONE', #39917, #40329 ) ;
#19446 = ORIENTED_EDGE ( 'NONE', *, *, #30379, .T. ) ;
#19445 = DIRECTION ( 'NONE',  ( -0.000000000000000000, -0.000000000000000000, 1.000000000000000000 ) ) ;
#19447 = VERTEX_POINT ( 'NONE', #14544 ) ;
#19448 = AXIS2_PLACEMENT_3D ( 'NONE', #37984, #30605, #2761 ) ;
#19449 = ORIENTED_EDGE ( 'NONE', *, *, #15598, .F. ) ;
#19450 = CIRCLE ( 'NONE', #25313, 125.0000000000000000 ) ;
#19451 = CARTESIAN_POINT ( 'NONE',  ( -330.4913330509368166, -138.1050951016783301, 57.16590939599346655 ) ) ;
#19452 = PLANE ( 'NONE',  #16991 ) ;
#19453 = CARTESIAN_POINT ( 'NONE',  ( -46.00000000000000711, 0.000000000000000000, -46.00000000000000000 ) ) ;
#19454 = CARTESIAN_POINT ( 'NONE',  ( -68.21229068036657850, -177.1207230881787780, -123.4325817657429809 ) ) ;
#19455 = ORIENTED_EDGE ( 'NONE', *, *, #8061, .F. ) ;
#19456 = CARTESIAN_POINT ( 'NONE',  ( 2.958066673514105016, 57.09730180201670180, -16.88239234222090701 ) ) ;
#19457 = ORIENTED_EDGE ( 'NONE', *, *, #32333, .T. ) ;
#19458 = AXIS2_PLACEMENT_3D ( 'NONE', #17075, #28867, #44916 ) ;
#19459 = ORIENTED_EDGE ( 'NONE', *, *, #28824, .F. ) ;
#19460 = VECTOR ( 'NONE', #33822, 1000.000000000000000 ) ;
#19461 = ORIENTED_EDGE ( 'NONE', *, *, #32750, .F. ) ;
#19462 = CARTESIAN_POINT ( 'NONE',  ( -136.1415351158078693, -175.3837268820161057, -89.10837311819173578 ) ) ;
#19463 = EDGE_CURVE ( 'NONE', #17942, #42649, #26094, .T. ) ;
#19464 = ADVANCED_FACE ( 'NONE', ( #13502 ), #17715, .F. ) ;
#19465 = CARTESIAN_POINT ( 'NONE',  ( -140.5933766095837427, -193.5000000000000000, -84.49831343337065448 ) ) ;
#19466 = VERTEX_POINT ( 'NONE', #34750 ) ;
#19467 = PRESENTATION_STYLE_ASSIGNMENT (( #15811 ) ) ;
#19468 = DIRECTION ( 'NONE',  ( -0.000000000000000000, 0.7485107481711024136, 0.6631226582407937498 ) ) ;
#19471 = EDGE_LOOP ( 'NONE', ( #10042, #48706, #12027, #40518 ) ) ;
#19470 = DIRECTION ( 'NONE',  ( 0.000000000000000000, 0.000000000000000000, -1.000000000000000000 ) ) ;
#19469 = CARTESIAN_POINT ( 'NONE',  ( -141.2664123866436512, -175.3837268820161057, -83.75869879877495805 ) ) ;
#19472 = DIRECTION ( 'NONE',  ( 1.000000000000000000, 0.000000000000000000, 0.000000000000000000 ) ) ;
#19473 = ORIENTED_EDGE ( 'NONE', *, *, #13833, .T. ) ;
#19474 = DIRECTION ( 'NONE',  ( 0.000000000000000000, 0.000000000000000000, 1.000000000000000000 ) ) ;
#19475 = VECTOR ( 'NONE', #3399, 999.9999999999998863 ) ;
#19476 = ORIENTED_EDGE ( 'NONE', *, *, #2368, .F. ) ;
#19477 = DIRECTION ( 'NONE',  ( -0.000000000000000000, 0.000000000000000000, -1.000000000000000000 ) ) ;
#19478 = EDGE_CURVE ( 'NONE', #50728, #5823, #13760, .T. ) ;
#19479 = FACE_OUTER_BOUND ( 'NONE', #4221, .T. ) ;
#19481 = DIRECTION ( 'NONE',  ( 0.000000000000000000, 1.000000000000000000, -0.000000000000000000 ) ) ;
#19480 = DIRECTION ( 'NONE',  ( -0.000000000000000000, 1.000000000000000000, 0.000000000000000000 ) ) ;
#19482 = ORIENTED_EDGE ( 'NONE', *, *, #42625, .F. ) ;
#19483 = EDGE_CURVE ( 'NONE', #24129, #12564, #30298, .T. ) ;
#19484 = VECTOR ( 'NONE', #13395, 1000.000000000000000 ) ;
#19485 = CARTESIAN_POINT ( 'NONE',  ( 0.000000000000000000, -96.08133284941780516, -52.24190551353947143 ) ) ;
#19486 = LINE ( 'NONE', #10839, #12190 ) ;
#19487 = EDGE_CURVE ( 'NONE', #46212, #51398, #2285, .T. ) ;
#19488 = DIRECTION ( 'NONE',  ( 0.000000000000000000, 0.8854560256532078011, -0.4647231720437724478 ) ) ;
#19489 = VERTEX_POINT ( 'NONE', #29771 ) ;
#19490 = DIRECTION ( 'NONE',  ( 0.000000000000000000, 0.000000000000000000, 1.000000000000000000 ) ) ;
#19491 = CARTESIAN_POINT ( 'NONE',  ( -41.96187976958284338, -193.5000000000000000, -123.8286356280830205 ) ) ;
#19492 = EDGE_CURVE ( 'NONE', #33439, #20384, #9817, .T. ) ;
#19493 = VERTEX_POINT ( 'NONE', #50543 ) ;
#19494 = DIRECTION ( 'NONE',  ( -0.000000000000000000, 0.7485107481711089639, 0.6631226582407863113 ) ) ;
#19495 = AXIS2_PLACEMENT_3D ( 'NONE', #6862, #46555, #15265 ) ;
#19497 = AXIS2_PLACEMENT_3D ( 'NONE', #41658, #42171, #6194 ) ;
#19496 = DIRECTION ( 'NONE',  ( 1.043714542225393539E-14, 0.1205366802553095307, -0.9927088740980556381 ) ) ;
#19498 = ORIENTED_EDGE ( 'NONE', *, *, #44416, .F. ) ;
#19499 = DIRECTION ( 'NONE',  ( -0.5829794791144820021, 0.000000000000000000, 0.8124868780056742068 ) ) ;
#19500 = EDGE_LOOP ( 'NONE', ( #45582, #45456, #48409, #41600 ) ) ;
#19501 = VECTOR ( 'NONE', #28800, 1000.000000000000000 ) ;
#19502 = AXIS2_PLACEMENT_3D ( 'NONE', #27423, #43471, #27685 ) ;
#19503 = FACE_OUTER_BOUND ( 'NONE', #5118, .T. ) ;
#19504 = LINE ( 'NONE', #31858, #34560 ) ;
#19505 = DIRECTION ( 'NONE',  ( 0.000000000000000000, 0.000000000000000000, 1.000000000000000000 ) ) ;
#19506 = DIRECTION ( 'NONE',  ( -0.000000000000000000, 1.000000000000000000, -0.000000000000000000 ) ) ;
#19507 = CARTESIAN_POINT ( 'NONE',  ( 69.66827051661184100, -193.5000000000000000, -40.81902153125260213 ) ) ;
#19508 = DIRECTION ( 'NONE',  ( 1.000000000000000000, -0.000000000000000000, -0.000000000000000000 ) ) ;
#19509 = DIRECTION ( 'NONE',  ( -0.000000000000000000, 1.000000000000000000, -0.000000000000000000 ) ) ;
#19510 = DIRECTION ( 'NONE',  ( -0.000000000000000000, -0.5680647467311485954, 0.8229838658936613482 ) ) ;
#19512 = ORIENTED_EDGE ( 'NONE', *, *, #24102, .F. ) ;
#19511 = DIRECTION ( 'NONE',  ( -0.000000000000000000, 1.000000000000000000, -0.000000000000000000 ) ) ;
#19513 = VECTOR ( 'NONE', #20994, 1000.000000000000000 ) ;
#19514 = EDGE_LOOP ( 'NONE', ( #4601, #35877, #46739, #43915 ) ) ;
#19515 = DIRECTION ( 'NONE',  ( 0.000000000000000000, 0.000000000000000000, 1.000000000000000000 ) ) ;
#19516 = EDGE_CURVE ( 'NONE', #19986, #32415, #31643, .T. ) ;
#19517 = DIRECTION ( 'NONE',  ( 0.000000000000000000, 0.000000000000000000, 1.000000000000000000 ) ) ;
#19518 = ORIENTED_EDGE ( 'NONE', *, *, #32956, .T. ) ;
#19519 = ORIENTED_EDGE ( 'NONE', *, *, #11512, .F. ) ;
#19520 = CARTESIAN_POINT ( 'NONE',  ( 69.25251857196690253, -175.3837268820161057, 38.92640747825683434 ) ) ;
#19521 = ORIENTED_EDGE ( 'NONE', *, *, #20275, .T. ) ;
#19522 = CYLINDRICAL_SURFACE ( 'NONE', #15829, 125.0000000000000000 ) ;
#19523 = LINE ( 'NONE', #43707, #51055 ) ;
#19524 = ADVANCED_FACE ( 'NONE', ( #31070 ), #14803, .F. ) ;
#19525 = EDGE_CURVE ( 'NONE', #42477, #11058, #51842, .T. ) ;
#19526 = ADVANCED_FACE ( 'NONE', ( #35520 ), #31326, .F. ) ;
#19527 = CARTESIAN_POINT ( 'NONE',  ( 5.015379008610418410, -177.1207230881787780, -112.9749434763326690 ) ) ;
#19528 = DIRECTION ( 'NONE',  ( -1.000000000000000000, 0.000000000000000000, 0.000000000000000000 ) ) ;
#19529 = ORIENTED_EDGE ( 'NONE', *, *, #37821, .T. ) ;
#19530 = AXIS2_PLACEMENT_3D ( 'NONE', #33298, #29347, #21988 ) ;
#19531 = ORIENTED_EDGE ( 'NONE', *, *, #1061, .T. ) ;
#19532 = EDGE_CURVE ( 'NONE', #27011, #44148, #47639, .T. ) ;
#19533 = ORIENTED_EDGE ( 'NONE', *, *, #20373, .F. ) ;
#19534 = DIRECTION ( 'NONE',  ( 0.5085311186492154079, 0.000000000000000000, 0.8610436117673585521 ) ) ;
#19535 = CARTESIAN_POINT ( 'NONE',  ( -118.1688136093591908, -175.3837268820161057, -103.7706487676296661 ) ) ;
#19536 = AXIS2_PLACEMENT_3D ( 'NONE', #10925, #23786, #15916 ) ;
#19537 = DIRECTION ( 'NONE',  ( 0.000000000000000000, -0.9709418174260519008, 0.2393156642875582940 ) ) ;
#19538 = VECTOR ( 'NONE', #38187, 1000.000000000000000 ) ;
#19539 = EDGE_CURVE ( 'NONE', #16914, #45874, #32475, .T. ) ;
#19540 = CARTESIAN_POINT ( 'NONE',  ( 51.05451324771860300, -177.1207230881787780, 75.61781872352698031 ) ) ;
#19541 = FACE_OUTER_BOUND ( 'NONE', #13907, .T. ) ;
#19542 = ORIENTED_EDGE ( 'NONE', *, *, #35982, .F. ) ;
#19543 = FACE_OUTER_BOUND ( 'NONE', #22857, .T. ) ;
#19544 = PRODUCT_DEFINITION_CONTEXT ( 'detailed design', #8183, 'design' ) ;
#19545 = CIRCLE ( 'NONE', #50586, 125.0000000000000000 ) ;
#19546 = EDGE_CURVE ( 'NONE', #50678, #9782, #35018, .T. ) ;
#19547 = LINE ( 'NONE', #47931, #23957 ) ;
#19548 = DIRECTION ( 'NONE',  ( -1.000000000000000000, 0.000000000000000000, 0.000000000000000000 ) ) ;
#19549 = EDGE_CURVE ( 'NONE', #16711, #25060, #38358, .T. ) ;
#19550 = ORIENTED_EDGE ( 'NONE', *, *, #13571, .T. ) ;
#19551 = ORIENTED_EDGE ( 'NONE', *, *, #38525, .F. ) ;
#19552 = VERTEX_POINT ( 'NONE', #46868 ) ;
#19553 = CARTESIAN_POINT ( 'NONE',  ( -332.3517673607765914, -118.8878589706978914, -59.82247199109903590 ) ) ;
#19554 = EDGE_CURVE ( 'NONE', #11654, #28777, #43679, .T. ) ;
#19555 = CARTESIAN_POINT ( 'NONE',  ( -336.3521761649654422, -71.64707600775140861, -30.18731974611341684 ) ) ;
#19556 = ORIENTED_EDGE ( 'NONE', *, *, #8632, .F. ) ;
#19557 = CARTESIAN_POINT ( 'NONE',  ( -66.64622755927948106, -177.1207230881787780, 123.6727797384707515 ) ) ;
#19558 = VECTOR ( 'NONE', #44339, 1000.000000000000000 ) ;
#19559 = ADVANCED_FACE ( 'NONE', ( #11625 ), #15842, .T. ) ;
#19560 = DIRECTION ( 'NONE',  ( 0.000000000000000000, -0.9350162426854107256, 0.3546048870425463906 ) ) ;
#19561 = CARTESIAN_POINT ( 'NONE',  ( -145.2888470698896981, -189.7472609257535510, -77.48473115145237955 ) ) ;
#19562 = ORIENTED_EDGE ( 'NONE', *, *, #33469, .T. ) ;
#19563 = CARTESIAN_POINT ( 'NONE',  ( -339.1964088526558498, -123.0000000000002700, -59.00000000000002132 ) ) ;
#19564 = EDGE_CURVE ( 'NONE', #48223, #39946, #2958, .T. ) ;
#19565 = VECTOR ( 'NONE', #37698, 1000.000000000000227 ) ;
#19566 = ORIENTED_EDGE ( 'NONE', *, *, #5746, .T. ) ;
#19567 = CARTESIAN_POINT ( 'NONE',  ( -332.3517673607765914, -123.5000000000000284, 0.000000000000000000 ) ) ;
#19568 = DIRECTION ( 'NONE',  ( 0.6749830015182142207, 0.000000000000000000, -0.7378332790417239107 ) ) ;
#19569 = ORIENTED_EDGE ( 'NONE', *, *, #11768, .F. ) ;
#19570 = CYLINDRICAL_SURFACE ( 'NONE', #9751, 125.0000000000000000 ) ;
#19571 = DIRECTION ( 'NONE',  ( 0.000000000000000000, 0.000000000000000000, -1.000000000000000000 ) ) ;
#19572 = CARTESIAN_POINT ( 'NONE',  ( -151.9915035862630646, -193.5000000000000000, 70.07273251429430161 ) ) ;
#19573 = AXIS2_PLACEMENT_3D ( 'NONE', #14229, #18426, #2118 ) ;
#19574 = DIRECTION ( 'NONE',  ( -1.000000000000000000, 1.043714542225393381E-14, -1.093232954177749459E-28 ) ) ;
#19575 = AXIS2_PLACEMENT_3D ( 'NONE', #31158, #42740, #10678 ) ;
#19576 = EDGE_CURVE ( 'NONE', #14462, #30271, #35271, .T. ) ;
#19577 = DIRECTION ( 'NONE',  ( -1.000000000000000000, 0.000000000000000000, 0.000000000000000000 ) ) ;
#19578 = VERTEX_POINT ( 'NONE', #50803 ) ;
#19579 = ORIENTED_EDGE ( 'NONE', *, *, #9348, .F. ) ;
#19580 = CIRCLE ( 'NONE', #50615, 125.0000000000000000 ) ;
#19581 = LINE ( 'NONE', #48498, #4305 ) ;
#19583 = ORIENTED_EDGE ( 'NONE', *, *, #4295, .F. ) ;
#19582 = FACE_OUTER_BOUND ( 'NONE', #1579, .T. ) ;
#19584 = EDGE_LOOP ( 'NONE', ( #26270, #26843, #25435, #1197 ) ) ;
#19585 = DIRECTION ( 'NONE',  ( -0.4031234292879730674, 0.000000000000000000, 0.9151456172430181280 ) ) ;
#19586 = AXIS2_PLACEMENT_3D ( 'NONE', #9636, #29859, #29343 ) ;
#19587 = CARTESIAN_POINT ( 'NONE',  ( -336.3521761649654422, -181.7525362123217292, 9.724760635742144999 ) ) ;
#19588 = ORIENTED_EDGE ( 'NONE', *, *, #41392, .F. ) ;
#19589 = LINE ( 'NONE', #23793, #44411 ) ;
#19590 = DIRECTION ( 'NONE',  ( 0.000000000000000000, 0.000000000000000000, -1.000000000000000000 ) ) ;
#19591 = EDGE_LOOP ( 'NONE', ( #6425, #6465, #15334, #50362 ) ) ;
#19592 = CARTESIAN_POINT ( 'NONE',  ( -330.4913330509368166, -130.2355952558269507, -59.62073260661665586 ) ) ;
#19593 = FACE_OUTER_BOUND ( 'NONE', #50576, .T. ) ;
#19594 = AXIS2_PLACEMENT_3D ( 'NONE', #41280, #6077, #25517 ) ;
#19595 = ADVANCED_FACE ( 'NONE', ( #10850 ), #47371, .T. ) ;
#19596 = EDGE_CURVE ( 'NONE', #32204, #50157, #43933, .T. ) ;
#19597 = LINE ( 'NONE', #30634, #20223 ) ;
#19598 = CARTESIAN_POINT ( 'NONE',  ( -330.4913330509368166, -137.1341532842523918, 57.40522506028099770 ) ) ;
#19599 = ORIENTED_EDGE ( 'NONE', *, *, #46315, .F. ) ;
#19600 = ORIENTED_EDGE ( 'NONE', *, *, #27276, .T. ) ;
#19601 = VECTOR ( 'NONE', #29650, 1000.000000000000000 ) ;
#19602 = ADVANCED_FACE ( 'NONE', ( #27651 ), #43157, .F. ) ;
#19603 = ORIENTED_EDGE ( 'NONE', *, *, #49912, .F. ) ;
#19604 = ADVANCED_FACE ( 'NONE', ( #7163 ), #3726, .F. ) ;
#19605 = DIRECTION ( 'NONE',  ( 0.9027978299657416494, 0.000000000000000000, 0.4300652022765245608 ) ) ;
#19606 = FACE_OUTER_BOUND ( 'NONE', #17863, .T. ) ;
#19607 = FACE_OUTER_BOUND ( 'NONE', #28701, .T. ) ;
#19608 = DIRECTION ( 'NONE',  ( 0.000000000000000000, 1.000000000000000000, 0.000000000000000000 ) ) ;
#19609 = CARTESIAN_POINT ( 'NONE',  ( 72.31641062551800303, -193.5000000000000000, 32.14713283941990341 ) ) ;
#19610 = ORIENTED_EDGE ( 'NONE', *, *, #16722, .T. ) ;
#19611 = VECTOR ( 'NONE', #18210, 1000.000000000000000 ) ;
#19612 = CARTESIAN_POINT ( 'NONE',  ( -180.0000000000000568, -115.7896721143442278, 60.00000000000000711 ) ) ;
#19613 = ORIENTED_EDGE ( 'NONE', *, *, #43325, .T. ) ;
#19614 = FACE_OUTER_BOUND ( 'NONE', #39892, .T. ) ;
#19615 = VECTOR ( 'NONE', #37781, 1000.000000000000000 ) ;
#19616 = VERTEX_POINT ( 'NONE', #4001 ) ;
#19617 = EDGE_CURVE ( 'NONE', #23894, #39687, #9825, .T. ) ;
#19618 = CARTESIAN_POINT ( 'NONE',  ( 49.03269102277813829, 30.00000000000000355, -50.83217377521822300 ) ) ;
#19619 = PRODUCT_DEFINITION ( 'UNKNOWN', '', #29265, #3774 ) ;
#19620 = CARTESIAN_POINT ( 'NONE',  ( -36.15208382588832592, -183.6283474603465606, 123.3865623328509145 ) ) ;
#19621 = DIRECTION ( 'NONE',  ( 0.000000000000000000, -0.000000000000000000, -1.000000000000000000 ) ) ;
#19622 = CARTESIAN_POINT ( 'NONE',  ( -339.1964088526558498, -144.8891964568526305, -54.98865587491811624 ) ) ;
#19623 = ORIENTED_EDGE ( 'NONE', *, *, #9224, .T. ) ;
#19624 = PLANE ( 'NONE',  #35909 ) ;
#19625 = ORIENTED_EDGE ( 'NONE', *, *, #13849, .F. ) ;
#19626 = EDGE_CURVE ( 'NONE', #29948, #21402, #41702, .T. ) ;
#19627 = ORIENTED_EDGE ( 'NONE', *, *, #49427, .F. ) ;
#19628 = LINE ( 'NONE', #23331, #38836 ) ;
#19629 = FACE_OUTER_BOUND ( 'NONE', #8063, .T. ) ;
#19630 = DIRECTION ( 'NONE',  ( 0.9890401873221644768, 0.000000000000000000, -0.1476465640024779702 ) ) ;
#19631 = CARTESIAN_POINT ( 'NONE',  ( -330.4913330509368166, -75.22798428563987727, -33.92731199008506593 ) ) ;
#19632 = VECTOR ( 'NONE', #28355, 1000.000000000000000 ) ;
#19633 = CARTESIAN_POINT ( 'NONE',  ( -339.1964088526558498, -175.9742670995610752, 26.97593913775620678 ) ) ;
#19634 = FACE_OUTER_BOUND ( 'NONE', #40190, .T. ) ;
#19635 = DIRECTION ( 'NONE',  ( -0.000000000000000000, 1.000000000000000000, -0.000000000000000000 ) ) ;
#19636 = ORIENTED_EDGE ( 'NONE', *, *, #8160, .T. ) ;
#19637 = CARTESIAN_POINT ( 'NONE',  ( -75.31296732259117732, -193.5000000000000000, -121.0625654437172614 ) ) ;
#19638 = FACE_OUTER_BOUND ( 'NONE', #40612, .T. ) ;
#19639 = AXIS2_PLACEMENT_3D ( 'NONE', #15966, #4380, #12527 ) ;
#19640 = PLANE ( 'NONE',  #14826 ) ;
#19641 = VERTEX_POINT ( 'NONE', #20810 ) ;
#19642 = DIRECTION ( 'NONE',  ( 0.000000000000000000, -0.000000000000000000, 1.000000000000000000 ) ) ;
#19643 = DIRECTION ( 'NONE',  ( 0.000000000000000000, -0.7485107481710953081, 0.6631226582408016323 ) ) ;
#19644 = ORIENTED_EDGE ( 'NONE', *, *, #38414, .T. ) ;
#19645 = CARTESIAN_POINT ( 'NONE',  ( -330.4913330509368166, -123.5000000000000284, 0.000000000000000000 ) ) ;
#19646 = CIRCLE ( 'NONE', #1147, 125.0000000000000000 ) ;
#19647 = ORIENTED_EDGE ( 'NONE', *, *, #47245, .F. ) ;
#19648 = FACE_BOUND ( 'NONE', #10067, .T. ) ;
#19650 = VERTEX_POINT ( 'NONE', #828 ) ;
#19649 = CARTESIAN_POINT ( 'NONE',  ( 1.150725574412418739, -189.7472609257535510, -114.7252272087845881 ) ) ;
#19651 = EDGE_CURVE ( 'NONE', #14780, #25092, #29206, .T. ) ;
#19652 = DIRECTION ( 'NONE',  ( -0.000000000000000000, 1.000000000000000000, -0.000000000000000000 ) ) ;
#19653 = ORIENTED_EDGE ( 'NONE', *, *, #34748, .F. ) ;
#19654 = ORIENTED_EDGE ( 'NONE', *, *, #20694, .T. ) ;
#19655 = DIRECTION ( 'NONE',  ( -0.4792266786073193785, 0.4327645661435916002, 0.7635814434633321213 ) ) ;
#19656 = ORIENTED_EDGE ( 'NONE', *, *, #29160, .T. ) ;
#19657 = CARTESIAN_POINT ( 'NONE',  ( -336.3521761649654422, -139.2044816956407089, -56.89493493766761389 ) ) ;
#19658 = CIRCLE ( 'NONE', #4553, 125.0000000000000000 ) ;
#19659 = CARTESIAN_POINT ( 'NONE',  ( -19.51863976943889512, -189.7472609257535510, 120.5706864261536992 ) ) ;
#19660 = VECTOR ( 'NONE', #23062, 1000.000000000000000 ) ;
#19661 = AXIS2_PLACEMENT_3D ( 'NONE', #11686, #36117, #19571 ) ;
#19662 = DIRECTION ( 'NONE',  ( 0.000000000000000000, -0.8229838658936516893, 0.5680647467311625842 ) ) ;
#19663 = CARTESIAN_POINT ( 'NONE',  ( -62.43888699632653783, -189.7472609257535510, 124.2180546213279371 ) ) ;
#19664 = ORIENTED_EDGE ( 'NONE', *, *, #43345, .F. ) ;
#19667 = ORIENTED_EDGE ( 'NONE', *, *, #36862, .T. ) ;
#19666 = CARTESIAN_POINT ( 'NONE',  ( -330.4913330509368166, -84.75001853787810546, 44.49369547121489887 ) ) ;
#19665 = CARTESIAN_POINT ( 'NONE',  ( -88.78924379339714790, -177.1207230881787780, -118.3219948448692520 ) ) ;
#19668 = ORIENTED_EDGE ( 'NONE', *, *, #9328, .F. ) ;
#19669 = EDGE_CURVE ( 'NONE', #44484, #20620, #45263, .T. ) ;
#19670 = DIRECTION ( 'NONE',  ( -0.000000000000000000, 1.000000000000000000, -0.000000000000000000 ) ) ;
#19671 = ORIENTED_EDGE ( 'NONE', *, *, #20853, .T. ) ;
#19672 = LINE ( 'NONE', #27564, #27273 ) ;
#19673 = ORIENTED_EDGE ( 'NONE', *, *, #3577, .F. ) ;
#19674 = CYLINDRICAL_SURFACE ( 'NONE', #38486, 124.9999999999999858 ) ;
#19675 = ORIENTED_EDGE ( 'NONE', *, *, #51384, .F. ) ;
#19677 = CARTESIAN_POINT ( 'NONE',  ( -330.4913330509368166, -96.52406086224436876, -52.47426709956133806 ) ) ;
#19676 = DIRECTION ( 'NONE',  ( 0.000000000000000000, 7.470875769873448799E-14, -1.000000000000000000 ) ) ;
#19678 = VECTOR ( 'NONE', #19869, 1000.000000000000000 ) ;
#19679 = VERTEX_POINT ( 'NONE', #33143 ) ;
#19680 = DIRECTION ( 'NONE',  ( 1.000000000000000000, 0.000000000000000000, -0.000000000000000000 ) ) ;
#19681 = ORIENTED_EDGE ( 'NONE', *, *, #8986, .F. ) ;
#19682 = CARTESIAN_POINT ( 'NONE',  ( -48.47912675150885065, -189.7472609257535510, 6.938893903907228378E-15 ) ) ;
#19683 = PLANE ( 'NONE',  #2189 ) ;
#19684 = DIRECTION ( 'NONE',  ( 0.000000000000000000, 1.000000000000000000, -0.000000000000000000 ) ) ;
#19685 = PLANE ( 'NONE',  #39145 ) ;
#19686 = DIRECTION ( 'NONE',  ( 0.000000000000000000, 0.000000000000000000, 1.000000000000000000 ) ) ;
#19687 = DIRECTION ( 'NONE',  ( -0.9960498426152158968, 0.000000000000000000, -0.08879589532294571153 ) ) ;
#19688 = VERTEX_POINT ( 'NONE', #16344 ) ;
#19689 = EDGE_CURVE ( 'NONE', #37889, #23392, #36565, .T. ) ;
#19690 = DIRECTION ( 'NONE',  ( 0.000000000000000000, -0.5000000000000054401, -0.8660254037844354880 ) ) ;
#19691 = CARTESIAN_POINT ( 'NONE',  ( 66.73972540229262052, -175.3837268820161057, 45.83253885719641829 ) ) ;
#19692 = FACE_OUTER_BOUND ( 'NONE', #19382, .T. ) ;
#19693 = EDGE_LOOP ( 'NONE', ( #25919, #22842, #13098, #31148 ) ) ;
#19694 = LINE ( 'NONE', #11566, #3010 ) ;
#19695 = VECTOR ( 'NONE', #21302, 1000.000000000000114 ) ;
#19696 = VECTOR ( 'NONE', #40250, 1000.000000000000114 ) ;
#19697 = DIRECTION ( 'NONE',  ( 0.7575112421616145841, 0.000000000000000000, 0.6528221181905280446 ) ) ;
#19699 = VERTEX_POINT ( 'NONE', #44197 ) ;
#19698 = DIRECTION ( 'NONE',  ( -0.000000000000000000, -1.000000000000000000, -0.000000000000000000 ) ) ;
#19700 = ORIENTED_EDGE ( 'NONE', *, *, #2741, .F. ) ;
#19701 = VERTEX_POINT ( 'NONE', #16871 ) ;
#19702 = AXIS2_PLACEMENT_3D ( 'NONE', #15458, #50679, #47514 ) ;
#19703 = EDGE_CURVE ( 'NONE', #5112, #18389, #50126, .T. ) ;
#19704 = CARTESIAN_POINT ( 'NONE',  ( 75.10200014432447801, -193.5000000000000000, 10.18383939837614349 ) ) ;
#19705 = DIRECTION ( 'NONE',  ( -0.000000000000000000, 1.000000000000000000, -0.000000000000000000 ) ) ;
#19706 = AXIS2_PLACEMENT_3D ( 'NONE', #47290, #46769, #42553 ) ;
#19707 = CARTESIAN_POINT ( 'NONE',  ( -180.0000000000000568, -123.5000000000000284, 6.938893903907228378E-15 ) ) ;
#19708 = FACE_OUTER_BOUND ( 'NONE', #23853, .T. ) ;
#19709 = VECTOR ( 'NONE', #44806, 1000.000000000000000 ) ;
#19710 = ORIENTED_EDGE ( 'NONE', *, *, #51228, .F. ) ;
#19711 = EDGE_CURVE ( 'NONE', #47019, #38839, #5308, .T. ) ;
#19712 = CIRCLE ( 'NONE', #3775, 125.0000000000000000 ) ;
#19713 = CARTESIAN_POINT ( 'NONE',  ( 3.872902682125705542, 52.32033434345547818, -19.87165656769529321 ) ) ;
#19714 = ORIENTED_EDGE ( 'NONE', *, *, #37869, .F. ) ;
#19715 = VERTEX_POINT ( 'NONE', #32101 ) ;
#19716 = EDGE_CURVE ( 'NONE', #10327, #18753, #49193, .T. ) ;
#19717 = ORIENTED_EDGE ( 'NONE', *, *, #32004, .F. ) ;
#19718 = CARTESIAN_POINT ( 'NONE',  ( 43.63512310656542326, -175.3837268820161057, 84.49831343337136502 ) ) ;
#19719 = ORIENTED_EDGE ( 'NONE', *, *, #25254, .T. ) ;
#19720 = PLANE ( 'NONE',  #9099 ) ;
#19721 = CARTESIAN_POINT ( 'NONE',  ( -170.0000000000000284, -115.7896721143442278, 60.00000000000000711 ) ) ;
#19724 = VERTEX_POINT ( 'NONE', #16621 ) ;
#19723 = DIRECTION ( 'NONE',  ( 0.000000000000000000, -2.558138885907131360E-13, 1.000000000000000000 ) ) ;
#19722 = DIRECTION ( 'NONE',  ( -0.000000000000000000, -1.000000000000000000, -0.000000000000000000 ) ) ;
#19725 = VECTOR ( 'NONE', #25016, 1000.000000000000114 ) ;
#19726 = EDGE_CURVE ( 'NONE', #779, #10952, #32630, .T. ) ;
#19727 = CARTESIAN_POINT ( 'NONE',  ( -170.0502155641509319, -193.5000000000000000, -29.07697310430878090 ) ) ;
#19728 = AXIS2_PLACEMENT_3D ( 'NONE', #15763, #43596, #12034 ) ;
#19729 = ORIENTED_EDGE ( 'NONE', *, *, #46148, .F. ) ;
#19730 = LINE ( 'NONE', #43905, #1203 ) ;
#19731 = ORIENTED_EDGE ( 'NONE', *, *, #28066, .F. ) ;
#19732 = AXIS2_PLACEMENT_3D ( 'NONE', #36424, #425, #31328 ) ;
#19733 = CARTESIAN_POINT ( 'NONE',  ( -330.4913330509368166, -176.3931552210899554, 28.32515014536886611 ) ) ;
#19734 = CARTESIAN_POINT ( 'NONE',  ( -142.3192003680973414, -183.6283474603465606, 82.57748230379304744 ) ) ;
#19736 = CARTESIAN_POINT ( 'NONE',  ( -332.3517673607765914, -94.18160986457395722, 52.34913561719000796 ) ) ;
#19735 = LINE ( 'NONE', #8433, #14872 ) ;
#19737 = EDGE_CURVE ( 'NONE', #42695, #48318, #21062, .T. ) ;
#19738 = EDGE_LOOP ( 'NONE', ( #8940, #9474, #42855, #19777 ) ) ;
#19739 = CARTESIAN_POINT ( 'NONE',  ( 48.33059356687144970, -189.7472609257535510, 77.48473115145309009 ) ) ;
#19740 = CARTESIAN_POINT ( 'NONE',  ( 141.7825277784304205, -213.5000000000000000, 41.45482488023466772 ) ) ;
#19741 = DIRECTION ( 'NONE',  ( 0.1182731709213730997, 0.000000000000000000, -0.9929810960135161402 ) ) ;
#19742 = ORIENTED_EDGE ( 'NONE', *, *, #35478, .T. ) ;
#19743 = VECTOR ( 'NONE', #9930, 1000.000000000000114 ) ;
#19744 = LINE ( 'NONE', #51833, #9819 ) ;
#19745 = CARTESIAN_POINT ( 'NONE',  ( -339.1964088526558498, -124.0000000000002700, -59.00000000000002132 ) ) ;
#19746 = VECTOR ( 'NONE', #1041, 1000.000000000000000 ) ;
#19747 = CARTESIAN_POINT ( 'NONE',  ( 76.47090317495664635, -189.7472609257535510, -3.534122433557455256 ) ) ;
#19748 = VERTEX_POINT ( 'NONE', #32876 ) ;
#19749 = FACE_OUTER_BOUND ( 'NONE', #9143, .T. ) ;
#19750 = VECTOR ( 'NONE', #2370, 1000.000000000000000 ) ;
#19751 = DIRECTION ( 'NONE',  ( -0.000000000000000000, 0.6631226582408039638, 0.7485107481710934207 ) ) ;
#19752 = AXIS2_PLACEMENT_3D ( 'NONE', #25434, #25691, #1520 ) ;
#19753 = ORIENTED_EDGE ( 'NONE', *, *, #20244, .T. ) ;
#19754 = DIRECTION ( 'NONE',  ( 0.000000000000000000, 1.000000000000000000, 0.000000000000000000 ) ) ;
#19755 = ORIENTED_EDGE ( 'NONE', *, *, #31482, .T. ) ;
#19756 = FACE_OUTER_BOUND ( 'NONE', #51469, .T. ) ;
#19757 = DIRECTION ( 'NONE',  ( 0.000000000000000000, 0.000000000000000000, -1.000000000000000000 ) ) ;
#19758 = CARTESIAN_POINT ( 'NONE',  ( 17.15229921100055321, -177.1207230881787780, -106.3838142112212779 ) ) ;
#19759 = EDGE_CURVE ( 'NONE', #19237, #42041, #47606, .T. ) ;
#19760 = CARTESIAN_POINT ( 'NONE',  ( 15.29189835570547551, -193.5000000000000000, 106.3450133598704213 ) ) ;
#19761 = LINE ( 'NONE', #39983, #21556 ) ;
#19762 = ADVANCED_FACE ( 'NONE', ( #12907 ), #37083, .T. ) ;
#19763 = FACE_OUTER_BOUND ( 'NONE', #17233, .T. ) ;
#19764 = AXIS2_PLACEMENT_3D ( 'NONE', #46228, #22813, #2835 ) ;
#19765 = DIRECTION ( 'NONE',  ( -0.02963332782255633305, 0.000000000000000000, -0.9995608365087944591 ) ) ;
#19766 = DIRECTION ( 'NONE',  ( -0.000000000000000000, 1.000000000000000000, -0.000000000000000000 ) ) ;
#19768 = VERTEX_POINT ( 'NONE', #8449 ) ;
#19767 = DIRECTION ( 'NONE',  ( 0.000000000000000000, 0.000000000000000000, 1.000000000000000000 ) ) ;
#19769 = CIRCLE ( 'NONE', #49992, 125.0000000000000000 ) ;
#19770 = VECTOR ( 'NONE', #26557, 1000.000000000000114 ) ;
#19771 = ORIENTED_EDGE ( 'NONE', *, *, #31630, .T. ) ;
#19772 = CARTESIAN_POINT ( 'NONE',  ( -339.1964088526558498, -108.8949048983213004, -57.16590939599337418 ) ) ;
#19773 = ADVANCED_FACE ( 'NONE', ( #1082 ), #40239, .T. ) ;
#19774 = EDGE_CURVE ( 'NONE', #49340, #6620, #44994, .T. ) ;
#19775 = DIRECTION ( 'NONE',  ( -0.000000000000000000, 1.000000000000000000, -0.000000000000000000 ) ) ;
#19776 = VERTEX_POINT ( 'NONE', #36050 ) ;
#19777 = ORIENTED_EDGE ( 'NONE', *, *, #23713, .T. ) ;
#19778 = EDGE_CURVE ( 'NONE', #6620, #19239, #25431, .T. ) ;
#19779 = CIRCLE ( 'NONE', #3856, 125.0000000000000000 ) ;
#19780 = VERTEX_POINT ( 'NONE', #48147 ) ;
#19781 = LINE ( 'NONE', #11890, #37622 ) ;
#19782 = CARTESIAN_POINT ( 'NONE',  ( -332.3517673607765914, -74.01670616005314685, 32.17247266903214609 ) ) ;
#19783 = VECTOR ( 'NONE', #37046, 1000.000000000000000 ) ;
#19784 = EDGE_CURVE ( 'NONE', #18133, #10779, #4254, .T. ) ;
#19786 = VECTOR ( 'NONE', #39963, 1000.000000000000114 ) ;
#19785 = CARTESIAN_POINT ( 'NONE',  ( 1.150725574412418739, -189.7472609257535510, -114.7252272087845881 ) ) ;
#19787 = DIRECTION ( 'NONE',  ( 1.000000000000000000, -0.000000000000000000, 6.978251959525016136E-17 ) ) ;
#19788 = VERTEX_POINT ( 'NONE', #4519 ) ;
#19789 = EDGE_LOOP ( 'NONE', ( #220, #3003, #8518, #22082 ) ) ;
#19790 = VERTEX_POINT ( 'NONE', #1348 ) ;
#19791 = VECTOR ( 'NONE', #40661, 1000.000000000000000 ) ;
#19792 = DIRECTION ( 'NONE',  ( 0.000000000000000000, -0.2393156642875482465, 0.9709418174260544543 ) ) ;
#19793 = CARTESIAN_POINT ( 'NONE',  ( -336.3521761649654422, -74.01670616005314685, 32.17247266903214609 ) ) ;
#19794 = DIRECTION ( 'NONE',  ( 0.000000000000000000, 9.251858538542971828E-16, 1.000000000000000000 ) ) ;
#19795 = FACE_OUTER_BOUND ( 'NONE', #10554, .T. ) ;
#19796 = DIRECTION ( 'NONE',  ( -0.5085311186492273983, 0.000000000000000000, 0.8610436117673514467 ) ) ;
#19797 = ORIENTED_EDGE ( 'NONE', *, *, #17989, .T. ) ;
#19798 = DIRECTION ( 'NONE',  ( 1.000000000000000000, -0.000000000000000000, 0.000000000000000000 ) ) ;
#19799 = LINE ( 'NONE', #51888, #45809 ) ;
#19800 = CARTESIAN_POINT ( 'NONE',  ( -280.0000000000000000, -153.5000000000000284, 60.00000000000002132 ) ) ;
#19801 = VERTEX_POINT ( 'NONE', #22102 ) ;
#19802 = ORIENTED_EDGE ( 'NONE', *, *, #40156, .T. ) ;
#19803 = EDGE_LOOP ( 'NONE', ( #21652, #386, #15892, #26197 ) ) ;
#19804 = LINE ( 'NONE', #7981, #42434 ) ;
#19805 = AXIS2_PLACEMENT_3D ( 'NONE', #41472, #38309, #17834 ) ;
#19806 = CARTESIAN_POINT ( 'NONE',  ( -47.87232660569026166, -183.6283474603465606, 0.7948544414133635883 ) ) ;
#19807 = EDGE_LOOP ( 'NONE', ( #19990, #28047, #24558, #35336 ) ) ;
#19808 = CARTESIAN_POINT ( 'NONE',  ( 70.19984492582109681, -175.3837268820161057, 39.24667733211968823 ) ) ;
#19809 = AXIS2_PLACEMENT_3D ( 'NONE', #2627, #30236, #18414 ) ;
#19810 = VECTOR ( 'NONE', #31577, 1000.000000000000114 ) ;
#19811 = DIRECTION ( 'NONE',  ( -0.000000000000000000, 1.000000000000000000, -0.000000000000000000 ) ) ;
#19812 = CARTESIAN_POINT ( 'NONE',  ( -49.21696003055057389, -175.3837268820161057, -0.6749830015182127774 ) ) ;
#19813 = VERTEX_POINT ( 'NONE', #9500 ) ;
#19814 = DIRECTION ( 'NONE',  ( 0.000000000000000000, 0.000000000000000000, 1.000000000000000000 ) ) ;
#19815 = ORIENTED_EDGE ( 'NONE', *, *, #32115, .T. ) ;
#19816 = CARTESIAN_POINT ( 'NONE',  ( -167.6453766917639427, -177.1207230881787780, 37.74128873232410086 ) ) ;
#19817 = CYLINDRICAL_SURFACE ( 'NONE', #22118, 125.0000000000000000 ) ;
#19818 = VECTOR ( 'NONE', #13521, 1000.000000000000000 ) ;
#19819 = CARTESIAN_POINT ( 'NONE',  ( -66.64622755927948106, -177.1207230881787780, 123.6727797384707515 ) ) ;
#19820 = ORIENTED_EDGE ( 'NONE', *, *, #12095, .T. ) ;
#19821 = AXIS2_PLACEMENT_3D ( 'NONE', #18031, #50355, #18543 ) ;
#19822 = PRESENTATION_LAYER_ASSIGNMENT (  '', '', ( #42484 ) ) ;
#19823 = EDGE_CURVE ( 'NONE', #47279, #11613, #18166, .T. ) ;
#19824 = DIRECTION ( 'NONE',  ( -0.000000000000000000, 1.000000000000000000, -0.000000000000000000 ) ) ;
#19825 = EDGE_CURVE ( 'NONE', #35, #4302, #247, .T. ) ;
#19826 = CARTESIAN_POINT ( 'NONE',  ( 67.29469129333651267, -183.6283474603465606, -44.41421852208627996 ) ) ;
#19827 = DIRECTION ( 'NONE',  ( 0.000000000000000000, 1.000000000000000000, 0.000000000000000000 ) ) ;
#19828 = EDGE_CURVE ( 'NONE', #37488, #48517, #34646, .T. ) ;
#19829 = VECTOR ( 'NONE', #50379, 1000.000000000000000 ) ;
#19830 = CARTESIAN_POINT ( 'NONE',  ( -91.84482189527193441, -175.3837268820161057, -117.2365833888816553 ) ) ;
#19831 = EDGE_CURVE ( 'NONE', #39559, #47693, #21232, .T. ) ;
#19832 = ORIENTED_EDGE ( 'NONE', *, *, #38305, .F. ) ;
#19834 = VECTOR ( 'NONE', #12098, 1000.000000000000114 ) ;
#19833 = FACE_OUTER_BOUND ( 'NONE', #49404, .T. ) ;
#19835 = ORIENTED_EDGE ( 'NONE', *, *, #47844, .T. ) ;
#19836 = ORIENTED_EDGE ( 'NONE', *, *, #7513, .T. ) ;
#19837 = ADVANCED_FACE ( 'NONE', ( #46292 ), #22360, .T. ) ;
#19838 = CARTESIAN_POINT ( 'NONE',  ( -339.1964088526558498, -95.63860483659040312, 52.00954392751717847 ) ) ;
#19840 = ORIENTED_EDGE ( 'NONE', *, *, #42439, .F. ) ;
#19839 = CARTESIAN_POINT ( 'NONE',  ( 67.66641500972446011, -189.7472609257535510, 46.20836643931067300 ) ) ;
#19841 = ADVANCED_FACE ( 'NONE', ( #2395 ), #41819, .T. ) ;
#19842 = VERTEX_POINT ( 'NONE', #5840 ) ;
#19843 = CARTESIAN_POINT ( 'NONE',  ( 21.49274850782854074, -175.3837268820161057, -103.5805805771126700 ) ) ;
#19844 = EDGE_CURVE ( 'NONE', #22714, #5997, #17907, .T. ) ;
#19845 = EDGE_CURVE ( 'NONE', #30580, #22041, #29456, .T. ) ;
#19846 = FACE_OUTER_BOUND ( 'NONE', #12592, .T. ) ;
#19847 = VECTOR ( 'NONE', #22289, 1000.000000000000000 ) ;
#19848 = VERTEX_POINT ( 'NONE', #13442 ) ;
#19849 = ADVANCED_FACE ( 'NONE', ( #5570 ), #13699, .F. ) ;
#19850 = CARTESIAN_POINT ( 'NONE',  ( 57.31108707223382481, -193.5000000000000000, -66.58401203837755133 ) ) ;
#19851 = DIRECTION ( 'NONE',  ( -1.000000000000000000, -0.000000000000000000, 0.000000000000000000 ) ) ;
#19852 = EDGE_LOOP ( 'NONE', ( #5421, #3926, #32550, #31090 ) ) ;
#19853 = CARTESIAN_POINT ( 'NONE',  ( -332.3517673607765914, -183.4422309845877805, 2.632288850093980503 ) ) ;
#19854 = CARTESIAN_POINT ( 'NONE',  ( 0.000000000000000000, -63.50000000000000000, -60.00000000000000711 ) ) ;
#19855 = AXIS2_PLACEMENT_3D ( 'NONE', #33828, #51181, #36155 ) ;
#19856 = EDGE_CURVE ( 'NONE', #23381, #41706, #34442, .T. ) ;
#19857 = LINE ( 'NONE', #32721, #38669 ) ;
#19858 = CARTESIAN_POINT ( 'NONE',  ( 0.000000000000000000, 111.8512453678547018, -94.59399843624255766 ) ) ;
#19859 = ORIENTED_EDGE ( 'NONE', *, *, #43907, .F. ) ;
#19860 = ORIENTED_EDGE ( 'NONE', *, *, #32422, .F. ) ;
#19861 = ORIENTED_EDGE ( 'NONE', *, *, #24700, .F. ) ;
#19862 = CARTESIAN_POINT ( 'NONE',  ( -305.0000000000000568, -123.5000000000000284, 20.00000000000000355 ) ) ;
#19863 = DIRECTION ( 'NONE',  ( 0.000000000000000000, -1.000000000000000000, 0.000000000000000000 ) ) ;
#19864 = AXIS2_PLACEMENT_3D ( 'NONE', #43424, #38683, #30809 ) ;
#19865 = AXIS2_PLACEMENT_3D ( 'NONE', #44985, #25008, #22866 ) ;
#19866 = DIRECTION ( 'NONE',  ( 0.8455960035018311727, 0.000000000000000000, -0.5338233779647826305 ) ) ;
#19867 = AXIS2_PLACEMENT_3D ( 'NONE', #33283, #25653, #1741 ) ;
#19868 = DIRECTION ( 'NONE',  ( 1.000000000000000000, -0.000000000000000000, -0.000000000000000000 ) ) ;
#19869 = DIRECTION ( 'NONE',  ( -0.000000000000000000, 1.000000000000000000, -0.000000000000000000 ) ) ;
#19870 = ORIENTED_EDGE ( 'NONE', *, *, #28707, .T. ) ;
#19871 = VECTOR ( 'NONE', #9590, 1000.000000000000114 ) ;
#19872 = EDGE_CURVE ( 'NONE', #7481, #10649, #37167, .T. ) ;
#19873 = VECTOR ( 'NONE', #43346, 1000.000000000000000 ) ;
#19874 = DIRECTION ( 'NONE',  ( -0.4566292373937018145, 0.000000000000000000, -0.8896570909947529859 ) ) ;
#19875 = ORIENTED_EDGE ( 'NONE', *, *, #9317, .T. ) ;
#19877 = ORIENTED_EDGE ( 'NONE', *, *, #45602, .T. ) ;
#19876 = DIRECTION ( 'NONE',  ( -0.8124868780056783146, 0.000000000000000000, -0.5829794791144762289 ) ) ;
#19878 = ORIENTED_EDGE ( 'NONE', *, *, #38110, .T. ) ;
#19879 = CARTESIAN_POINT ( 'NONE',  ( -70.75782287548091176, -175.3837268820161057, 122.9986166548864901 ) ) ;
#19880 = CARTESIAN_POINT ( 'NONE',  ( -87.88805327685030022, -183.6283474603465606, 117.5715283571807106 ) ) ;
#19881 = LINE ( 'NONE', #24097, #31230 ) ;
#19882 = CARTESIAN_POINT ( 'NONE',  ( -163.4524646452520926, -193.5000000000000000, 46.44493303993097300 ) ) ;
#19883 = ORIENTED_EDGE ( 'NONE', *, *, #23780, .T. ) ;
#19884 = CARTESIAN_POINT ( 'NONE',  ( -11.17913199888832843, -189.7472609257535510, 119.3051146910914326 ) ) ;
#19885 = ORIENTED_EDGE ( 'NONE', *, *, #11773, .T. ) ;
#19886 = ADVANCED_FACE ( 'NONE', ( #30246 ), #1623, .F. ) ;
#19887 = ORIENTED_EDGE ( 'NONE', *, *, #46863, .F. ) ;
#19888 = AXIS2_PLACEMENT_3D ( 'NONE', #3542, #7236, #39291 ) ;
#19889 = VECTOR ( 'NONE', #5053, 1000.000000000000000 ) ;
#19890 = PLANE ( 'NONE',  #25709 ) ;
#19891 = LINE ( 'NONE', #3870, #48261 ) ;
#19892 = VECTOR ( 'NONE', #37634, 1000.000000000000000 ) ;
#19893 = ADVANCED_FACE ( 'NONE', ( #10273 ), #14486, .T. ) ;
#19894 = EDGE_CURVE ( 'NONE', #3648, #24784, #45763, .T. ) ;
#19895 = CARTESIAN_POINT ( 'NONE',  ( -169.6464974000608379, -175.3837268820161057, 26.35287080855539088 ) ) ;
#19896 = CYLINDRICAL_SURFACE ( 'NONE', #42158, 125.0000000000000000 ) ;
#19897 = EDGE_CURVE ( 'NONE', #10996, #22773, #30494, .T. ) ;
#19898 = ORIENTED_EDGE ( 'NONE', *, *, #8121, .F. ) ;
#19899 = DIRECTION ( 'NONE',  ( -0.000000000000000000, -0.7485107481711046340, -0.6631226582407911962 ) ) ;
#19900 = FACE_OUTER_BOUND ( 'NONE', #10083, .T. ) ;
#19901 = ADVANCED_FACE ( 'NONE', ( #26289 ), #37346, .F. ) ;
#19902 = FACE_BOUND ( 'NONE', #16925, .T. ) ;
#19903 = ORIENTED_EDGE ( 'NONE', *, *, #51636, .T. ) ;
#19904 = VECTOR ( 'NONE', #42992, 1000.000000000000000 ) ;
#19905 = CIRCLE ( 'NONE', #28300, 125.0000000000000000 ) ;
#19906 = LINE ( 'NONE', #40372, #18930 ) ;
#19907 = VECTOR ( 'NONE', #50011, 1000.000000000000000 ) ;
#19908 = CARTESIAN_POINT ( 'NONE',  ( -46.00000000000000711, 20.00000000000000000, -46.00000000000000000 ) ) ;
#19909 = ORIENTED_EDGE ( 'NONE', *, *, #4144, .T. ) ;
#19910 = DIRECTION ( 'NONE',  ( 0.000000000000000000, 0.000000000000000000, 1.000000000000000000 ) ) ;
#19911 = AXIS2_PLACEMENT_3D ( 'NONE', #48954, #595, #4815 ) ;
#19912 = VERTEX_POINT ( 'NONE', #31012 ) ;
#19913 = VECTOR ( 'NONE', #8964, 1000.000000000000000 ) ;
#19914 = FACE_OUTER_BOUND ( 'NONE', #26215, .T. ) ;
#19915 = EDGE_CURVE ( 'NONE', #4854, #48288, #35460, .T. ) ;
#19916 = FACE_BOUND ( 'NONE', #16155, .T. ) ;
#19918 = ORIENTED_EDGE ( 'NONE', *, *, #23774, .T. ) ;
#19917 = PLANE ( 'NONE',  #50612 ) ;
#19919 = EDGE_CURVE ( 'NONE', #20876, #4233, #19438, .T. ) ;
#19920 = CARTESIAN_POINT ( 'NONE',  ( -339.1964088526558498, -71.49045607248213230, 27.86139516340826106 ) ) ;
#19921 = VERTEX_POINT ( 'NONE', #51263 ) ;
#19922 = EDGE_CURVE ( 'NONE', #32747, #37279, #7105, .T. ) ;
#19923 = ORIENTED_EDGE ( 'NONE', *, *, #7051, .F. ) ;
#19924 = LINE ( 'NONE', #16245, #35128 ) ;
#19925 = VECTOR ( 'NONE', #47754, 1000.000000000000000 ) ;
#19926 = AXIS2_PLACEMENT_3D ( 'NONE', #48064, #4697, #24933 ) ;
#19927 = ORIENTED_EDGE ( 'NONE', *, *, #48803, .F. ) ;
#19928 = CARTESIAN_POINT ( 'NONE',  ( -73.70588833648351113, -193.5000000000000000, 121.4073237908568359 ) ) ;
#19929 = CARTESIAN_POINT ( 'NONE',  ( -48.47912675150885065, -177.1207230881787780, 6.938893903907228378E-15 ) ) ;
#19930 = VECTOR ( 'NONE', #48891, 1000.000000000000000 ) ;
#19931 = DIRECTION ( 'NONE',  ( 0.000000000000000000, -0.8854560256532141294, -0.4647231720437604574 ) ) ;
#19932 = CARTESIAN_POINT ( 'NONE',  ( -46.00000000000000711, 0.000000000000000000, 8.673617379884035472E-15 ) ) ;
#19933 = ORIENTED_EDGE ( 'NONE', *, *, #3995, .F. ) ;
#19936 = EDGE_LOOP ( 'NONE', ( #33633, #28807, #22547, #16969 ) ) ;
#19935 = DIRECTION ( 'NONE',  ( 0.000000000000000000, 0.000000000000000000, -1.000000000000000000 ) ) ;
#19934 = CARTESIAN_POINT ( 'NONE',  ( -150.5215542367829471, -189.7472609257535510, -72.19655804061974891 ) ) ;
#19937 = AXIS2_PLACEMENT_3D ( 'NONE', #41899, #31095, #2723 ) ;
#19938 = ORIENTED_EDGE ( 'NONE', *, *, #18313, .T. ) ;
#19939 = AXIS2_PLACEMENT_3D ( 'NONE', #24204, #32322, #1053 ) ;
#19940 = VECTOR ( 'NONE', #41144, 1000.000000000000341 ) ;
#19941 = CARTESIAN_POINT ( 'NONE',  ( -339.1964088526558498, -63.87926739338334414, -6.735595255826711814 ) ) ;
#19942 = ORIENTED_EDGE ( 'NONE', *, *, #40718, .T. ) ;
#19943 = LINE ( 'NONE', #20195, #50779 ) ;
#19944 = ORIENTED_EDGE ( 'NONE', *, *, #37514, .F. ) ;
#19945 = AXIS2_PLACEMENT_3D ( 'NONE', #27314, #10782, #3402 ) ;
#19946 = DIRECTION ( 'NONE',  ( 0.000000000000000000, 0.000000000000000000, 1.000000000000000000 ) ) ;
#19947 = EDGE_LOOP ( 'NONE', ( #39515, #8117 ) ) ;
#19949 = DIRECTION ( 'NONE',  ( -0.000000000000000000, 0.8854560256532157947, 0.4647231720437573488 ) ) ;
#19948 = DIRECTION ( 'NONE',  ( -1.000000000000000000, -0.000000000000000000, -0.000000000000000000 ) ) ;
#19950 = ORIENTED_EDGE ( 'NONE', *, *, #14700, .F. ) ;
#19951 = AXIS2_PLACEMENT_3D ( 'NONE', #33113, #16848, #36807 ) ;
#19952 = VERTEX_POINT ( 'NONE', #23140 ) ;
#19953 = CARTESIAN_POINT ( 'NONE',  ( -330.4913330509368166, -156.6043281241909995, 48.84008046109159551 ) ) ;
#19954 = CARTESIAN_POINT ( 'NONE',  ( -172.2289551866394106, -193.5000000000000000, -17.63462396184707970 ) ) ;
#19955 = CARTESIAN_POINT ( 'NONE',  ( -339.1964088526558498, -79.00630452878414189, 38.74998146212082162 ) ) ;
#19956 = PLANE ( 'NONE',  #4012 ) ;
#19957 = CARTESIAN_POINT ( 'NONE',  ( -332.3517673607765914, -182.3871109312487420, -4.498567634386014369 ) ) ;
#19958 = DIRECTION ( 'NONE',  ( 0.000000000000000000, 0.000000000000000000, 1.000000000000000000 ) ) ;
#19959 = ORIENTED_EDGE ( 'NONE', *, *, #21894, .F. ) ;
#19960 = EDGE_CURVE ( 'NONE', #11395, #32749, #3623, .T. ) ;
#19961 = ADVANCED_FACE ( 'NONE', ( #39154 ), #3410, .T. ) ;
#19962 = CARTESIAN_POINT ( 'NONE',  ( 0.000000000000000000, 0.000000000000000000, 0.000000000000000000 ) ) ;
#19963 = CARTESIAN_POINT ( 'NONE',  ( 72.14504940832446778, -193.5000000000000000, -32.78426643622660208 ) ) ;
#19964 = LINE ( 'NONE', #51780, #39900 ) ;
#19965 = DIRECTION ( 'NONE',  ( 0.9720229140804089729, 0.000000000000000000, 0.2348860457809911206 ) ) ;
#19966 = ORIENTED_EDGE ( 'NONE', *, *, #44128, .F. ) ;
#19967 = VECTOR ( 'NONE', #3782, 1000.000000000000000 ) ;
#19968 = AXIS2_PLACEMENT_3D ( 'NONE', #25632, #29052, #41663 ) ;
#19969 = FACE_OUTER_BOUND ( 'NONE', #13524, .T. ) ;
#19970 = VECTOR ( 'NONE', #38719, 1000.000000000000000 ) ;
#19971 = DIRECTION ( 'NONE',  ( 0.000000000000000000, 0.4845575045900850641, -0.8747594096352605542 ) ) ;
#19972 = CARTESIAN_POINT ( 'NONE',  ( -65.65563056894596627, -183.6283474603465606, 123.8142468240612999 ) ) ;
#19973 = VERTEX_POINT ( 'NONE', #15250 ) ;
#19974 = ORIENTED_EDGE ( 'NONE', *, *, #51010, .F. ) ;
#19975 = VERTEX_POINT ( 'NONE', #15787 ) ;
#19976 = AXIS2_PLACEMENT_3D ( 'NONE', #31355, #23729, #27925 ) ;
#19977 = DIRECTION ( 'NONE',  ( 0.8610436117673514467, 0.000000000000000000, 0.5085311186492273983 ) ) ;
#19978 = DIRECTION ( 'NONE',  ( 0.4031234292879665171, 0.000000000000000000, 0.9151456172430210145 ) ) ;
#19979 = EDGE_CURVE ( 'NONE', #32000, #32301, #47317, .T. ) ;
#19980 = CARTESIAN_POINT ( 'NONE',  ( -339.1964088526558498, -66.09477493971917283, -13.63415328425296202 ) ) ;
#19981 = DIRECTION ( 'NONE',  ( 1.000000000000000000, 0.000000000000000000, 0.000000000000000000 ) ) ;
#19982 = ORIENTED_EDGE ( 'NONE', *, *, #41070, .F. ) ;
#19983 = CARTESIAN_POINT ( 'NONE',  ( 4.321872425944940588, 55.11937612772108963, -17.91061045145632846 ) ) ;
#19984 = EDGE_CURVE ( 'NONE', #36830, #43678, #22097, .T. ) ;
#19985 = VECTOR ( 'NONE', #28327, 1000.000000000000000 ) ;
#19986 = VERTEX_POINT ( 'NONE', #2639 ) ;
#19987 = ORIENTED_EDGE ( 'NONE', *, *, #50700, .F. ) ;
#19988 = ORIENTED_EDGE ( 'NONE', *, *, #32339, .F. ) ;
#19989 = DIRECTION ( 'NONE',  ( 0.000000000000000000, 0.000000000000000000, 1.000000000000000000 ) ) ;
#19990 = ORIENTED_EDGE ( 'NONE', *, *, #14619, .F. ) ;
#19991 = DIRECTION ( 'NONE',  ( 0.9473263538541876194, 0.000000000000000000, 0.3202698538628486746 ) ) ;
#19992 = DIRECTION ( 'NONE',  ( -0.000000000000000000, 1.000000000000000000, -0.000000000000000000 ) ) ;
#19993 = AXIS2_PLACEMENT_3D ( 'NONE', #38681, #26083, #2944 ) ;
#19996 = ORIENTED_EDGE ( 'NONE', *, *, #43398, .F. ) ;
#19995 = DIRECTION ( 'NONE',  ( -1.000000000000000000, 0.000000000000000000, -0.000000000000000000 ) ) ;
#19994 = CARTESIAN_POINT ( 'NONE',  ( -49.40581635894068313, -189.7472609257535510, -0.3758275821142418316 ) ) ;
#19997 = VECTOR ( 'NONE', #7740, 1000.000000000000000 ) ;
#19998 = VECTOR ( 'NONE', #25237, 1000.000000000000000 ) ;
#19999 = DIRECTION ( 'NONE',  ( -1.000000000000000000, -0.000000000000000000, 0.000000000000000000 ) ) ;
#20000 = ORIENTED_EDGE ( 'NONE', *, *, #50577, .T. ) ;
#20001 = CARTESIAN_POINT ( 'NONE',  ( -48.47912675150883643, -189.7472609257535510, -125.0000000000000000 ) ) ;
#20002 = AXIS2_PLACEMENT_3D ( 'NONE', #39675, #28382, #48109 ) ;
#20003 = EDGE_LOOP ( 'NONE', ( #13719, #35136, #13982, #6551 ) ) ;
#20004 = LINE ( 'NONE', #36033, #24943 ) ;
#20005 = CARTESIAN_POINT ( 'NONE',  ( 0.000000000000000000, -123.4999999999994174, 59.00000000000002132 ) ) ;
#20007 = LINE ( 'NONE', #39202, #26499 ) ;
#20006 = FACE_OUTER_BOUND ( 'NONE', #17268, .T. ) ;
#20008 = ORIENTED_EDGE ( 'NONE', *, *, #26463, .F. ) ;
#20009 = EDGE_CURVE ( 'NONE', #43701, #7946, #31523, .T. ) ;
#20010 = VECTOR ( 'NONE', #46185, 1000.000000000000000 ) ;
#20011 = CARTESIAN_POINT ( 'NONE',  ( -46.00000000000000711, 0.000000000000000000, 5.000000000000006217 ) ) ;
#20012 = CARTESIAN_POINT ( 'NONE',  ( -336.3521761649654422, -177.7325358280884586, 23.38292116578760726 ) ) ;
#20013 = FACE_OUTER_BOUND ( 'NONE', #47919, .T. ) ;
#20014 = ORIENTED_EDGE ( 'NONE', *, *, #50938, .T. ) ;
#20015 = CARTESIAN_POINT ( 'NONE',  ( 42.96730897722186171, 35.00000000000000000, -41.16782622478179832 ) ) ;
#20016 = CARTESIAN_POINT ( 'NONE',  ( -48.47912675150885065, -189.7472609257535510, 6.938893903907228378E-15 ) ) ;
#20017 = CARTESIAN_POINT ( 'NONE',  ( -127.4665351220365892, -177.1207230881787780, -96.88131563365291754 ) ) ;
#20018 = ORIENTED_EDGE ( 'NONE', *, *, #20873, .F. ) ;
#20019 = EDGE_CURVE ( 'NONE', #3372, #13063, #14527, .T. ) ;
#20020 = CARTESIAN_POINT ( 'NONE',  ( -305.0000000000000568, -171.3361784870343740, 36.21739951675979086 ) ) ;
#20021 = DIRECTION ( 'NONE',  ( 0.000000000000000000, 0.9927088740980556381, 0.1205366802553095307 ) ) ;
#20022 = AXIS2_PLACEMENT_3D ( 'NONE', #4694, #8378, #44638 ) ;
#20023 = ORIENTED_EDGE ( 'NONE', *, *, #31937, .T. ) ;
#20024 = CARTESIAN_POINT ( 'NONE',  ( 76.43863189440992301, -175.3837268820161057, -4.533605064403313456 ) ) ;
#20025 = ORIENTED_EDGE ( 'NONE', *, *, #13441, .F. ) ;
#20026 = EDGE_CURVE ( 'NONE', #7370, #26319, #19198, .T. ) ;
#20027 = CARTESIAN_POINT ( 'NONE',  ( -332.3517673607765914, -161.2787550547969033, 46.61293454085098631 ) ) ;
#20028 = DIRECTION ( 'NONE',  ( 0.000000000000000000, 1.000000000000000000, 0.000000000000000000 ) ) ;
#20029 = LINE ( 'NONE', #16096, #10120 ) ;
#20030 = CARTESIAN_POINT ( 'NONE',  ( -48.24424070572786860, -189.7472609257535510, -0.9720229140804037549 ) ) ;
#20031 = DIRECTION ( 'NONE',  ( -0.9982437317643214625, 0.000000000000000000, -0.05924062789371441901 ) ) ;
#20032 = DIRECTION ( 'NONE',  ( -0.000000000000000000, -0.5680647467311596976, -0.8229838658936536877 ) ) ;
#20033 = VECTOR ( 'NONE', #14800, 1000.000000000000000 ) ;
#20034 = MECHANICAL_DESIGN_GEOMETRIC_PRESENTATION_REPRESENTATION (  '', ( #13332 ), #8304 ) ;
#20035 = CARTESIAN_POINT ( 'NONE',  ( -47.97059563285963435, -193.5000000000000000, 0.8610436117673654355 ) ) ;
#20036 = EDGE_CURVE ( 'NONE', #6126, #20552, #50610, .T. ) ;
#20037 = CYLINDRICAL_SURFACE ( 'NONE', #3754, 125.0000000000000000 ) ;
#20039 = VERTEX_POINT ( 'NONE', #51011 ) ;
#20038 = DIRECTION ( 'NONE',  ( -0.8124868780056742068, 0.000000000000000000, -0.5829794791144820021 ) ) ;
#20040 = CIRCLE ( 'NONE', #13336, 125.0000000000000000 ) ;
#20041 = ORIENTED_EDGE ( 'NONE', *, *, #25265, .T. ) ;
#20042 = LINE ( 'NONE', #8215, #35833 ) ;
#20043 = CARTESIAN_POINT ( 'NONE',  ( -49.29161362951453640, -193.5000000000000000, 0.5829794791144718991 ) ) ;
#20044 = ORIENTED_EDGE ( 'NONE', *, *, #5806, .T. ) ;
#20045 = AXIS2_PLACEMENT_3D ( 'NONE', #5718, #1754, #41433 ) ;
#20046 = ORIENTED_EDGE ( 'NONE', *, *, #23052, .F. ) ;
#20047 = ORIENTED_EDGE ( 'NONE', *, *, #1601, .T. ) ;
#20048 = DIRECTION ( 'NONE',  ( 0.000000000000000000, 0.000000000000000000, -1.000000000000000000 ) ) ;
#20049 = DIRECTION ( 'NONE',  ( 0.9890401873221623674, 0.000000000000000000, 0.1476465640024917925 ) ) ;
#20050 = LINE ( 'NONE', #51873, #6014 ) ;
#20051 = DIRECTION ( 'NONE',  ( 0.000000000000000000, 0.000000000000000000, -1.000000000000000000 ) ) ;
#20052 = ORIENTED_EDGE ( 'NONE', *, *, #8005, .F. ) ;
#20053 = EDGE_LOOP ( 'NONE', ( #20610, #27981, #35047, #7122 ) ) ;
#20054 = EDGE_LOOP ( 'NONE', ( #45484, #25922 ) ) ;
#20055 = VECTOR ( 'NONE', #19118, 1000.000000000000227 ) ;
#20056 = CARTESIAN_POINT ( 'NONE',  ( 51.65665342072241373, -177.1207230881787780, 74.81861753132420745 ) ) ;
#20057 = PLANE ( 'NONE',  #26024 ) ;
#20058 = CARTESIAN_POINT ( 'NONE',  ( -336.3521761649654422, -66.60506506233235768, -15.70448169564047092 ) ) ;
#20059 = DIRECTION ( 'NONE',  ( 0.000000000000000000, -0.000000000000000000, 1.000000000000000000 ) ) ;
#20060 = LINE ( 'NONE', #12158, #29768 ) ;
#20061 = VERTEX_POINT ( 'NONE', #46802 ) ;
#20062 = CARTESIAN_POINT ( 'NONE',  ( -332.3517673607765914, -80.42027357919624819, -40.34602258462219027 ) ) ;
#20063 = ADVANCED_FACE ( 'NONE', ( #39405 ), #10790, .F. ) ;
#20064 = LINE ( 'NONE', #36091, #32433 ) ;
#20065 = CARTESIAN_POINT ( 'NONE',  ( -330.4913330509368166, -68.51134412508180560, -21.38919645685231075 ) ) ;
#20066 = CARTESIAN_POINT ( 'NONE',  ( -111.3295483157475445, -193.5000000000000000, 108.0501018472332504 ) ) ;
#20067 = EDGE_CURVE ( 'NONE', #49029, #3029, #20396, .T. ) ;
#20068 = ORIENTED_EDGE ( 'NONE', *, *, #19275, .F. ) ;
#20069 = ORIENTED_EDGE ( 'NONE', *, *, #16665, .F. ) ;
#20070 = ORIENTED_EDGE ( 'NONE', *, *, #14430, .F. ) ;
#20071 = PLANE ( 'NONE',  #45790 ) ;
#20073 = VECTOR ( 'NONE', #36445, 1000.000000000000000 ) ;
#20072 = DIRECTION ( 'NONE',  ( 0.6965510290629932655, 0.000000000000000000, 0.7175072570443347120 ) ) ;
#20074 = ORIENTED_EDGE ( 'NONE', *, *, #43846, .F. ) ;
#20075 = CARTESIAN_POINT ( 'NONE',  ( -336.3521761649654422, -166.5797264208035244, 40.34602258462248159 ) ) ;
#20076 = COLOUR_RGB ( '', 0.09019608, 0.27058824, 0.51372549) ;
#20077 = DIRECTION ( 'NONE',  ( 0.000000000000000000, -0.000000000000000000, -1.000000000000000000 ) ) ;
#20078 = DIRECTION ( 'NONE',  ( 0.5586467658036415873, 0.000000000000000000, 0.8294056854502090959 ) ) ;
#20079 = ORIENTED_EDGE ( 'NONE', *, *, #27888, .T. ) ;
#20080 = EDGE_CURVE ( 'NONE', #46003, #46969, #47579, .T. ) ;
#20081 = CARTESIAN_POINT ( 'NONE',  ( -339.1964088526558498, -151.8251501453679850, 52.89315522109039591 ) ) ;
#20082 = ADVANCED_FACE ( 'NONE', ( #19692 ), #39653, .T. ) ;
#20083 = EDGE_CURVE ( 'NONE', #29431, #40004, #35724, .T. ) ;
#20084 = VERTEX_POINT ( 'NONE', #43099 ) ;
#20085 = CARTESIAN_POINT ( 'NONE',  ( 70.68712318874649725, -193.5000000000000000, -37.74128873232327663 ) ) ;
#20086 = ORIENTED_EDGE ( 'NONE', *, *, #39419, .F. ) ;
#20087 = DIRECTION ( 'NONE',  ( 0.000000000000000000, 0.000000000000000000, -1.000000000000000000 ) ) ;
#20088 = EDGE_CURVE ( 'NONE', #15690, #22268, #7868, .T. ) ;
#20089 = DIRECTION ( 'NONE',  ( 0.000000000000000000, 1.000000000000000000, -0.000000000000000000 ) ) ;
#20090 = ORIENTED_EDGE ( 'NONE', *, *, #15703, .T. ) ;
#20091 = CARTESIAN_POINT ( 'NONE',  ( 46.00000000000000000, 20.00000000000000000, 0.000000000000000000 ) ) ;
#20092 = DIRECTION ( 'NONE',  ( 0.000000000000000000, -0.000000000000000000, 1.000000000000000000 ) ) ;
#20093 = CARTESIAN_POINT ( 'NONE',  ( -336.3521761649654422, -182.3871109312487420, -4.498567634386014369 ) ) ;
#20094 = CARTESIAN_POINT ( 'NONE',  ( -169.9131040279660567, -183.6283474603465606, 29.64437826672833864 ) ) ;
#20095 = AXIS2_PLACEMENT_3D ( 'NONE', #37858, #33912, #49957 ) ;
#20096 = ORIENTED_EDGE ( 'NONE', *, *, #15348, .T. ) ;
#20097 = DIRECTION ( 'NONE',  ( 0.000000000000000000, -1.000000000000000000, 0.000000000000000000 ) ) ;
#20098 = ORIENTED_EDGE ( 'NONE', *, *, #46858, .T. ) ;
#20099 = EDGE_LOOP ( 'NONE', ( #29940, #33579, #8228, #32092 ) ) ;
#20100 = CARTESIAN_POINT ( 'NONE',  ( -336.3521761649654422, -123.5000000000000284, 0.000000000000000000 ) ) ;
#20102 = ORIENTED_EDGE ( 'NONE', *, *, #3213, .F. ) ;
#20101 = DIRECTION ( 'NONE',  ( 0.000000000000000000, -0.000000000000000000, -1.000000000000000000 ) ) ;
#20103 = ORIENTED_EDGE ( 'NONE', *, *, #16335, .F. ) ;
#20104 = DIRECTION ( 'NONE',  ( 0.000000000000000000, 0.000000000000000000, 1.000000000000000000 ) ) ;
#20105 = PLANE ( 'NONE',  #11702 ) ;
#20106 = ORIENTED_EDGE ( 'NONE', *, *, #45593, .T. ) ;
#20107 = CIRCLE ( 'NONE', #5847, 125.0000000000000000 ) ;
#20108 = LINE ( 'NONE', #16177, #39023 ) ;
#20109 = LINE ( 'NONE', #32192, #28678 ) ;
#20110 = ORIENTED_EDGE ( 'NONE', *, *, #25910, .T. ) ;
#20111 = CARTESIAN_POINT ( 'NONE',  ( 47.04848625005566731, -183.6283474603465606, 80.61932246194658092 ) ) ;
#20112 = CARTESIAN_POINT ( 'NONE',  ( -48.47912675150885065, -175.3837268820161057, 6.938893903907228378E-15 ) ) ;
#20113 = FACE_OUTER_BOUND ( 'NONE', #48483, .T. ) ;
#20114 = CARTESIAN_POINT ( 'NONE',  ( -336.3521761649654422, -175.3529239922484351, 30.18731974611377566 ) ) ;
#20115 = ORIENTED_EDGE ( 'NONE', *, *, #35337, .T. ) ;
#20116 = EDGE_LOOP ( 'NONE', ( #51617, #48604, #32705, #21517 ) ) ;
#20117 = ORIENTED_EDGE ( 'NONE', *, *, #38493, .T. ) ;
#20118 = CARTESIAN_POINT ( 'NONE',  ( -330.4913330509368166, -67.22367097967925531, -20.80804632820203537 ) ) ;
#20119 = CARTESIAN_POINT ( 'NONE',  ( 60.00000000000001421, -113.5000000000000000, -40.00000000000001421 ) ) ;
#20120 = FACE_OUTER_BOUND ( 'NONE', #5482, .T. ) ;
#20121 = FACE_BOUND ( 'NONE', #48102, .T. ) ;
#20122 = LINE ( 'NONE', #7532, #33931 ) ;
#20123 = EDGE_LOOP ( 'NONE', ( #39254, #296 ) ) ;
#20124 = ADVANCED_FACE ( 'NONE', ( #16558 ), #48344, .T. ) ;
#20125 = EDGE_CURVE ( 'NONE', #41700, #25155, #44409, .T. ) ;
#20126 = ADVANCED_FACE ( 'NONE', ( #4715 ), #40688, .T. ) ;
#20127 = AXIS2_PLACEMENT_3D ( 'NONE', #26282, #25780, #34436 ) ;
#20128 = AXIS2_PLACEMENT_3D ( 'NONE', #21921, #37943, #49788 ) ;
#20129 = DIRECTION ( 'NONE',  ( 0.000000000000000000, 1.000000000000000000, -0.000000000000000000 ) ) ;
#20130 = ORIENTED_EDGE ( 'NONE', *, *, #2947, .T. ) ;
#20132 = VERTEX_POINT ( 'NONE', #32036 ) ;
#20131 = DIRECTION ( 'NONE',  ( 0.000000000000000000, 1.000000000000000000, 0.000000000000000000 ) ) ;
#20133 = DIRECTION ( 'NONE',  ( 0.000000000000000000, 1.047444401652940007E-14, 1.000000000000000000 ) ) ;
#20134 = ORIENTED_EDGE ( 'NONE', *, *, #41035, .F. ) ;
#20135 = CARTESIAN_POINT ( 'NONE',  ( -47.66663987350317910, -193.5000000000000000, 0.5829794791144832233 ) ) ;
#20136 = EDGE_CURVE ( 'NONE', #33417, #47120, #18721, .T. ) ;
#20137 = FACE_OUTER_BOUND ( 'NONE', #14316, .T. ) ;
#20138 = DIRECTION ( 'NONE',  ( 0.000000000000000000, 2.361536891963093559E-13, -1.000000000000000000 ) ) ;
#20139 = DIRECTION ( 'NONE',  ( 1.000000000000000000, -0.000000000000000000, -0.000000000000000000 ) ) ;
#20140 = VERTEX_POINT ( 'NONE', #28086 ) ;
#20141 = EDGE_CURVE ( 'NONE', #51271, #8740, #31310, .T. ) ;
#20142 = DIRECTION ( 'NONE',  ( 0.000000000000000000, -1.000000000000000000, 0.000000000000000000 ) ) ;
#20143 = VERTEX_POINT ( 'NONE', #24176 ) ;
#20144 = EDGE_CURVE ( 'NONE', #19332, #11775, #49792, .T. ) ;
#20145 = ORIENTED_EDGE ( 'NONE', *, *, #6285, .T. ) ;
#20146 = DIRECTION ( 'NONE',  ( 0.000000000000000000, 0.000000000000000000, 1.000000000000000000 ) ) ;
#20147 = EDGE_CURVE ( 'NONE', #13215, #32692, #16207, .T. ) ;
#20148 = VECTOR ( 'NONE', #10543, 1000.000000000000114 ) ;
#20149 = CARTESIAN_POINT ( 'NONE',  ( 46.00000000000000711, 20.00000000000000000, 51.00000000000000000 ) ) ;
#20150 = DIRECTION ( 'NONE',  ( 0.000000000000000000, -1.000000000000000000, 0.000000000000000000 ) ) ;
#20151 = ADVANCED_FACE ( 'NONE', ( #17079 ), #36241, .F. ) ;
#20152 = DIRECTION ( 'NONE',  ( 0.000000000000000000, 2.498001805406602216E-14, -1.000000000000000000 ) ) ;
#20153 = CARTESIAN_POINT ( 'NONE',  ( -5.113431607746556473, -175.3837268820161057, 117.2365833888819679 ) ) ;
#20154 = ORIENTED_EDGE ( 'NONE', *, *, #1158, .T. ) ;
#20155 = CARTESIAN_POINT ( 'NONE',  ( -153.7737137892885073, -189.7472609257535510, -65.49088066501643368 ) ) ;
#20156 = FACE_OUTER_BOUND ( 'NONE', #15145, .T. ) ;
#20157 = FACE_BOUND ( 'NONE', #45741, .T. ) ;
#20158 = ORIENTED_EDGE ( 'NONE', *, *, #19201, .F. ) ;
#20159 = DIRECTION ( 'NONE',  ( 0.000000000000000000, 0.000000000000000000, -1.000000000000000000 ) ) ;
#20160 = CARTESIAN_POINT ( 'NONE',  ( -49.25565061422690150, -189.7472609257535510, 0.6300878435817109935 ) ) ;
#20161 = ORIENTED_EDGE ( 'NONE', *, *, #29663, .T. ) ;
#20162 = LINE ( 'NONE', #16494, #41377 ) ;
#20163 = ORIENTED_EDGE ( 'NONE', *, *, #11956, .T. ) ;
#20164 = ADVANCED_FACE ( 'NONE', ( #12059 ), #24679, .T. ) ;
#20165 = VECTOR ( 'NONE', #599, 1000.000000000000000 ) ;
#20166 = VECTOR ( 'NONE', #41546, 1000.000000000000000 ) ;
#20167 = CARTESIAN_POINT ( 'NONE',  ( -158.3442440847887269, -193.5000000000000000, -59.62093586438114556 ) ) ;
#20168 = FACE_BOUND ( 'NONE', #13408, .T. ) ;
#20170 = ORIENTED_EDGE ( 'NONE', *, *, #20205, .F. ) ;
#20169 = DIRECTION ( 'NONE',  ( 0.000000000000000000, 1.000000000000000000, 0.000000000000000000 ) ) ;
#20171 = CARTESIAN_POINT ( 'NONE',  ( -21.46839590530488451, -193.5000000000000000, 122.0467960216650738 ) ) ;
#20172 = ORIENTED_EDGE ( 'NONE', *, *, #29455, .T. ) ;
#20173 = EDGE_LOOP ( 'NONE', ( #19221, #7679, #37925, #47216 ) ) ;
#20174 = EDGE_CURVE ( 'NONE', #42501, #13947, #37025, .T. ) ;
#20175 = DIRECTION ( 'NONE',  ( -0.000000000000000000, 1.000000000000000000, -0.000000000000000000 ) ) ;
#20176 = VECTOR ( 'NONE', #19652, 1000.000000000000000 ) ;
#20177 = ORIENTED_EDGE ( 'NONE', *, *, #10895, .F. ) ;
#20178 = DIRECTION ( 'NONE',  ( 0.000000000000000000, 0.9709418174260511236, -0.2393156642875615969 ) ) ;
#20179 = CARTESIAN_POINT ( 'NONE',  ( 67.87295084395105960, -177.1207230881787780, 42.87565520599286373 ) ) ;
#20180 = EDGE_CURVE ( 'NONE', #33465, #25065, #24954, .T. ) ;
#20181 = ADVANCED_FACE ( 'NONE', ( #32567 ), #44920, .F. ) ;
#20182 = EDGE_CURVE ( 'NONE', #35111, #17063, #33083, .T. ) ;
#20183 = EDGE_CURVE ( 'NONE', #12564, #16597, #48618, .T. ) ;
#20184 = EDGE_CURVE ( 'NONE', #19790, #30079, #12848, .T. ) ;
#20185 = CARTESIAN_POINT ( 'NONE',  ( -336.3521761649654422, -125.1322888500942270, -59.00000000000002132 ) ) ;
#20186 = FACE_OUTER_BOUND ( 'NONE', #44837, .T. ) ;
#20187 = ORIENTED_EDGE ( 'NONE', *, *, #47820, .F. ) ;
#20190 = EDGE_LOOP ( 'NONE', ( #10435, #26782, #37687, #13821 ) ) ;
#20189 = FACE_OUTER_BOUND ( 'NONE', #49598, .T. ) ;
#20188 = DIRECTION ( 'NONE',  ( -1.000000000000000000, 0.000000000000000000, 0.000000000000000000 ) ) ;
#20191 = ORIENTED_EDGE ( 'NONE', *, *, #6409, .T. ) ;
#20192 = EDGE_CURVE ( 'NONE', #15949, #45202, #28872, .T. ) ;
#20193 = DIRECTION ( 'NONE',  ( -0.000000000000000000, 1.000000000000000000, -0.000000000000000000 ) ) ;
#20194 = VERTEX_POINT ( 'NONE', #9189 ) ;
#20195 = CARTESIAN_POINT ( 'NONE',  ( -173.4724443937511751, -193.5000000000000000, 1.292495564989516454 ) ) ;
#20196 = VECTOR ( 'NONE', #37932, 1000.000000000000000 ) ;
#20197 = VERTEX_POINT ( 'NONE', #21528 ) ;
#20198 = DIRECTION ( 'NONE',  ( 0.9151456172430153524, 0.000000000000000000, 0.4031234292879792847 ) ) ;
#20199 = ORIENTED_EDGE ( 'NONE', *, *, #5861, .F. ) ;
#20200 = EDGE_CURVE ( 'NONE', #32592, #50673, #41759, .T. ) ;
#20202 = CARTESIAN_POINT ( 'NONE',  ( -134.2540868116286958, -189.7472609257535510, 89.54698061029652933 ) ) ;
#20201 = PLANE ( 'NONE',  #6543 ) ;
#20203 = VERTEX_POINT ( 'NONE', #45982 ) ;
#20204 = VECTOR ( 'NONE', #51813, 1000.000000000000114 ) ;
#20205 = EDGE_CURVE ( 'NONE', #12928, #35455, #15681, .T. ) ;
#20206 = CIRCLE ( 'NONE', #3429, 125.0000000000000000 ) ;
#20207 = ORIENTED_EDGE ( 'NONE', *, *, #51956, .F. ) ;
#20208 = CARTESIAN_POINT ( 'NONE',  ( -332.3517673607765914, -181.7525362123217292, 9.724760635742144999 ) ) ;
#20209 = CARTESIAN_POINT ( 'NONE',  ( -170.0000000000000284, -113.5000000000000000, -40.00000000000001421 ) ) ;
#20210 = EDGE_CURVE ( 'NONE', #9746, #41712, #5248, .T. ) ;
#20211 = CARTESIAN_POINT ( 'NONE',  ( -305.0000000000000568, -159.7173995167596274, -47.83617848703448772 ) ) ;
#20212 = CARTESIAN_POINT ( 'NONE',  ( 48.69345348225014902, -175.3837268820161057, -78.62880929222872339 ) ) ;
#20213 = CARTESIAN_POINT ( 'NONE',  ( -107.6930423737362190, -183.6283474603465606, 110.0850225811110761 ) ) ;
#20214 = DIRECTION ( 'NONE',  ( 0.000000000000000000, 0.000000000000000000, 1.000000000000000000 ) ) ;
#20215 = EDGE_CURVE ( 'NONE', #48966, #28239, #22035, .T. ) ;
#20216 = ORIENTED_EDGE ( 'NONE', *, *, #41954, .F. ) ;
#20217 = SHAPE_DEFINITION_REPRESENTATION ( #41509, #6277 ) ;
#20218 = CARTESIAN_POINT ( 'NONE',  ( -173.0003472773501301, -189.7472609257535510, 10.93003379476953896 ) ) ;
#20219 = PLANE ( 'NONE',  #3840 ) ;
#20220 = EDGE_CURVE ( 'NONE', #12568, #2342, #18189, .T. ) ;
#20221 = DIRECTION ( 'NONE',  ( 0.7765238627180349740, 0.000000000000000000, 0.6300878435817203194 ) ) ;
#20222 = VERTEX_POINT ( 'NONE', #30189 ) ;
#20223 = VECTOR ( 'NONE', #47214, 1000.000000000000000 ) ;
#20224 = DIRECTION ( 'NONE',  ( -0.000000000000000000, 1.000000000000000000, -0.000000000000000000 ) ) ;
#20225 = LINE ( 'NONE', #28876, #42860 ) ;
#20226 = CARTESIAN_POINT ( 'NONE',  ( -336.3521761649654422, -123.5000000000000284, 0.000000000000000000 ) ) ;
#20227 = ORIENTED_EDGE ( 'NONE', *, *, #25178, .F. ) ;
#20228 = ORIENTED_EDGE ( 'NONE', *, *, #30897, .F. ) ;
#20229 = ORIENTED_EDGE ( 'NONE', *, *, #7635, .F. ) ;
#20230 = EDGE_CURVE ( 'NONE', #1228, #30377, #10606, .T. ) ;
#20231 = EDGE_CURVE ( 'NONE', #25977, #44982, #37801, .T. ) ;
#20232 = CARTESIAN_POINT ( 'NONE',  ( -330.4913330509368166, -130.1153096980153236, -58.63009191191284941 ) ) ;
#20233 = DIRECTION ( 'NONE',  ( 0.7948544414133565938, 0.000000000000000000, -0.6068001458185890984 ) ) ;
#20234 = LINE ( 'NONE', #39422, #11115 ) ;
#20235 = LINE ( 'NONE', #24970, #1038 ) ;
#20236 = AXIS2_PLACEMENT_3D ( 'NONE', #39978, #44467, #36054 ) ;
#20237 = ORIENTED_EDGE ( 'NONE', *, *, #36577, .F. ) ;
#20238 = LINE ( 'NONE', #49420, #24351 ) ;
#20239 = EDGE_LOOP ( 'NONE', ( #29190, #22818, #10532, #51371 ) ) ;
#20240 = AXIS2_PLACEMENT_3D ( 'NONE', #44859, #12787, #40908 ) ;
#20241 = VERTEX_POINT ( 'NONE', #37289 ) ;
#20242 = ORIENTED_EDGE ( 'NONE', *, *, #19059, .F. ) ;
#20243 = DIRECTION ( 'NONE',  ( 0.000000000000000000, -1.000000000000000000, 0.000000000000000000 ) ) ;
#20244 = EDGE_CURVE ( 'NONE', #46197, #27750, #25724, .T. ) ;
#20245 = EDGE_CURVE ( 'NONE', #50634, #8813, #49393, .T. ) ;
#20246 = ORIENTED_EDGE ( 'NONE', *, *, #18302, .F. ) ;
#20247 = ADVANCED_FACE ( 'NONE', ( #29918 ), #33861, .F. ) ;
#20248 = DIRECTION ( 'NONE',  ( 0.000000000000000000, 1.000000000000000000, -0.000000000000000000 ) ) ;
#20249 = DIRECTION ( 'NONE',  ( 0.000000000000000000, 0.000000000000000000, -1.000000000000000000 ) ) ;
#20252 = VERTEX_POINT ( 'NONE', #41220 ) ;
#20251 = DIRECTION ( 'NONE',  ( -0.000000000000000000, 1.000000000000000000, -0.000000000000000000 ) ) ;
#20250 = CARTESIAN_POINT ( 'NONE',  ( -105.2524431885210987, -193.5000000000000000, 110.2396968984195382 ) ) ;
#20253 = CIRCLE ( 'NONE', #42909, 125.0000000000000000 ) ;
#20254 = CARTESIAN_POINT ( 'NONE',  ( -330.4913330509368166, -122.9999999999994600, 59.00000000000002132 ) ) ;
#20255 = ORIENTED_EDGE ( 'NONE', *, *, #37180, .F. ) ;
#20256 = CARTESIAN_POINT ( 'NONE',  ( 74.28166149629942083, -175.3837268820161057, 17.48697739784543259 ) ) ;
#20257 = ORIENTED_EDGE ( 'NONE', *, *, #27458, .F. ) ;
#20258 = FACE_OUTER_BOUND ( 'NONE', #29873, .T. ) ;
#20259 = DIRECTION ( 'NONE',  ( 0.000000000000000000, 0.9350162426854132791, -0.3546048870425396182 ) ) ;
#20261 = CARTESIAN_POINT ( 'NONE',  ( 17.98688506184922176, -193.5000000000000000, 104.6823626202124586 ) ) ;
#20260 = PLANE ( 'NONE',  #40872 ) ;
#20262 = ORIENTED_EDGE ( 'NONE', *, *, #15398, .T. ) ;
#20263 = LINE ( 'NONE', #11334, #6382 ) ;
#20264 = LINE ( 'NONE', #40485, #39574 ) ;
#20265 = ORIENTED_EDGE ( 'NONE', *, *, #24896, .F. ) ;
#20266 = EDGE_CURVE ( 'NONE', #29097, #47521, #29397, .T. ) ;
#20267 = DIRECTION ( 'NONE',  ( 0.8757349421956345248, 0.000000000000000000, 0.4827922027307490205 ) ) ;
#20268 = CARTESIAN_POINT ( 'NONE',  ( -48.24424070572786860, -175.3837268820161057, -0.9720229140804037549 ) ) ;
#20269 = AXIS2_PLACEMENT_3D ( 'NONE', #51151, #23523, #7237 ) ;
#20270 = DIRECTION ( 'NONE',  ( 0.000000000000000000, 0.6631226582407911962, -0.7485107481711046340 ) ) ;
#20271 = EDGE_LOOP ( 'NONE', ( #2434, #9735, #14189, #29535 ) ) ;
#20272 = CARTESIAN_POINT ( 'NONE',  ( -103.4012653778457462, -193.5000000000000000, -112.2878385610366649 ) ) ;
#20273 = VECTOR ( 'NONE', #7296, 1000.000000000000000 ) ;
#20274 = CARTESIAN_POINT ( 'NONE',  ( -332.3517673607765914, -141.9604555052315220, 56.09938080879057765 ) ) ;
#20275 = EDGE_CURVE ( 'NONE', #1349, #12927, #18098, .T. ) ;
#20276 = ORIENTED_EDGE ( 'NONE', *, *, #41565, .T. ) ;
#20277 = DIRECTION ( 'NONE',  ( 0.000000000000000000, -0.5680647467311625842, -0.8229838658936516893 ) ) ;
#20278 = ORIENTED_EDGE ( 'NONE', *, *, #51904, .T. ) ;
#20279 = CARTESIAN_POINT ( 'NONE',  ( -332.3517673607765914, -123.5000000000000284, 0.000000000000000000 ) ) ;
#20280 = CARTESIAN_POINT ( 'NONE',  ( -49.44376233341721161, -193.5000000000000000, 0.2635871660690650709 ) ) ;
#20281 = LINE ( 'NONE', #51085, #44518 ) ;
#20282 = CARTESIAN_POINT ( 'NONE',  ( -82.67254833784559764, -193.5000000000000000, -120.2323164553483963 ) ) ;
#20283 = CARTESIAN_POINT ( 'NONE',  ( -305.0000000000000568, -123.5000000000000284, 0.000000000000000000 ) ) ;
#20284 = VECTOR ( 'NONE', #10093, 1000.000000000000000 ) ;
#20285 = PLANE ( 'NONE',  #17088 ) ;
#20286 = AXIS2_PLACEMENT_3D ( 'NONE', #10300, #50513, #51286 ) ;
#20287 = DIRECTION ( 'NONE',  ( 0.000000000000000000, -1.000000000000000000, 0.000000000000000000 ) ) ;
#20288 = CARTESIAN_POINT ( 'NONE',  ( -330.4913330509368166, -156.6043281241909995, 48.84008046109159551 ) ) ;
#20290 = VERTEX_POINT ( 'NONE', #34124 ) ;
#20289 = CARTESIAN_POINT ( 'NONE',  ( -167.1580984288390823, -189.7472609257535510, -39.24667733211878584 ) ) ;
#20291 = ORIENTED_EDGE ( 'NONE', *, *, #34453, .T. ) ;
#20292 = DIRECTION ( 'NONE',  ( 0.000000000000000000, 0.000000000000000000, 1.000000000000000000 ) ) ;
#20293 = DIRECTION ( 'NONE',  ( 0.000000000000000000, -1.000000000000000000, -0.000000000000000000 ) ) ;
#20294 = VERTEX_POINT ( 'NONE', #25465 ) ;
#20295 = EDGE_LOOP ( 'NONE', ( #18145, #34670, #24405, #14174 ) ) ;
#20296 = ORIENTED_EDGE ( 'NONE', *, *, #30880, .T. ) ;
#20297 = CARTESIAN_POINT ( 'NONE',  ( 71.97629403264902237, -183.6283474603465606, -29.43839964798649333 ) ) ;
#20298 = CIRCLE ( 'NONE', #4367, 124.9999999999999858 ) ;
#20299 = ADVANCED_FACE ( 'NONE', ( #41481 ), #33608, .F. ) ;
#20300 = DIRECTION ( 'NONE',  ( 0.000000000000000000, 0.9709418174260493473, -0.2393156642875685913 ) ) ;
#20301 = CARTESIAN_POINT ( 'NONE',  ( -48.98765787015805984, -189.7472609257535510, -0.8610436117673551104 ) ) ;
#20302 = AXIS2_PLACEMENT_3D ( 'NONE', #4576, #32170, #48992 ) ;
#20303 = VERTEX_POINT ( 'NONE', #42256 ) ;
#20304 = ORIENTED_EDGE ( 'NONE', *, *, #14110, .F. ) ;
#20305 = EDGE_LOOP ( 'NONE', ( #37159, #17230, #5456, #20145 ) ) ;
#20306 = CARTESIAN_POINT ( 'NONE',  ( 48.69345348225014902, -175.3837268820161057, -78.62880929222872339 ) ) ;
#20307 = DIRECTION ( 'NONE',  ( 1.000000000000000000, -0.000000000000000000, -0.000000000000000000 ) ) ;
#20309 = ORIENTED_EDGE ( 'NONE', *, *, #46629, .T. ) ;
#20308 = CARTESIAN_POINT ( 'NONE',  ( -157.8637630444124795, -193.5000000000000000, -60.49794494914009135 ) ) ;
#20310 = DIRECTION ( 'NONE',  ( 0.000000000000000000, 0.5680647467311510379, -0.8229838658936596829 ) ) ;
#20311 = DIRECTION ( 'NONE',  ( -0.000000000000000000, -1.000000000000000000, 0.000000000000000000 ) ) ;
#20312 = ORIENTED_EDGE ( 'NONE', *, *, #23713, .F. ) ;
#20313 = DIRECTION ( 'NONE',  ( -0.000000000000000000, 1.000000000000000000, 0.000000000000000000 ) ) ;
#20314 = FACE_OUTER_BOUND ( 'NONE', #51064, .T. ) ;
#20315 = DIRECTION ( 'NONE',  ( 0.000000000000000000, 0.000000000000000000, -1.000000000000000000 ) ) ;
#20316 = CARTESIAN_POINT ( 'NONE',  ( -121.1142239062970418, -193.5000000000000000, 101.7307360698549132 ) ) ;
#20317 = AXIS2_PLACEMENT_3D ( 'NONE', #45776, #25801, #41832 ) ;
#20318 = ORIENTED_EDGE ( 'NONE', *, *, #34681, .T. ) ;
#20319 = VERTEX_POINT ( 'NONE', #29656 ) ;
#20320 = TOROIDAL_SURFACE ( 'NONE', #7728, 1.951623109906645004, 10.00000000000000000 ) ;
#20321 = EDGE_LOOP ( 'NONE', ( #26987, #6254, #44380, #36730 ) ) ;
#20322 = VECTOR ( 'NONE', #604, 1000.000000000000114 ) ;
#20323 = CARTESIAN_POINT ( 'NONE',  ( -48.47912675150885065, -183.6283474603465606, 6.938893903907228378E-15 ) ) ;
#20324 = DIRECTION ( 'NONE',  ( 0.000000000000000000, 0.000000000000000000, 1.000000000000000000 ) ) ;
#20325 = ORIENTED_EDGE ( 'NONE', *, *, #15114, .T. ) ;
#20326 = EDGE_CURVE ( 'NONE', #2316, #23737, #41655, .T. ) ;
#20327 = DIRECTION ( 'NONE',  ( 0.000000000000000000, 0.000000000000000000, 1.000000000000000000 ) ) ;
#20328 = DIRECTION ( 'NONE',  ( 0.3482016354343928088, 0.000000000000000000, 0.9374196611341231167 ) ) ;
#20329 = ORIENTED_EDGE ( 'NONE', *, *, #45493, .F. ) ;
#20330 = DIRECTION ( 'NONE',  ( -0.000000000000000000, 1.000000000000000000, -0.000000000000000000 ) ) ;
#20331 = ORIENTED_EDGE ( 'NONE', *, *, #9347, .T. ) ;
#20332 = DIRECTION ( 'NONE',  ( 0.8896570909947436601, 0.000000000000000000, 0.4566292373937200777 ) ) ;
#20333 = ORIENTED_EDGE ( 'NONE', *, *, #48755, .F. ) ;
#20334 = DIRECTION ( 'NONE',  ( -0.000000000000000000, 1.000000000000000000, -0.000000000000000000 ) ) ;
#20335 = FACE_BOUND ( 'NONE', #45707, .T. ) ;
#20336 = CARTESIAN_POINT ( 'NONE',  ( -332.3517673607765914, -146.8829211657874794, -54.23253582808848705 ) ) ;
#20337 = EDGE_CURVE ( 'NONE', #30471, #23668, #45706, .T. ) ;
#20338 = ORIENTED_EDGE ( 'NONE', *, *, #24629, .T. ) ;
#20339 = VECTOR ( 'NONE', #38814, 1000.000000000000000 ) ;
#20340 = DIRECTION ( 'NONE',  ( -0.000000000000000000, 1.000000000000000000, -0.000000000000000000 ) ) ;
#20341 = DIRECTION ( 'NONE',  ( 0.000000000000000000, 0.000000000000000000, 1.000000000000000000 ) ) ;
#20342 = DIRECTION ( 'NONE',  ( 0.000000000000000000, -0.000000000000000000, -1.000000000000000000 ) ) ;
#20343 = EDGE_CURVE ( 'NONE', #210, #11500, #16502, .T. ) ;
#20344 = CARTESIAN_POINT ( 'NONE',  ( -96.65280530915693191, -183.6283474603465606, -115.3442529744087466 ) ) ;
#20345 = CIRCLE ( 'NONE', #5295, 125.0000000000000000 ) ;
#20346 = ORIENTED_EDGE ( 'NONE', *, *, #46117, .F. ) ;
#20347 = DIRECTION ( 'NONE',  ( 0.000000000000000000, -0.000000000000000000, -1.000000000000000000 ) ) ;
#20348 = ORIENTED_EDGE ( 'NONE', *, *, #6026, .F. ) ;
#20349 = EDGE_LOOP ( 'NONE', ( #45410, #1650, #28695, #13457 ) ) ;
#20350 = ADVANCED_FACE ( 'NONE', ( #50431 ), #29139, .F. ) ;
#20351 = CARTESIAN_POINT ( 'NONE',  ( -305.0000000000000568, -88.08538291676191534, 48.43351006119235080 ) ) ;
#20353 = VERTEX_POINT ( 'NONE', #19386 ) ;
#20352 = PLANE ( 'NONE',  #45475 ) ;
#20354 = ORIENTED_EDGE ( 'NONE', *, *, #5598, .F. ) ;
#20355 = DIRECTION ( 'NONE',  ( -0.000000000000000000, 0.9927088740980538617, -0.1205366802553232974 ) ) ;
#20356 = VECTOR ( 'NONE', #49145, 1000.000000000000000 ) ;
#20357 = AXIS2_PLACEMENT_3D ( 'NONE', #49826, #6713, #9611 ) ;
#20358 = EDGE_CURVE ( 'NONE', #32858, #39920, #51457, .T. ) ;
#20359 = LINE ( 'NONE', #44020, #32679 ) ;
#20360 = AXIS2_PLACEMENT_3D ( 'NONE', #33791, #26155, #13830 ) ;
#20361 = AXIS2_PLACEMENT_3D ( 'NONE', #51522, #47591, #51028 ) ;
#20362 = EDGE_LOOP ( 'NONE', ( #21992, #479, #32768, #40921 ) ) ;
#20363 = DIRECTION ( 'NONE',  ( -0.000000000000000000, 0.4647231720437664526, -0.8854560256532110207 ) ) ;
#20364 = CARTESIAN_POINT ( 'NONE',  ( -48.88225018079680950, -177.1207230881787780, -0.9151456172430169067 ) ) ;
#20365 = ORIENTED_EDGE ( 'NONE', *, *, #40345, .F. ) ;
#20366 = DIRECTION ( 'NONE',  ( 0.000000000000000000, 0.000000000000000000, 1.000000000000000000 ) ) ;
#20367 = DIRECTION ( 'NONE',  ( -0.000000000000000000, 1.000000000000000000, -0.000000000000000000 ) ) ;
#20368 = ADVANCED_FACE ( 'NONE', ( #31207 ), #39082, .F. ) ;
#20369 = CARTESIAN_POINT ( 'NONE',  ( 59.29945538372744807, -193.5000000000000000, 63.31490529818492519 ) ) ;
#20370 = LINE ( 'NONE', #36395, #38329 ) ;
#20371 = ORIENTED_EDGE ( 'NONE', *, *, #17325, .F. ) ;
#20372 = ORIENTED_EDGE ( 'NONE', *, *, #19856, .F. ) ;
#20373 = EDGE_CURVE ( 'NONE', #4643, #7784, #42786, .T. ) ;
#20374 = ORIENTED_EDGE ( 'NONE', *, *, #17818, .T. ) ;
#20375 = LINE ( 'NONE', #40593, #10638 ) ;
#20376 = CARTESIAN_POINT ( 'NONE',  ( -48.47912675150885065, -120.5000000000000284, 14.00000000000001776 ) ) ;
#20377 = ADVANCED_FACE ( 'NONE', ( #2586 ), #3094, .T. ) ;
#20378 = PLANE ( 'NONE',  #30988 ) ;
#20379 = FACE_BOUND ( 'NONE', #21645, .T. ) ;
#20380 = FACE_OUTER_BOUND ( 'NONE', #24912, .T. ) ;
#20381 = VECTOR ( 'NONE', #51195, 1000.000000000000227 ) ;
#20382 = ORIENTED_EDGE ( 'NONE', *, *, #48, .F. ) ;
#20383 = VECTOR ( 'NONE', #38200, 1000.000000000000000 ) ;
#20384 = VERTEX_POINT ( 'NONE', #27003 ) ;
#20386 = ORIENTED_EDGE ( 'NONE', *, *, #25036, .T. ) ;
#20385 = CARTESIAN_POINT ( 'NONE',  ( -48.47912675150885065, -117.5479369270332057, 6.938893903907228378E-15 ) ) ;
#20387 = DIRECTION ( 'NONE',  ( 0.000000000000000000, -1.000000000000000000, 1.047444401652940007E-14 ) ) ;
#20388 = ORIENTED_EDGE ( 'NONE', *, *, #4258, .T. ) ;
#20389 = CARTESIAN_POINT ( 'NONE',  ( 61.06976976088562026, -193.5000000000000000, -60.19999396110170409 ) ) ;
#20390 = EDGE_CURVE ( 'NONE', #10059, #32964, #27397, .T. ) ;
#20391 = CARTESIAN_POINT ( 'NONE',  ( -339.1964088526558498, -74.65991953890876687, -33.10432812419148263 ) ) ;
#20392 = DIRECTION ( 'NONE',  ( -0.2635871660690648488, 0.000000000000000000, -0.9646355819083595184 ) ) ;
#20393 = CARTESIAN_POINT ( 'NONE',  ( -78.41101675714243413, -193.5000000000000000, -120.3332351033023286 ) ) ;
#20394 = ORIENTED_EDGE ( 'NONE', *, *, #14238, .F. ) ;
#20395 = LINE ( 'NONE', #32748, #14958 ) ;
#20396 = CIRCLE ( 'NONE', #5304, 125.0000000000000000 ) ;
#20397 = ORIENTED_EDGE ( 'NONE', *, *, #49697, .F. ) ;
#20398 = VECTOR ( 'NONE', #36727, 1000.000000000000000 ) ;
#20399 = EDGE_LOOP ( 'NONE', ( #5801, #16696, #29404, #40173 ) ) ;
#20400 = LINE ( 'NONE', #24105, #13675 ) ;
#20401 = VECTOR ( 'NONE', #8889, 1000.000000000000000 ) ;
#20402 = CARTESIAN_POINT ( 'NONE',  ( 76.47090317495664635, -175.3837268820161057, -3.534122433557446374 ) ) ;
#20403 = DIRECTION ( 'NONE',  ( -0.4300652022765304450, 0.000000000000000000, 0.9027978299657387629 ) ) ;
#20404 = CARTESIAN_POINT ( 'NONE',  ( -153.7332855749581881, -189.7472609257535510, 67.42819922234390617 ) ) ;
#20405 = CARTESIAN_POINT ( 'NONE',  ( -330.4913330509368166, -150.9396941197155968, -53.35787839313373837 ) ) ;
#20406 = LINE ( 'NONE', #32501, #48053 ) ;
#20407 = AXIS2_PLACEMENT_3D ( 'NONE', #19645, #32773, #40636 ) ;
#20408 = ORIENTED_EDGE ( 'NONE', *, *, #10525, .T. ) ;
#20409 = DIRECTION ( 'NONE',  ( -0.4566292373937140270, 0.000000000000000000, 0.8896570909947467687 ) ) ;
#20410 = LINE ( 'NONE', #36431, #13143 ) ;
#20411 = CARTESIAN_POINT ( 'NONE',  ( 72.12732647922463514, -177.1207230881787780, 28.81338593824055749 ) ) ;
#20412 = FACE_BOUND ( 'NONE', #45069, .T. ) ;
#20413 = ORIENTED_EDGE ( 'NONE', *, *, #2432, .F. ) ;
#20414 = LINE ( 'NONE', #39854, #4632 ) ;
#20415 = VECTOR ( 'NONE', #38634, 1000.000000000000000 ) ;
#20416 = DIRECTION ( 'NONE',  ( -0.5315839928299663786, 0.000000000000000000, 0.8470055835512245723 ) ) ;
#20417 = EDGE_CURVE ( 'NONE', #50110, #39155, #8090, .T. ) ;
#20418 = EDGE_LOOP ( 'NONE', ( #38524, #12295, #9741, #42561 ) ) ;
#20419 = EDGE_CURVE ( 'NONE', #6309, #42116, #27525, .T. ) ;
#20420 = CARTESIAN_POINT ( 'NONE',  ( -107.6930423737362190, -193.5000000000000000, 110.0850225811110761 ) ) ;
#20421 = ORIENTED_EDGE ( 'NONE', *, *, #34319, .F. ) ;
#20422 = VECTOR ( 'NONE', #33445, 1000.000000000000114 ) ;
#20423 = CARTESIAN_POINT ( 'NONE',  ( 74.31448861501726810, -177.1207230881787780, -23.38221600314288651 ) ) ;
#20424 = FACE_BOUND ( 'NONE', #36166, .T. ) ;
#20426 = ORIENTED_EDGE ( 'NONE', *, *, #38834, .T. ) ;
#20425 = FACE_OUTER_BOUND ( 'NONE', #10842, .T. ) ;
#20427 = EDGE_CURVE ( 'NONE', #8625, #17957, #38832, .T. ) ;
#20429 = VECTOR ( 'NONE', #18463, 1000.000000000000000 ) ;
#20428 = CARTESIAN_POINT ( 'NONE',  ( 37.29583330861160562, -175.3837268820161057, -89.54698061029594669 ) ) ;
#20430 = ORIENTED_EDGE ( 'NONE', *, *, #27606, .F. ) ;
#20431 = EDGE_CURVE ( 'NONE', #10147, #47473, #30953, .T. ) ;
#20432 = VERTEX_POINT ( 'NONE', #23582 ) ;
#20433 = DIRECTION ( 'NONE',  ( -0.000000000000000000, 1.000000000000000000, -0.000000000000000000 ) ) ;
#20434 = AXIS2_PLACEMENT_3D ( 'NONE', #23049, #51966, #31962 ) ;
#20435 = EDGE_CURVE ( 'NONE', #16247, #14954, #21533, .T. ) ;
#20436 = EDGE_LOOP ( 'NONE', ( #17559, #16411, #25534, #38462 ) ) ;
#20437 = CARTESIAN_POINT ( 'NONE',  ( -149.1282321233095445, -193.5000000000000000, -72.42760398749011586 ) ) ;
#20438 = PLANE ( 'NONE',  #23626 ) ;
#20439 = DIRECTION ( 'NONE',  ( 0.000000000000000000, 0.000000000000000000, 1.000000000000000000 ) ) ;
#20440 = ADVANCED_FACE ( 'NONE', ( #22568 ), #19640, .F. ) ;
#20441 = FACE_OUTER_BOUND ( 'NONE', #23089, .T. ) ;
#20442 = FACE_OUTER_BOUND ( 'NONE', #44775, .T. ) ;
#20443 = ORIENTED_EDGE ( 'NONE', *, *, #34639, .F. ) ;
#20446 = EDGE_LOOP ( 'NONE', ( #21611, #6401 ) ) ;
#20445 = CARTESIAN_POINT ( 'NONE',  ( -142.3192003680973130, -183.6283474603465606, 82.57748230379306165 ) ) ;
#20444 = DIRECTION ( 'NONE',  ( 0.000000000000000000, 1.000000000000000000, 0.000000000000000000 ) ) ;
#20447 = ORIENTED_EDGE ( 'NONE', *, *, #49090, .F. ) ;
#20448 = DIRECTION ( 'NONE',  ( -0.7575112421616284619, 0.000000000000000000, 0.6528221181905119463 ) ) ;
#20449 = ORIENTED_EDGE ( 'NONE', *, *, #21815, .T. ) ;
#20450 = FACE_OUTER_BOUND ( 'NONE', #34550, .T. ) ;
#20451 = VECTOR ( 'NONE', #44346, 1000.000000000000114 ) ;
#20452 = ORIENTED_EDGE ( 'NONE', *, *, #8460, .F. ) ;
#20453 = PLANE ( 'NONE',  #37173 ) ;
#20454 = CARTESIAN_POINT ( 'NONE',  ( -140.0851925571752474, -193.5000000000000000, 83.57229767764225414 ) ) ;
#20455 = VERTEX_POINT ( 'NONE', #6544 ) ;
#20457 = CARTESIAN_POINT ( 'NONE',  ( -92.16375985330356002, -193.5000000000000000, 117.1181148702521710 ) ) ;
#20456 = LINE ( 'NONE', #476, #21616 ) ;
#20458 = ORIENTED_EDGE ( 'NONE', *, *, #8818, .T. ) ;
#20459 = AXIS2_PLACEMENT_3D ( 'NONE', #2263, #42184, #14878 ) ;
#20460 = VERTEX_POINT ( 'NONE', #38582 ) ;
#20461 = FACE_OUTER_BOUND ( 'NONE', #20418, .T. ) ;
#20462 = FACE_OUTER_BOUND ( 'NONE', #17983, .T. ) ;
#20463 = CARTESIAN_POINT ( 'NONE',  ( -169.9883746053192795, -175.3837268820161057, -24.72869175143020826 ) ) ;
#20464 = DIRECTION ( 'NONE',  ( 0.000000000000000000, -0.7485107481711089639, -0.6631226582407863113 ) ) ;
#20465 = CARTESIAN_POINT ( 'NONE',  ( -48.47912675150885065, -189.7472609257535510, 6.938893903907228378E-15 ) ) ;
#20466 = CARTESIAN_POINT ( 'NONE',  ( -332.3517673607765914, -170.5607375887735770, 35.68215131113770155 ) ) ;
#20467 = PRODUCT_CONTEXT ( 'NONE', #7870, 'mechanical' ) ;
#20468 = DIRECTION ( 'NONE',  ( -0.8757349421956412971, 0.000000000000000000, 0.4827922027307366970 ) ) ;
#20469 = AXIS2_PLACEMENT_3D ( 'NONE', #26449, #14134, #11200 ) ;
#20470 = CARTESIAN_POINT ( 'NONE',  ( -336.3521761649654422, -97.52665284734005979, -53.00046796564681983 ) ) ;
#20471 = FACE_OUTER_BOUND ( 'NONE', #12522, .T. ) ;
#20472 = DIRECTION ( 'NONE',  ( 0.000000000000000000, 0.000000000000000000, -1.000000000000000000 ) ) ;
#20473 = VERTEX_POINT ( 'NONE', #19137 ) ;
#20474 = CARTESIAN_POINT ( 'NONE',  ( 61.06976976088562026, -175.3837268820161057, -60.19999396110170409 ) ) ;
#20475 = EDGE_CURVE ( 'NONE', #45648, #36788, #35152, .T. ) ;
#20476 = DIRECTION ( 'NONE',  ( 0.000000000000000000, 0.000000000000000000, -1.000000000000000000 ) ) ;
#20477 = CARTESIAN_POINT ( 'NONE',  ( -53.47502265695602119, -177.1207230881787780, -124.9001241957025883 ) ) ;
#20478 = ADVANCED_FACE ( 'NONE', ( #3356, #50677, #26486, #31464, #30682, #51207, #15196, #43297, #26751, #11492, #43560, #6794, #22817, #20157, #12780, #48283, #32765, #48558, #20676, #12263, #176, #24364, #28297, #44349, #28031, #15719, #24881, #23841, #4388, #3876, #28806, #8340, #36712, #40369, #31979, #44594, #43808, #8844, #24614, #31734, #16224, #4650, #44855, #47772, #40128, #28550, #7809, #48810, #16485, #20412, #4145, #11747, #20949, #36435, #32507, #715, #434, #12533, #8583, #39852, #40628, #48019, #40900, #19902, #4925, #16760, #24117, #51714, #15971, #44073, #8073, #12002, #35935, #27773, #51986, #36180, #32238, #13569, #41682, #49586, #959, #45904, #17009, #29067, #41419, #33796, #49061, #9379, #5707, #33018, #25404, #37482, #13044, #45133, #25150, #45645, #41164, #36968, #49843, #17535, #9122, #29592, #21199, #5184, #37741, #9897 ), #45386, .T. ) ;
#20479 = ORIENTED_EDGE ( 'NONE', *, *, #23099, .T. ) ;
#20480 = EDGE_CURVE ( 'NONE', #15659, #24073, #5442, .T. ) ;
#20481 = EDGE_LOOP ( 'NONE', ( #49731, #35441, #12968, #17843 ) ) ;
#20482 = ADVANCED_FACE ( 'NONE', ( #33548 ), #17267, .F. ) ;
#20483 = FACE_OUTER_BOUND ( 'NONE', #25128, .T. ) ;
#20484 = EDGE_CURVE ( 'NONE', #13937, #41128, #21724, .T. ) ;
#20485 = PLANE ( 'NONE',  #164 ) ;
#20486 = CARTESIAN_POINT ( 'NONE',  ( -80.17897391495031911, -193.5000000000000000, 120.9136869416132498 ) ) ;
#20487 = CARTESIAN_POINT ( 'NONE',  ( -48.47912675150885065, -183.6283474603465606, 6.938893903907228378E-15 ) ) ;
#20488 = ORIENTED_EDGE ( 'NONE', *, *, #35247, .F. ) ;
#20489 = VECTOR ( 'NONE', #33345, 1000.000000000000000 ) ;
#20490 = CARTESIAN_POINT ( 'NONE',  ( -305.0000000000000568, -180.1590281025188460, -19.74220186498920881 ) ) ;
#20491 = EDGE_CURVE ( 'NONE', #41453, #27204, #3894, .T. ) ;
#20492 = DIRECTION ( 'NONE',  ( 0.000000000000000000, -0.000000000000000000, 1.000000000000000000 ) ) ;
#20493 = ORIENTED_EDGE ( 'NONE', *, *, #46917, .T. ) ;
#20494 = AXIS2_PLACEMENT_3D ( 'NONE', #5371, #17195, #890 ) ;
#20495 = EDGE_CURVE ( 'NONE', #43377, #38337, #29335, .T. ) ;
#20496 = DIRECTION ( 'NONE',  ( 0.9473263538541946138, 0.000000000000000000, -0.3202698538628279690 ) ) ;
#20497 = ORIENTED_EDGE ( 'NONE', *, *, #10394, .F. ) ;
#20498 = EDGE_CURVE ( 'NONE', #16257, #1746, #5954, .T. ) ;
#20499 = EDGE_LOOP ( 'NONE', ( #28916, #5367, #18001, #46275 ) ) ;
#20500 = CARTESIAN_POINT ( 'NONE',  ( -330.0000000000000568, -123.5000000000000284, 0.000000000000000000 ) ) ;
#20501 = ADVANCED_FACE ( 'NONE', ( #32404 ), #20695, .T. ) ;
#20502 = VECTOR ( 'NONE', #42940, 1000.000000000000114 ) ;
#20503 = EDGE_CURVE ( 'NONE', #17442, #46449, #50086, .T. ) ;
#20504 = DIRECTION ( 'NONE',  ( 0.08879589532292483933, 0.000000000000000000, 0.9960498426152178952 ) ) ;
#20505 = DIRECTION ( 'NONE',  ( 0.6528221181905174975, 0.000000000000000000, 0.7575112421616236880 ) ) ;
#20508 = ORIENTED_EDGE ( 'NONE', *, *, #48145, .T. ) ;
#20507 = FACE_OUTER_BOUND ( 'NONE', #39218, .T. ) ;
#20506 = CARTESIAN_POINT ( 'NONE',  ( 69.66827051661184100, -175.3837268820161057, -40.81902153125259503 ) ) ;
#20509 = LINE ( 'NONE', #28645, #48279 ) ;
#20510 = EDGE_LOOP ( 'NONE', ( #7524, #38193, #27343, #29577 ) ) ;
#20511 = LINE ( 'NONE', #24455, #36457 ) ;
#20512 = CARTESIAN_POINT ( 'NONE',  ( -92.16375985330357423, -175.3837268820161057, 117.1181148702521710 ) ) ;
#20513 = ORIENTED_EDGE ( 'NONE', *, *, #5803, .T. ) ;
#20514 = CARTESIAN_POINT ( 'NONE',  ( -332.3517673607765914, -65.92952926200918284, -16.90091414705545247 ) ) ;
#20515 = FACE_OUTER_BOUND ( 'NONE', #1122, .T. ) ;
#20517 = DIRECTION ( 'NONE',  ( -1.000000000000000000, 0.000000000000000000, 0.000000000000000000 ) ) ;
#20516 = DIRECTION ( 'NONE',  ( 0.000000000000000000, -4.093947403305264743E-14, 1.000000000000000000 ) ) ;
#20518 = EDGE_CURVE ( 'NONE', #47358, #37325, #11908, .T. ) ;
#20519 = ORIENTED_EDGE ( 'NONE', *, *, #28564, .F. ) ;
#20520 = LINE ( 'NONE', #12896, #50873 ) ;
#20521 = DIRECTION ( 'NONE',  ( 0.000000000000000000, -0.000000000000000000, -1.000000000000000000 ) ) ;
#20522 =( LENGTH_UNIT ( ) NAMED_UNIT ( * ) SI_UNIT ( .MILLI., .METRE. ) );
#20523 = EDGE_LOOP ( 'NONE', ( #6587, #38406, #7001, #11367 ) ) ;
#20524 = LINE ( 'NONE', #20802, #39947 ) ;
#20525 = VECTOR ( 'NONE', #50212, 1000.000000000000000 ) ;
#20526 = CARTESIAN_POINT ( 'NONE',  ( -49.29161362951453640, -175.3837268820161057, 0.5829794791144718991 ) ) ;
#20527 = AXIS2_PLACEMENT_3D ( 'NONE', #3936, #231, #19958 ) ;
#20528 = ORIENTED_EDGE ( 'NONE', *, *, #14910, .F. ) ;
#20529 = CARTESIAN_POINT ( 'NONE',  ( -47.50057025920934706, -183.6283474603465606, -0.2059786187410884151 ) ) ;
#20531 = CIRCLE ( 'NONE', #19702, 125.0000000000000000 ) ;
#20530 = CARTESIAN_POINT ( 'NONE',  ( -1.230335819511603423, -183.6283474603465606, 115.7261930397108216 ) ) ;
#20532 = ADVANCED_FACE ( 'NONE', ( #40022 ), #868, .F. ) ;
#20533 = ORIENTED_EDGE ( 'NONE', *, *, #46852, .T. ) ;
#20534 = CARTESIAN_POINT ( 'NONE',  ( -172.5669052183642123, -177.1207230881787780, 15.07392567185553567 ) ) ;
#20535 = VERTEX_POINT ( 'NONE', #24006 ) ;
#20536 = LINE ( 'NONE', #8201, #6362 ) ;
#20537 = CARTESIAN_POINT ( 'NONE',  ( 30.05499637021959813, -177.1207230881787780, -97.24912084693207248 ) ) ;
#20538 = AXIS2_PLACEMENT_3D ( 'NONE', #22321, #38352, #17377 ) ;
#20539 = EDGE_CURVE ( 'NONE', #37802, #41107, #20064, .T. ) ;
#20540 = DIRECTION ( 'NONE',  ( -1.000000000000000000, 0.000000000000000000, 0.000000000000000000 ) ) ;
#20541 = CARTESIAN_POINT ( 'NONE',  ( -166.9492939735806090, -189.7472609257535510, 39.87254040532606325 ) ) ;
#20542 = DIRECTION ( 'NONE',  ( 0.000000000000000000, 0.8854560256532157947, 0.4647231720437573488 ) ) ;
#20543 = EDGE_CURVE ( 'NONE', #18993, #41471, #16664, .T. ) ;
#20544 = CIRCLE ( 'NONE', #2915, 125.0000000000000000 ) ;
#20545 = ADVANCED_FACE ( 'NONE', ( #9028 ), #5087, .T. ) ;
#20546 = CARTESIAN_POINT ( 'NONE',  ( 69.14211578623219623, -177.1207230881787780, 42.31126686685117022 ) ) ;
#20547 = EDGE_CURVE ( 'NONE', #37656, #36987, #40802, .T. ) ;
#20548 = CARTESIAN_POINT ( 'NONE',  ( -48.47912675150885065, -189.7472609257535510, 6.938893903907228378E-15 ) ) ;
#20549 = LINE ( 'NONE', #47654, #19696 ) ;
#20551 = ORIENTED_EDGE ( 'NONE', *, *, #38155, .T. ) ;
#20550 = CARTESIAN_POINT ( 'NONE',  ( -339.1964088526558498, -108.8949048983204051, 57.16590939599314680 ) ) ;
#20552 = VERTEX_POINT ( 'NONE', #20855 ) ;
#20553 = DIRECTION ( 'NONE',  ( 0.000000000000000000, 0.8229838658936556861, -0.5680647467311569221 ) ) ;
#20554 = CARTESIAN_POINT ( 'NONE',  ( -140.8230258362169707, -193.5000000000000000, 84.24728067916045404 ) ) ;
#20555 = VERTEX_POINT ( 'NONE', #48713 ) ;
#20556 = ORIENTED_EDGE ( 'NONE', *, *, #27879, .T. ) ;
#20557 = VECTOR ( 'NONE', #50414, 1000.000000000000000 ) ;
#20558 = EDGE_CURVE ( 'NONE', #32896, #51992, #43977, .T. ) ;
#20559 = EDGE_LOOP ( 'NONE', ( #7588, #27735, #14505, #68 ) ) ;
#20560 = CARTESIAN_POINT ( 'NONE',  ( 75.27070168362158142, -193.5000000000000000, 17.63462396184792524 ) ) ;
#20561 = CIRCLE ( 'NONE', #22251, 125.0000000000000000 ) ;
#20562 = VECTOR ( 'NONE', #9820, 1000.000000000000000 ) ;
#20563 = EDGE_CURVE ( 'NONE', #28063, #21855, #87, .T. ) ;
#20564 = DIRECTION ( 'NONE',  ( -0.000000000000000000, 1.000000000000000000, 0.000000000000000000 ) ) ;
#20565 = DIRECTION ( 'NONE',  ( -1.000000000000000000, 0.000000000000000000, 0.000000000000000000 ) ) ;
#20566 = ORIENTED_EDGE ( 'NONE', *, *, #30592, .T. ) ;
#20567 = VERTEX_POINT ( 'NONE', #48192 ) ;
#20568 = AXIS2_PLACEMENT_3D ( 'NONE', #41762, #42258, #30192 ) ;
#20569 = EDGE_CURVE ( 'NONE', #41226, #4457, #48969, .T. ) ;
#20570 = PLANE ( 'NONE',  #9032 ) ;
#20571 = CARTESIAN_POINT ( 'NONE',  ( 55.03325008324586776, -177.1207230881787780, -70.07273251429357686 ) ) ;
#20573 = ORIENTED_EDGE ( 'NONE', *, *, #7628, .T. ) ;
#20572 = DIRECTION ( 'NONE',  ( -1.000000000000000000, 0.000000000000000000, 0.000000000000000000 ) ) ;
#20574 = AXIS2_PLACEMENT_3D ( 'NONE', #33324, #13355, #17048 ) ;
#20575 = PLANE ( 'NONE',  #38817 ) ;
#20576 = AXIS2_PLACEMENT_3D ( 'NONE', #51108, #15095, #15336 ) ;
#20577 = CARTESIAN_POINT ( 'NONE',  ( -330.4913330509368166, -182.5000000000000568, -0.4999999999999551470 ) ) ;
#20578 = EDGE_LOOP ( 'NONE', ( #30293, #12222, #48590, #23589 ) ) ;
#20579 = LINE ( 'NONE', #31890, #2032 ) ;
#20580 = EDGE_LOOP ( 'NONE', ( #35854, #21381, #19257, #44428 ) ) ;
#20581 = DIRECTION ( 'NONE',  ( -0.000000000000000000, 1.000000000000000000, -0.000000000000000000 ) ) ;
#20582 = AXIS2_PLACEMENT_3D ( 'NONE', #13160, #32854, #28908 ) ;
#20583 = FACE_OUTER_BOUND ( 'NONE', #30403, .T. ) ;
#20584 = DIRECTION ( 'NONE',  ( 1.000000000000000000, -0.000000000000000000, -0.000000000000000000 ) ) ;
#20585 = CIRCLE ( 'NONE', #25738, 4.000000000000003553 ) ;
#20586 = ORIENTED_EDGE ( 'NONE', *, *, #45124, .F. ) ;
#20587 = ORIENTED_EDGE ( 'NONE', *, *, #8664, .F. ) ;
#20588 = DIRECTION ( 'NONE',  ( 0.000000000000000000, 0.000000000000000000, 1.000000000000000000 ) ) ;
#20589 = FACE_OUTER_BOUND ( 'NONE', #34322, .T. ) ;
#20590 = ORIENTED_EDGE ( 'NONE', *, *, #19960, .T. ) ;
#20591 = DIRECTION ( 'NONE',  ( 0.000000000000000000, -0.000000000000000000, -1.000000000000000000 ) ) ;
#20592 = DIRECTION ( 'NONE',  ( -0.000000000000000000, -3.491481338843133355E-15, -1.000000000000000000 ) ) ;
#20593 = ORIENTED_EDGE ( 'NONE', *, *, #7976, .T. ) ;
#20594 = DIRECTION ( 'NONE',  ( 0.000000000000000000, 0.8229838658936613482, 0.5680647467311485954 ) ) ;
#20595 = LINE ( 'NONE', #32686, #34804 ) ;
#20596 = VERTEX_POINT ( 'NONE', #32672 ) ;
#20597 = CARTESIAN_POINT ( 'NONE',  ( -336.3521761649654422, -69.26746417191145611, -23.38292116578723068 ) ) ;
#20598 = EDGE_LOOP ( 'NONE', ( #28259, #40226, #40660, #6371 ) ) ;
#20599 = AXIS2_PLACEMENT_3D ( 'NONE', #298, #16619, #12641 ) ;
#20600 = CARTESIAN_POINT ( 'NONE',  ( -77.03256798524175508, -175.3837268820161057, 121.6951149130964893 ) ) ;
#20601 = ORIENTED_EDGE ( 'NONE', *, *, #10110, .F. ) ;
#20602 = AXIS2_PLACEMENT_3D ( 'NONE', #48199, #8244, #28460 ) ;
#20603 = VECTOR ( 'NONE', #33668, 1000.000000000000114 ) ;
#20604 = DIRECTION ( 'NONE',  ( 0.000000000000000000, -1.000000000000000000, -0.000000000000000000 ) ) ;
#20605 = CARTESIAN_POINT ( 'NONE',  ( -336.3521761649654422, -101.0520950768976149, 54.58714071513087873 ) ) ;
#20606 = CARTESIAN_POINT ( 'NONE',  ( -336.3521761649654422, -123.5000000000000284, 0.000000000000000000 ) ) ;
#20607 = ADVANCED_FACE ( 'NONE', ( #20314 ), #12164, .F. ) ;
#20608 = EDGE_CURVE ( 'NONE', #26111, #21667, #24272, .T. ) ;
#20609 = PLANE ( 'NONE',  #36659 ) ;
#20610 = ORIENTED_EDGE ( 'NONE', *, *, #29162, .T. ) ;
#20611 = CARTESIAN_POINT ( 'NONE',  ( 67.42090074966655777, -175.3837268820161057, -46.82076062204441058 ) ) ;
#20612 = ORIENTED_EDGE ( 'NONE', *, *, #51304, .T. ) ;
#20613 = APPLICATION_CONTEXT ( 'automotive_design' ) ;
#20614 = ORIENTED_EDGE ( 'NONE', *, *, #21085, .F. ) ;
#20615 = CIRCLE ( 'NONE', #9708, 125.0000000000000000 ) ;
#20616 = DIRECTION ( 'NONE',  ( -0.000000000000000000, 1.000000000000000000, -0.000000000000000000 ) ) ;
#20618 = ORIENTED_EDGE ( 'NONE', *, *, #29861, .T. ) ;
#20617 = CARTESIAN_POINT ( 'NONE',  ( -48.88225018079680950, -193.5000000000000000, -0.9151456172430169067 ) ) ;
#20619 = CIRCLE ( 'NONE', #41577, 125.0000000000000000 ) ;
#20620 = VERTEX_POINT ( 'NONE', #25061 ) ;
#20621 = DIRECTION ( 'NONE',  ( -0.8124868780056742068, 0.000000000000000000, -0.5829794791144820021 ) ) ;
#20622 = AXIS2_PLACEMENT_3D ( 'NONE', #19485, #31313, #40228 ) ;
#20623 = VECTOR ( 'NONE', #3515, 1000.000000000000227 ) ;
#20624 = CARTESIAN_POINT ( 'NONE',  ( -173.4460699164830260, -189.7472609257535510, -2.874563619423202265 ) ) ;
#20625 = ORIENTED_EDGE ( 'NONE', *, *, #48396, .F. ) ;
#20626 = CARTESIAN_POINT ( 'NONE',  ( -332.3517673607765914, -113.6616659693417546, 59.18789727217204444 ) ) ;
#20627 = ADVANCED_FACE ( 'NONE', ( #21101 ), #37123, .F. ) ;
#20628 = ORIENTED_EDGE ( 'NONE', *, *, #36626, .T. ) ;
#20629 = FACE_OUTER_BOUND ( 'NONE', #40839, .T. ) ;
#20630 = DIRECTION ( 'NONE',  ( 0.000000000000000000, -1.000000000000000000, 0.000000000000000000 ) ) ;
#20631 = DIRECTION ( 'NONE',  ( 0.000000000000000000, -0.000000000000000000, 1.000000000000000000 ) ) ;
#20632 = DIRECTION ( 'NONE',  ( 0.000000000000000000, -0.000000000000000000, -1.000000000000000000 ) ) ;
#20633 = ORIENTED_EDGE ( 'NONE', *, *, #17098, .T. ) ;
#20634 = ORIENTED_EDGE ( 'NONE', *, *, #20141, .F. ) ;
#20635 = EDGE_CURVE ( 'NONE', #32740, #16500, #44502, .T. ) ;
#20636 = EDGE_LOOP ( 'NONE', ( #29770, #33103, #36156, #25469 ) ) ;
#20637 = DIRECTION ( 'NONE',  ( 0.000000000000000000, 0.000000000000000000, -1.000000000000000000 ) ) ;
#20638 = LINE ( 'NONE', #32976, #35210 ) ;
#20639 = CIRCLE ( 'NONE', #50028, 125.0000000000000000 ) ;
#20640 = DIRECTION ( 'NONE',  ( 0.000000000000000000, -1.000000000000000000, 0.000000000000000000 ) ) ;
#20641 = VECTOR ( 'NONE', #32026, 1000.000000000000000 ) ;
#20642 = CYLINDRICAL_SURFACE ( 'NONE', #11096, 60.00000000000000000 ) ;
#20643 = PLANE ( 'NONE',  #5410 ) ;
#20644 = ORIENTED_EDGE ( 'NONE', *, *, #19424, .T. ) ;
#20645 = VECTOR ( 'NONE', #14275, 1000.000000000000000 ) ;
#20646 = EDGE_CURVE ( 'NONE', #32529, #32483, #40539, .T. ) ;
#20647 = VERTEX_POINT ( 'NONE', #614 ) ;
#20649 = ORIENTED_EDGE ( 'NONE', *, *, #20125, .T. ) ;
#20648 = DIRECTION ( 'NONE',  ( 0.8896570909947436601, 0.000000000000000000, 0.4566292373937200777 ) ) ;
#20650 = ORIENTED_EDGE ( 'NONE', *, *, #21491, .F. ) ;
#20651 = LINE ( 'NONE', #32743, #19925 ) ;
#20652 = AXIS2_PLACEMENT_3D ( 'NONE', #6190, #27635, #31053 ) ;
#20653 = DIRECTION ( 'NONE',  ( -0.000000000000000000, 1.000000000000000000, 0.000000000000000000 ) ) ;
#20654 = AXIS2_PLACEMENT_3D ( 'NONE', #41608, #29524, #21661 ) ;
#20655 = CARTESIAN_POINT ( 'NONE',  ( -336.3521761649654422, -93.75055682584159911, 51.01861988938794923 ) ) ;
#20656 = CARTESIAN_POINT ( 'NONE',  ( -160.0000000000000284, -123.5000000000000284, 41.63467731922665394 ) ) ;
#20657 = ORIENTED_EDGE ( 'NONE', *, *, #49497, .T. ) ;
#20658 = DIRECTION ( 'NONE',  ( 0.000000000000000000, 0.000000000000000000, 1.000000000000000000 ) ) ;
#20659 = CIRCLE ( 'NONE', #8924, 60.00000000000000000 ) ;
#20660 = ORIENTED_EDGE ( 'NONE', *, *, #8574, .T. ) ;
#20661 = ADVANCED_FACE ( 'NONE', ( #33466 ), #13227, .T. ) ;
#20662 = AXIS2_PLACEMENT_3D ( 'NONE', #6974, #51148, #14879 ) ;
#20663 = VERTEX_POINT ( 'NONE', #30283 ) ;
#20664 = DIRECTION ( 'NONE',  ( 1.000000000000000000, 0.000000000000000000, 0.000000000000000000 ) ) ;
#20665 = DIRECTION ( 'NONE',  ( -8.718379230999703429E-17, 0.4647231720437695057, 0.8854560256532093554 ) ) ;
#20666 = LINE ( 'NONE', #45824, #20562 ) ;
#20667 = CARTESIAN_POINT ( 'NONE',  ( 141.7825277784304205, -213.5000000000000000, -41.45482488023466061 ) ) ;
#20668 = DIRECTION ( 'NONE',  ( -0.000000000000000000, -1.000000000000000000, -0.000000000000000000 ) ) ;
#20669 = LINE ( 'NONE', #171, #28715 ) ;
#20670 = EDGE_CURVE ( 'NONE', #4146, #153, #21637, .T. ) ;
#20671 = ADVANCED_FACE ( 'NONE', ( #45301 ), #5873, .F. ) ;
#20672 = EDGE_LOOP ( 'NONE', ( #42544, #28032, #24839, #10548 ) ) ;
#20673 = LINE ( 'NONE', #37220, #34741 ) ;
#20674 = CARTESIAN_POINT ( 'NONE',  ( -260.0000000000000000, -63.50000000000000000, 60.00000000000000711 ) ) ;
#20675 = PLANE ( 'NONE',  #48796 ) ;
#20676 = FACE_BOUND ( 'NONE', #18525, .T. ) ;
#20677 = VERTEX_POINT ( 'NONE', #5611 ) ;
#20678 = EDGE_CURVE ( 'NONE', #14148, #10828, #34161, .T. ) ;
#20679 = CIRCLE ( 'NONE', #49200, 125.0000000000000000 ) ;
#20680 = AXIS2_PLACEMENT_3D ( 'NONE', #15709, #31725, #23830 ) ;
#20681 = CARTESIAN_POINT ( 'NONE',  ( -47.53180039765465636, -175.3837268820161057, -0.3202698538628280800 ) ) ;
#20682 = ORIENTED_EDGE ( 'NONE', *, *, #40585, .T. ) ;
#20683 = AXIS2_PLACEMENT_3D ( 'NONE', #25264, #8975, #33913 ) ;
#20684 = CARTESIAN_POINT ( 'NONE',  ( -330.4913330509368166, -157.9941932480469973, -49.09328500076553325 ) ) ;
#20685 = ORIENTED_EDGE ( 'NONE', *, *, #1920, .T. ) ;
#20686 = DIRECTION ( 'NONE',  ( 0.3202698538628279690, 0.000000000000000000, 0.9473263538541946138 ) ) ;
#20687 = ORIENTED_EDGE ( 'NONE', *, *, #34716, .F. ) ;
#20688 = DIRECTION ( 'NONE',  ( 0.000000000000000000, 0.000000000000000000, 1.000000000000000000 ) ) ;
#20689 = CIRCLE ( 'NONE', #30733, 125.0000000000000000 ) ;
#20690 = FACE_BOUND ( 'NONE', #20481, .T. ) ;
#20691 = VECTOR ( 'NONE', #9493, 1000.000000000000114 ) ;
#20693 = VERTEX_POINT ( 'NONE', #26337 ) ;
#20692 = CARTESIAN_POINT ( 'NONE',  ( -49.30901192927175458, -189.7472609257535510, -124.9972451320097093 ) ) ;
#20694 = EDGE_CURVE ( 'NONE', #35744, #21107, #48425, .T. ) ;
#20695 = CONICAL_SURFACE ( 'NONE', #3059, 14.00000000000001066, 0.7853981633974491672 ) ;
#20696 = AXIS2_PLACEMENT_3D ( 'NONE', #32425, #37404, #28729 ) ;
#20697 = AXIS2_PLACEMENT_3D ( 'NONE', #11441, #7260, #8030 ) ;
#20698 = DIRECTION ( 'NONE',  ( 0.000000000000000000, 1.000000000000000000, 0.000000000000000000 ) ) ;
#20699 = ORIENTED_EDGE ( 'NONE', *, *, #43908, .F. ) ;
#20700 = EDGE_LOOP ( 'NONE', ( #17347, #40717, #26088, #15082 ) ) ;
#20701 = VECTOR ( 'NONE', #25559, 1000.000000000000114 ) ;
#20702 = CARTESIAN_POINT ( 'NONE',  ( -84.19171550243319757, -193.5000000000000000, 119.7898618611247628 ) ) ;
#20703 = DIRECTION ( 'NONE',  ( -0.000000000000000000, 0.4739294676984008858, 0.8805628084623552398 ) ) ;
#20704 = ORIENTED_EDGE ( 'NONE', *, *, #15359, .T. ) ;
#20705 = CARTESIAN_POINT ( 'NONE',  ( -47.66663987350317910, -193.5000000000000000, 0.5829794791144832233 ) ) ;
#20706 = DIRECTION ( 'NONE',  ( 0.000000000000000000, 0.000000000000000000, 1.000000000000000000 ) ) ;
#20707 = DIRECTION ( 'NONE',  ( 0.4566292373937077542, 0.000000000000000000, 0.8896570909947499883 ) ) ;
#20708 = CARTESIAN_POINT ( 'NONE',  ( -92.78132261338707565, -175.3837268820161057, -116.8859077982276773 ) ) ;
#20709 = DIRECTION ( 'NONE',  ( 0.1182731709213592358, 0.000000000000000000, 0.9929810960135178055 ) ) ;
#20710 = ORIENTED_EDGE ( 'NONE', *, *, #33779, .F. ) ;
#20713 = VERTEX_POINT ( 'NONE', #45548 ) ;
#20712 = DIRECTION ( 'NONE',  ( 1.043714542225393223E-14, 0.9350162426854181641, 0.3546048870425267951 ) ) ;
#20711 = LINE ( 'NONE', #36747, #33227 ) ;
#20714 = VECTOR ( 'NONE', #892, 1000.000000000000114 ) ;
#20715 = EDGE_LOOP ( 'NONE', ( #23135, #45406, #5841, #19529 ) ) ;
#20716 = VECTOR ( 'NONE', #19004, 1000.000000000000000 ) ;
#20717 = PLANE ( 'NONE',  #35735 ) ;
#20718 = ORIENTED_EDGE ( 'NONE', *, *, #23285, .F. ) ;
#20719 = CARTESIAN_POINT ( 'NONE',  ( -336.3521761649654422, -86.34605966037949543, -45.90766452162698386 ) ) ;
#20720 = ORIENTED_EDGE ( 'NONE', *, *, #49954, .T. ) ;
#20721 = VECTOR ( 'NONE', #47747, 1000.000000000000000 ) ;
#20722 = ADVANCED_FACE ( 'NONE', ( #1391 ), #37386, .F. ) ;
#20723 = CARTESIAN_POINT ( 'NONE',  ( -146.2338470511239450, -177.1207230881787780, 76.29032973288700248 ) ) ;
#20724 = CARTESIAN_POINT ( 'NONE',  ( -165.5546359831674295, -193.5000000000000000, 43.79868877201493405 ) ) ;
#20725 = VERTEX_POINT ( 'NONE', #42105 ) ;
#20727 = DIRECTION ( 'NONE',  ( 0.000000000000000000, 0.000000000000000000, 1.000000000000000000 ) ) ;
#20726 = LINE ( 'NONE', #36759, #636 ) ;
#20728 = VERTEX_POINT ( 'NONE', #33185 ) ;
#20729 = EDGE_LOOP ( 'NONE', ( #38869, #1982, #13486, #685 ) ) ;
#20730 = CARTESIAN_POINT ( 'NONE',  ( -48.47912675150885065, -189.7472609257535510, 6.938893903907228378E-15 ) ) ;
#20731 = VECTOR ( 'NONE', #39560, 1000.000000000000000 ) ;
#20732 = PLANE ( 'NONE',  #18960 ) ;
#20733 = AXIS2_PLACEMENT_3D ( 'NONE', #20213, #484, #48071 ) ;
#20734 = DIRECTION ( 'NONE',  ( 0.000000000000000000, 0.000000000000000000, 1.000000000000000000 ) ) ;
#20735 = CARTESIAN_POINT ( 'NONE',  ( -330.4913330509368166, -68.15673923803930734, -20.45418021416698551 ) ) ;
#20736 = ORIENTED_EDGE ( 'NONE', *, *, #313, .F. ) ;
#20737 = CIRCLE ( 'NONE', #33347, 125.0000000000000000 ) ;
#20738 = VECTOR ( 'NONE', #8198, 1000.000000000000114 ) ;
#20739 = FACE_OUTER_BOUND ( 'NONE', #12440, .T. ) ;
#20740 = DIRECTION ( 'NONE',  ( 0.000000000000000000, -1.000000000000000000, 0.000000000000000000 ) ) ;
#20741 = ADVANCED_FACE ( 'NONE', ( #13482 ), #25307, .T. ) ;
#20742 = VECTOR ( 'NONE', #37375, 1000.000000000000000 ) ;
#20743 = DIRECTION ( 'NONE',  ( 0.000000000000000000, 0.000000000000000000, 1.000000000000000000 ) ) ;
#20744 = DIRECTION ( 'NONE',  ( -1.000000000000000000, 0.000000000000000000, 0.000000000000000000 ) ) ;
#20745 = EDGE_CURVE ( 'NONE', #27746, #28072, #30029, .T. ) ;
#20746 = AXIS2_PLACEMENT_3D ( 'NONE', #23379, #19948, #19676 ) ;
#20747 = CARTESIAN_POINT ( 'NONE',  ( -48.47912675150885065, -175.3837268820161057, 6.938893903907228378E-15 ) ) ;
#20748 = ORIENTED_EDGE ( 'NONE', *, *, #30958, .F. ) ;
#20749 = ORIENTED_EDGE ( 'NONE', *, *, #35944, .F. ) ;
#20750 = EDGE_CURVE ( 'NONE', #8060, #36650, #41582, .T. ) ;
#20751 = DIRECTION ( 'NONE',  ( -0.2348860457809842095, 0.000000000000000000, 0.9720229140804107493 ) ) ;
#20752 = DIRECTION ( 'NONE',  ( 0.7378332790417285736, 0.000000000000000000, -0.6749830015182091136 ) ) ;
#20753 = DIRECTION ( 'NONE',  ( -1.000000000000000000, -0.000000000000000000, -0.000000000000000000 ) ) ;
#20754 = ORIENTED_EDGE ( 'NONE', *, *, #32711, .F. ) ;
#20755 = ORIENTED_EDGE ( 'NONE', *, *, #18783, .T. ) ;
#20756 = ORIENTED_EDGE ( 'NONE', *, *, #38752, .T. ) ;
#20757 = VECTOR ( 'NONE', #8429, 1000.000000000000000 ) ;
#20758 = DIRECTION ( 'NONE',  ( -8.718379230999704661E-17, 0.1205366802553164696, -0.9927088740980548609 ) ) ;
#20759 = CIRCLE ( 'NONE', #21597, 125.0000000000000000 ) ;
#20760 = DIRECTION ( 'NONE',  ( 0.000000000000000000, -0.9350162426854121689, 0.3546048870425426713 ) ) ;
#20761 = DIRECTION ( 'NONE',  ( 0.000000000000000000, 0.000000000000000000, -1.000000000000000000 ) ) ;
#20762 = DIRECTION ( 'NONE',  ( 0.000000000000000000, -1.000000000000000000, 0.000000000000000000 ) ) ;
#20763 = VECTOR ( 'NONE', #38595, 1000.000000000000000 ) ;
#20764 = ORIENTED_EDGE ( 'NONE', *, *, #25967, .F. ) ;
#20765 = CARTESIAN_POINT ( 'NONE',  ( -332.3517673607765914, -82.40546666720629787, 42.41660376256258047 ) ) ;
#20766 = CARTESIAN_POINT ( 'NONE',  ( -336.3521761649654422, -76.43926241122620979, -35.68215131113738181 ) ) ;
#20767 = ORIENTED_EDGE ( 'NONE', *, *, #6019, .T. ) ;
#20768 = CARTESIAN_POINT ( 'NONE',  ( -43.48323084606168720, -177.1207230881787780, 123.9001241957026167 ) ) ;
#20769 = VERTEX_POINT ( 'NONE', #29248 ) ;
#20770 = AXIS2_PLACEMENT_3D ( 'NONE', #2009, #6746, #18049 ) ;
#20771 = AXIS2_PLACEMENT_3D ( 'NONE', #16125, #334, #32395 ) ;
#20772 = ORIENTED_EDGE ( 'NONE', *, *, #22111, .F. ) ;
#20773 = DIRECTION ( 'NONE',  ( -0.1768902751225733261, 0.000000000000000000, 0.9842305779475966077 ) ) ;
#20774 = AXIS2_PLACEMENT_3D ( 'NONE', #45951, #34101, #5748 ) ;
#20775 = VECTOR ( 'NONE', #26329, 999.9999999999998863 ) ;
#20776 = CARTESIAN_POINT ( 'NONE',  ( 14.94072793302542124, -175.3837268820161057, 107.7168604805791716 ) ) ;
#20777 = CARTESIAN_POINT ( 'NONE',  ( -336.3521761649654422, -132.2320517616439020, -58.37307289257706344 ) ) ;
#20780 = EDGE_LOOP ( 'NONE', ( #7536, #40978, #19875, #33866 ) ) ;
#20779 = CARTESIAN_POINT ( 'NONE',  ( -332.3517673607765914, -64.50000000000000000, -2.632288850093980503 ) ) ;
#20778 = FACE_OUTER_BOUND ( 'NONE', #49087, .T. ) ;
#20781 = PLANE ( 'NONE',  #50798 ) ;
#20782 = VERTEX_POINT ( 'NONE', #5348 ) ;
#20783 = DIRECTION ( 'NONE',  ( 0.6965510290629882695, 0.000000000000000000, 0.7175072570443395970 ) ) ;
#20784 = FACE_OUTER_BOUND ( 'NONE', #10018, .T. ) ;
#20785 = ORIENTED_EDGE ( 'NONE', *, *, #31266, .F. ) ;
#20786 = EDGE_CURVE ( 'NONE', #19679, #40406, #17699, .T. ) ;
#20787 = EDGE_CURVE ( 'NONE', #26369, #7333, #17949, .T. ) ;
#20788 = EDGE_CURVE ( 'NONE', #31046, #22971, #7310, .T. ) ;
#20789 = DIRECTION ( 'NONE',  ( 0.000000000000000000, -1.000000000000000000, 0.000000000000000000 ) ) ;
#20791 = DIRECTION ( 'NONE',  ( 0.000000000000000000, -0.000000000000000000, -1.000000000000000000 ) ) ;
#20790 = DIRECTION ( 'NONE',  ( 0.2059786187410889424, 0.000000000000000000, 0.9785564922995060311 ) ) ;
#20792 = VERTEX_POINT ( 'NONE', #45805 ) ;
#20793 = ADVANCED_FACE ( 'NONE', ( #38430 ), #21363, .T. ) ;
#20794 = DIRECTION ( 'NONE',  ( 0.000000000000000000, -1.000000000000000000, 0.000000000000000000 ) ) ;
#20795 = VECTOR ( 'NONE', #39517, 1000.000000000000114 ) ;
#20796 = DIRECTION ( 'NONE',  ( 0.000000000000000000, 1.000000000000000000, 0.000000000000000000 ) ) ;
#20797 = VECTOR ( 'NONE', #39131, 1000.000000000000000 ) ;
#20798 = DIRECTION ( 'NONE',  ( 0.1182731709213660498, 0.000000000000000000, -0.9929810960135169173 ) ) ;
#20799 = ORIENTED_EDGE ( 'NONE', *, *, #19894, .F. ) ;
#20800 = EDGE_CURVE ( 'NONE', #33685, #1866, #41858, .T. ) ;
#20801 = CARTESIAN_POINT ( 'NONE',  ( -86.93810158023210022, -183.6283474603465606, 117.8859915627477335 ) ) ;
#20802 = CARTESIAN_POINT ( 'NONE',  ( 32.99469856375239374, -189.7472609257535510, 94.79987230212019256 ) ) ;
#20803 = EDGE_CURVE ( 'NONE', #41684, #37940, #26077, .T. ) ;
#20804 = AXIS2_PLACEMENT_3D ( 'NONE', #23485, #47915, #40261 ) ;
#20805 = CYLINDRICAL_SURFACE ( 'NONE', #43342, 125.0000000000000000 ) ;
#20806 = VERTEX_POINT ( 'NONE', #30799 ) ;
#20807 = EDGE_CURVE ( 'NONE', #39429, #44939, #34999, .T. ) ;
#20808 = CARTESIAN_POINT ( 'NONE',  ( 75.60865171534661044, -183.6283474603465606, -15.07392567185467236 ) ) ;
#20809 = EDGE_CURVE ( 'NONE', #36354, #42318, #11604, .T. ) ;
#20810 = CARTESIAN_POINT ( 'NONE',  ( -110.8210171970983566, -175.3837268820161057, 107.1890582354659074 ) ) ;
#20811 = ORIENTED_EDGE ( 'NONE', *, *, #26882, .T. ) ;
#20812 = VECTOR ( 'NONE', #10102, 1000.000000000000000 ) ;
#20813 = ADVANCED_FACE ( 'NONE', ( #7420 ), #3449, .T. ) ;
#20814 = DIRECTION ( 'NONE',  ( 0.000000000000000000, 1.137978600240785454E-13, -1.000000000000000000 ) ) ;
#20815 = CARTESIAN_POINT ( 'NONE',  ( 75.02564229359539638, -193.5000000000000000, -19.27620354518634826 ) ) ;
#20816 = EDGE_CURVE ( 'NONE', #20956, #13540, #14865, .T. ) ;
#20817 = PLANE ( 'NONE',  #51248 ) ;
#20818 = DIRECTION ( 'NONE',  ( 0.000000000000000000, -0.000000000000000000, -1.000000000000000000 ) ) ;
#20819 = CARTESIAN_POINT ( 'NONE',  ( -48.65601702663143868, -183.6283474603465606, 0.9842305779476024918 ) ) ;
#20821 = AXIS2_PLACEMENT_3D ( 'NONE', #40729, #24989, #17631 ) ;
#20820 = LINE ( 'NONE', #21070, #48096 ) ;
#20822 = DIRECTION ( 'NONE',  ( -1.000000000000000000, -0.000000000000000000, 0.000000000000000000 ) ) ;
#20823 = LINE ( 'NONE', #36848, #45508 ) ;
#20825 = ORIENTED_EDGE ( 'NONE', *, *, #29783, .F. ) ;
#20824 = FACE_OUTER_BOUND ( 'NONE', #5629, .T. ) ;
#20826 = ORIENTED_EDGE ( 'NONE', *, *, #17395, .T. ) ;
#20827 = DIRECTION ( 'NONE',  ( 0.000000000000000000, 0.000000000000000000, -1.000000000000000000 ) ) ;
#20828 = EDGE_CURVE ( 'NONE', #2008, #32067, #3209, .T. ) ;
#20829 = LINE ( 'NONE', #41301, #17105 ) ;
#20830 = ORIENTED_EDGE ( 'NONE', *, *, #45143, .T. ) ;
#20831 = VECTOR ( 'NONE', #16327, 1000.000000000000000 ) ;
#20832 = VECTOR ( 'NONE', #3339, 1000.000000000000227 ) ;
#20833 = ORIENTED_EDGE ( 'NONE', *, *, #14398, .T. ) ;
#20834 = AXIS2_PLACEMENT_3D ( 'NONE', #14255, #35238, #11062 ) ;
#20835 = ORIENTED_EDGE ( 'NONE', *, *, #39177, .F. ) ;
#20836 = DIRECTION ( 'NONE',  ( 0.000000000000000000, 1.000000000000000000, 0.000000000000000000 ) ) ;
#20837 = AXIS2_PLACEMENT_3D ( 'NONE', #48368, #3965, #19989 ) ;
#20838 = DIRECTION ( 'NONE',  ( -0.9266896074318291543, 0.000000000000000000, -0.3758275821142488260 ) ) ;
#20839 = CARTESIAN_POINT ( 'NONE',  ( -33.64434644548591535, -175.3837268820161057, -123.1094209424468033 ) ) ;
#20840 = VERTEX_POINT ( 'NONE', #34731 ) ;
#20841 = ORIENTED_EDGE ( 'NONE', *, *, #47800, .T. ) ;
#20842 = EDGE_CURVE ( 'NONE', #42630, #13937, #44214, .T. ) ;
#20843 = DIRECTION ( 'NONE',  ( -0.000000000000000000, 0.2393156642875685636, 0.9709418174260492362 ) ) ;
#20844 = AXIS2_PLACEMENT_3D ( 'NONE', #15599, #7461, #39249 ) ;
#20846 = ORIENTED_EDGE ( 'NONE', *, *, #12497, .F. ) ;
#20845 = FACE_OUTER_BOUND ( 'NONE', #14108, .T. ) ;
#20847 = DIRECTION ( 'NONE',  ( -0.000000000000000000, 1.000000000000000000, 0.000000000000000000 ) ) ;
#20848 = ORIENTED_EDGE ( 'NONE', *, *, #38818, .T. ) ;
#20849 = DIRECTION ( 'NONE',  ( -0.7378332790417189146, 0.000000000000000000, -0.6749830015182196608 ) ) ;
#20850 = VERTEX_POINT ( 'NONE', #42631 ) ;
#20851 = ADVANCED_FACE ( 'NONE', ( #51550 ), #10567, .F. ) ;
#20852 = EDGE_CURVE ( 'NONE', #37982, #24439, #11073, .T. ) ;
#20853 = EDGE_CURVE ( 'NONE', #14387, #45870, #50783, .T. ) ;
#20854 = ADVANCED_FACE ( 'NONE', ( #51057 ), #11327, .F. ) ;
#20855 = CARTESIAN_POINT ( 'NONE',  ( 66.49421114223471818, -175.3837268820161057, -46.44493303993017719 ) ) ;
#20856 = DIRECTION ( 'NONE',  ( -0.000000000000000000, 1.000000000000000000, -0.000000000000000000 ) ) ;
#20857 = CARTESIAN_POINT ( 'NONE',  ( -305.0000000000000568, -94.18160986457394301, 52.34913561719000086 ) ) ;
#20858 = EDGE_CURVE ( 'NONE', #32415, #32067, #27364, .T. ) ;
#20859 = VECTOR ( 'NONE', #37845, 1000.000000000000000 ) ;
#20860 = ORIENTED_EDGE ( 'NONE', *, *, #41249, .F. ) ;
#20861 = ORIENTED_EDGE ( 'NONE', *, *, #12487, .T. ) ;
#20862 = DIRECTION ( 'NONE',  ( -0.000000000000000000, 1.000000000000000000, 0.000000000000000000 ) ) ;
#20863 = LINE ( 'NONE', #16917, #19111 ) ;
#20864 = ORIENTED_EDGE ( 'NONE', *, *, #29619, .F. ) ;
#20865 = EDGE_CURVE ( 'NONE', #28928, #10952, #29958, .T. ) ;
#20866 = EDGE_CURVE ( 'NONE', #664, #35703, #31049, .T. ) ;
#20867 = PLANE ( 'NONE',  #34127 ) ;
#20868 = LINE ( 'NONE', #32928, #39619 ) ;
#20869 = ORIENTED_EDGE ( 'NONE', *, *, #8092, .T. ) ;
#20870 = DIRECTION ( 'NONE',  ( 0.03686245026030392918, 0.000000000000000000, -0.9993203489176064602 ) ) ;
#20871 = ADVANCED_FACE ( 'NONE', ( #7144 ), #22664, .F. ) ;
#20872 = CARTESIAN_POINT ( 'NONE',  ( -149.9407190013151592, -189.7472609257535510, -73.01058346660460074 ) ) ;
#20873 = EDGE_CURVE ( 'NONE', #24589, #51222, #35250, .T. ) ;
#20874 = ORIENTED_EDGE ( 'NONE', *, *, #22775, .T. ) ;
#20875 = CARTESIAN_POINT ( 'NONE',  ( -84.85683048652070681, -175.3837268820161057, 118.5439281552633446 ) ) ;
#20876 = VERTEX_POINT ( 'NONE', #23441 ) ;
#20877 = FACE_BOUND ( 'NONE', #6953, .T. ) ;
#20878 = DIRECTION ( 'NONE',  ( 0.000000000000000000, 1.000000000000000000, 0.000000000000000000 ) ) ;
#20879 = VECTOR ( 'NONE', #6197, 1000.000000000000000 ) ;
#20880 = EDGE_CURVE ( 'NONE', #15236, #4741, #13201, .T. ) ;
#20881 = CIRCLE ( 'NONE', #16687, 125.0000000000000000 ) ;
#20882 = CARTESIAN_POINT ( 'NONE',  ( -47.74129347246712740, -177.1207230881787780, -0.6749830015182022303 ) ) ;
#20883 = ORIENTED_EDGE ( 'NONE', *, *, #25001, .T. ) ;
#20884 = AXIS2_PLACEMENT_3D ( 'NONE', #2855, #26004, #18888 ) ;
#20885 = ADVANCED_FACE ( 'NONE', ( #50527 ), #30533, .F. ) ;
#20886 = CARTESIAN_POINT ( 'NONE',  ( -48.65601702663143868, -177.1207230881787780, 0.9842305779476024918 ) ) ;
#20887 = DIRECTION ( 'NONE',  ( -0.000000000000000000, 0.000000000000000000, -1.000000000000000000 ) ) ;
#20888 = CARTESIAN_POINT ( 'NONE',  ( -180.0000000000000568, -115.7896721143442278, 60.00000000000000711 ) ) ;
#20889 = DIRECTION ( 'NONE',  ( 0.2920567706369764371, 0.000000000000000000, -0.9564009842765223146 ) ) ;
#20890 = ADVANCED_FACE ( 'NONE', ( #7904 ), #18231, .T. ) ;
#20891 = ORIENTED_EDGE ( 'NONE', *, *, #48741, .T. ) ;
#20892 = LINE ( 'NONE', #16425, #42961 ) ;
#20893 = EDGE_LOOP ( 'NONE', ( #43238, #21173, #29441, #40801 ) ) ;
#20894 = VERTEX_POINT ( 'NONE', #19733 ) ;
#20895 = VECTOR ( 'NONE', #1506, 1000.000000000000114 ) ;
#20896 = CARTESIAN_POINT ( 'NONE',  ( -40.24578378811990831, -175.3837268820161057, 124.7285535218268251 ) ) ;
#20898 = VERTEX_POINT ( 'NONE', #39956 ) ;
#20897 = LINE ( 'NONE', #44537, #51328 ) ;
#20899 = ORIENTED_EDGE ( 'NONE', *, *, #34716, .T. ) ;
#20900 = CARTESIAN_POINT ( 'NONE',  ( -169.2746641285359317, -175.3837268820161057, -32.14713283941908628 ) ) ;
#20901 = VECTOR ( 'NONE', #46208, 1000.000000000000000 ) ;
#20902 = ADVANCED_FACE ( 'NONE', ( #39690 ), #48658, .F. ) ;
#20903 = LINE ( 'NONE', #17212, #14272 ) ;
#20904 = EDGE_LOOP ( 'NONE', ( #44251, #46713, #29700, #50699 ) ) ;
#20905 = CARTESIAN_POINT ( 'NONE',  ( 5.542374969221976144, -177.1207230881787780, 112.7238987608088365 ) ) ;
#20906 = VERTEX_POINT ( 'NONE', #23939 ) ;
#20907 = CARTESIAN_POINT ( 'NONE',  ( -336.3521761649654422, -64.50000000000000000, -2.632288850093980503 ) ) ;
#20908 = LINE ( 'NONE', #35887, #51835 ) ;
#20909 = CARTESIAN_POINT ( 'NONE',  ( 8.448131207122532516, -175.3837268820161057, 111.2847127925100352 ) ) ;
#20910 = FACE_OUTER_BOUND ( 'NONE', #46021, .T. ) ;
#20911 = ORIENTED_EDGE ( 'NONE', *, *, #26485, .T. ) ;
#20912 = ORIENTED_EDGE ( 'NONE', *, *, #38113, .F. ) ;
#20913 = VERTEX_POINT ( 'NONE', #31835 ) ;
#20914 = DIRECTION ( 'NONE',  ( -0.000000000000000000, 1.000000000000000000, 0.000000000000000000 ) ) ;
#20915 = DIRECTION ( 'NONE',  ( 0.2920567706369694982, 0.000000000000000000, 0.9564009842765243130 ) ) ;
#20916 = AXIS2_PLACEMENT_3D ( 'NONE', #46487, #41771, #18110 ) ;
#20917 = CARTESIAN_POINT ( 'NONE',  ( -2.429962845726266397E-15, 20.00000000000000355, 0.000000000000000000 ) ) ;
#20918 = LINE ( 'NONE', #32978, #14458 ) ;
#20919 = DIRECTION ( 'NONE',  ( -8.718379230999707126E-17, -0.3546048870425426158, -0.9350162426854121689 ) ) ;
#20920 = ORIENTED_EDGE ( 'NONE', *, *, #8992, .F. ) ;
#20921 = AXIS2_PLACEMENT_3D ( 'NONE', #11719, #11449, #51680 ) ;
#20922 = EDGE_CURVE ( 'NONE', #22789, #7887, #20737, .T. ) ;
#20923 = ADVANCED_FACE ( 'NONE', ( #8693 ), #36540, .T. ) ;
#20924 = ORIENTED_EDGE ( 'NONE', *, *, #19831, .T. ) ;
#20926 = VERTEX_POINT ( 'NONE', #33583 ) ;
#20925 = DIRECTION ( 'NONE',  ( 0.000000000000000000, 0.2393156642875582940, 0.9709418174260519008 ) ) ;
#20927 = AXIS2_PLACEMENT_3D ( 'NONE', #34070, #38262, #45920 ) ;
#20928 = ORIENTED_EDGE ( 'NONE', *, *, #6478, .F. ) ;
#20929 = DIRECTION ( 'NONE',  ( 0.000000000000000000, -1.000000000000000000, 0.000000000000000000 ) ) ;
#20930 = CARTESIAN_POINT ( 'NONE',  ( -305.0000000000000568, -157.1712093821534211, -49.66134974749665076 ) ) ;
#20931 = PLANE ( 'NONE',  #36380 ) ;
#20932 = DIRECTION ( 'NONE',  ( -0.000000000000000000, 1.000000000000000000, -0.000000000000000000 ) ) ;
#20933 = ORIENTED_EDGE ( 'NONE', *, *, #30054, .T. ) ;
#20934 = DIRECTION ( 'NONE',  ( 0.000000000000000000, 1.000000000000000000, 0.000000000000000000 ) ) ;
#20935 = ORIENTED_EDGE ( 'NONE', *, *, #31586, .F. ) ;
#20936 = AXIS2_PLACEMENT_3D ( 'NONE', #13692, #39770, #41275 ) ;
#20937 = ORIENTED_EDGE ( 'NONE', *, *, #23345, .F. ) ;
#20938 = DIRECTION ( 'NONE',  ( 0.000000000000000000, 0.000000000000000000, -1.000000000000000000 ) ) ;
#20939 = EDGE_CURVE ( 'NONE', #20353, #13271, #51807, .T. ) ;
#20940 = LINE ( 'NONE', #5427, #22797 ) ;
#20941 = FACE_OUTER_BOUND ( 'NONE', #1612, .T. ) ;
#20942 = DIRECTION ( 'NONE',  ( 0.000000000000000000, -1.000000000000000000, -0.000000000000000000 ) ) ;
#20943 = PLANE ( 'NONE',  #44722 ) ;
#20944 = ORIENTED_EDGE ( 'NONE', *, *, #30841, .T. ) ;
#20945 = LINE ( 'NONE', #13040, #12072 ) ;
#20946 = FACE_OUTER_BOUND ( 'NONE', #17619, .T. ) ;
#20947 = EDGE_CURVE ( 'NONE', #18306, #38201, #44702, .T. ) ;
#20948 = DIRECTION ( 'NONE',  ( -1.000000000000000000, 0.000000000000000000, -0.000000000000000000 ) ) ;
#20949 = FACE_BOUND ( 'NONE', #9955, .T. ) ;
#20950 = EDGE_LOOP ( 'NONE', ( #7611, #35482, #50743, #15452 ) ) ;
#20951 = VECTOR ( 'NONE', #30627, 1000.000000000000000 ) ;
#20952 = CARTESIAN_POINT ( 'NONE',  ( -63.09433862318517328, -175.3837268820161057, -124.1426420773539405 ) ) ;
#20953 = EDGE_LOOP ( 'NONE', ( #51803, #7350, #50953, #6039 ) ) ;
#20954 = VECTOR ( 'NONE', #49432, 1000.000000000000000 ) ;
#20955 = LINE ( 'NONE', #16228, #40367 ) ;
#20956 = VERTEX_POINT ( 'NONE', #12096 ) ;
#20957 = PLANE ( 'NONE',  #45604 ) ;
#20958 = ORIENTED_EDGE ( 'NONE', *, *, #36892, .F. ) ;
#20959 = PRODUCT ( 'Flanges', 'Flanges', '', ( #20467 ) ) ;
#20960 = DIRECTION ( 'NONE',  ( 0.000000000000000000, 1.000000000000000000, -0.000000000000000000 ) ) ;
#20961 = DIRECTION ( 'NONE',  ( 1.000000000000000000, 0.000000000000000000, -0.000000000000000000 ) ) ;
#20963 = ORIENTED_EDGE ( 'NONE', *, *, #34609, .F. ) ;
#20962 = CARTESIAN_POINT ( 'NONE',  ( -330.4913330509368166, -66.33409060400670398, -14.60509510167892522 ) ) ;
#20964 = DIRECTION ( 'NONE',  ( -0.000000000000000000, 0.6631226582407937498, -0.7485107481711024136 ) ) ;
#20965 = ORIENTED_EDGE ( 'NONE', *, *, #13147, .T. ) ;
#20966 = ORIENTED_EDGE ( 'NONE', *, *, #38706, .T. ) ;
#20967 = CIRCLE ( 'NONE', #17644, 125.0000000000000000 ) ;
#20968 = ORIENTED_EDGE ( 'NONE', *, *, #40786, .T. ) ;
#20969 = CARTESIAN_POINT ( 'NONE',  ( -339.1964088526558498, -63.99980407363865709, -7.728304129924767452 ) ) ;
#20970 = CARTESIAN_POINT ( 'NONE',  ( -172.3334410065085649, -193.5000000000000000, -6.025661128238022357 ) ) ;
#20971 = VERTEX_POINT ( 'NONE', #16072 ) ;
#20972 = DIRECTION ( 'NONE',  ( -0.7378332790417189146, 0.000000000000000000, -0.6749830015182196608 ) ) ;
#20973 = CARTESIAN_POINT ( 'NONE',  ( 30.50828161901820224, -177.1207230881787780, 96.88131563365348597 ) ) ;
#20974 = CARTESIAN_POINT ( 'NONE',  ( -106.2948367055610106, -189.7472609257535510, -110.8257356506552185 ) ) ;
#20975 = ADVANCED_FACE ( 'NONE', ( #4500 ), #540, .T. ) ;
#20976 = DIRECTION ( 'NONE',  ( 0.7765238627180437447, 0.000000000000000000, -0.6300878435817094392 ) ) ;
#20977 = CARTESIAN_POINT ( 'NONE',  ( 55.35935253854128035, -183.6283474603465606, 69.58857822035041352 ) ) ;
#20978 = ORIENTED_EDGE ( 'NONE', *, *, #10032, .T. ) ;
#20981 = ORIENTED_EDGE ( 'NONE', *, *, #38282, .F. ) ;
#20980 = LINE ( 'NONE', #15755, #49926 ) ;
#20979 = DIRECTION ( 'NONE',  ( 0.000000000000000000, 0.000000000000000000, -1.000000000000000000 ) ) ;
#20982 = VERTEX_POINT ( 'NONE', #43910 ) ;
#20983 = VECTOR ( 'NONE', #6102, 1000.000000000000000 ) ;
#20984 = PLANE ( 'NONE',  #29847 ) ;
#20985 = VERTEX_POINT ( 'NONE', #20514 ) ;
#20986 = CARTESIAN_POINT ( 'NONE',  ( -305.0000000000000568, -123.5000000000000284, -15.24495751795539000 ) ) ;
#20987 = VERTEX_POINT ( 'NONE', #5483 ) ;
#20988 = DIRECTION ( 'NONE',  ( 0.000000000000000000, -1.000000000000000000, 0.000000000000000000 ) ) ;
#20989 = DIRECTION ( 'NONE',  ( -0.4031234292879792847, 0.000000000000000000, 0.9151456172430153524 ) ) ;
#20990 = VERTEX_POINT ( 'NONE', #51821 ) ;
#20991 = CARTESIAN_POINT ( 'NONE',  ( 59.80284513346456521, -177.1207230881787780, 62.45009659481583952 ) ) ;
#20992 = EDGE_LOOP ( 'NONE', ( #21074, #20799, #47687, #30195 ) ) ;
#20993 = EDGE_LOOP ( 'NONE', ( #36037, #8962, #25889, #4189 ) ) ;
#20994 = DIRECTION ( 'NONE',  ( -0.000000000000000000, -1.000000000000000000, -0.000000000000000000 ) ) ;
#20995 = DIRECTION ( 'NONE',  ( 0.4300652022765115712, 0.000000000000000000, 0.9027978299657477557 ) ) ;
#20996 = EDGE_CURVE ( 'NONE', #34425, #38590, #27873, .T. ) ;
#20997 = LINE ( 'NONE', #4703, #21330 ) ;
#20998 = EDGE_LOOP ( 'NONE', ( #7127, #40677, #38449, #37004 ) ) ;
#20999 = FACE_OUTER_BOUND ( 'NONE', #48407, .T. ) ;
#21000 = SHAPE_DEFINITION_REPRESENTATION ( #17186, #15639 ) ;
#21001 = DIRECTION ( 'NONE',  ( 0.000000000000000000, -1.000000000000000000, 0.000000000000000000 ) ) ;
#21002 = FACE_OUTER_BOUND ( 'NONE', #45959, .T. ) ;
#21003 = CARTESIAN_POINT ( 'NONE',  ( -336.3521761649654422, -123.5000000000000284, 0.000000000000000000 ) ) ;
#21004 = PLANE ( 'NONE',  #16452 ) ;
#21005 = VECTOR ( 'NONE', #11659, 1000.000000000000000 ) ;
#21006 = CIRCLE ( 'NONE', #26953, 125.0000000000000000 ) ;
#21007 = DIRECTION ( 'NONE',  ( -1.000000000000000000, -0.000000000000000000, 0.000000000000000000 ) ) ;
#21008 = ORIENTED_EDGE ( 'NONE', *, *, #48263, .T. ) ;
#21009 = CARTESIAN_POINT ( 'NONE',  ( -170.0000000000000284, -173.5000000000000284, 60.00000000000000000 ) ) ;
#21010 = DIRECTION ( 'NONE',  ( 0.000000000000000000, -1.000000000000000000, 0.000000000000000000 ) ) ;
#21011 = FACE_OUTER_BOUND ( 'NONE', #4276, .T. ) ;
#21012 = EDGE_LOOP ( 'NONE', ( #35322, #8379, #4965, #10066 ) ) ;
#21013 = ORIENTED_EDGE ( 'NONE', *, *, #18329, .T. ) ;
#21014 = ORIENTED_EDGE ( 'NONE', *, *, #7609, .F. ) ;
#21015 = LINE ( 'NONE', #8928, #3279 ) ;
#21016 = AXIS2_PLACEMENT_3D ( 'NONE', #22053, #49918, #29413 ) ;
#21017 = FACE_OUTER_BOUND ( 'NONE', #17283, .T. ) ;
#21018 = DIRECTION ( 'NONE',  ( 0.000000000000000000, 0.7485107481711089639, 0.6631226582407863113 ) ) ;
#21019 = PLANE ( 'NONE',  #41326 ) ;
#21020 = ORIENTED_EDGE ( 'NONE', *, *, #26594, .F. ) ;
#21021 = EDGE_CURVE ( 'NONE', #45109, #25441, #20004, .T. ) ;
#21022 = PLANE ( 'NONE',  #9850 ) ;
#21023 = CARTESIAN_POINT ( 'NONE',  ( -170.0000000000000284, -93.50000000000002842, 51.54700538379266561 ) ) ;
#21024 = ORIENTED_EDGE ( 'NONE', *, *, #16276, .F. ) ;
#21025 = DIRECTION ( 'NONE',  ( 1.000000000000000000, 0.000000000000000000, -0.000000000000000000 ) ) ;
#21026 = EDGE_CURVE ( 'NONE', #18514, #17157, #29130, .T. ) ;
#21027 = ORIENTED_EDGE ( 'NONE', *, *, #13185, .F. ) ;
#21028 = CARTESIAN_POINT ( 'NONE',  ( -339.1964088526558498, -180.6659093959934523, -14.60509510167853264 ) ) ;
#21029 = ORIENTED_EDGE ( 'NONE', *, *, #27908, .T. ) ;
#21030 = CARTESIAN_POINT ( 'NONE',  ( -170.0000000000000284, -173.5000000000000284, 60.00000000000000000 ) ) ;
#21031 = EDGE_CURVE ( 'NONE', #18239, #19986, #21498, .T. ) ;
#21032 = EDGE_CURVE ( 'NONE', #18605, #2316, #16319, .T. ) ;
#21033 = VECTOR ( 'NONE', #50266, 1000.000000000000114 ) ;
#21034 = AXIS2_PLACEMENT_3D ( 'NONE', #2963, #13766, #31860 ) ;
#21035 = CARTESIAN_POINT ( 'NONE',  ( -305.0000000000000568, -89.00580675195338642, -49.09328500076576773 ) ) ;
#21036 = CARTESIAN_POINT ( 'NONE',  ( -332.3517673607765914, -170.5607375887735770, 35.68215131113770155 ) ) ;
#21039 = EDGE_LOOP ( 'NONE', ( #28969, #21769, #34678, #51684 ) ) ;
#21038 = PLANE ( 'NONE',  #19939 ) ;
#21037 = CARTESIAN_POINT ( 'NONE',  ( -0.2934788161349695668, 58.14470866581338271, -16.45750525699328293 ) ) ;
#21040 = EDGE_CURVE ( 'NONE', #30980, #18160, #29630, .T. ) ;
#21041 = CARTESIAN_POINT ( 'NONE',  ( -166.2107720749849022, -189.7472609257535510, -38.92640747825594616 ) ) ;
#21042 = ORIENTED_EDGE ( 'NONE', *, *, #30492, .F. ) ;
#21043 = DIRECTION ( 'NONE',  ( 0.000000000000000000, -1.000000000000000000, -0.000000000000000000 ) ) ;
#21044 = CARTESIAN_POINT ( 'NONE',  ( -48.36085358058748085, -175.3837268820161057, -0.9929810960135100339 ) ) ;
#21045 = ORIENTED_EDGE ( 'NONE', *, *, #16040, .F. ) ;
#21046 = LINE ( 'NONE', #45488, #49379 ) ;
#21048 = FACE_OUTER_BOUND ( 'NONE', #23405, .T. ) ;
#21047 = CARTESIAN_POINT ( 'NONE',  ( -108.0638572795232335, -183.6283474603465606, 108.7464374498172504 ) ) ;
#21049 = ORIENTED_EDGE ( 'NONE', *, *, #2224, .F. ) ;
#21050 = LINE ( 'NONE', #8436, #28229 ) ;
#21051 = FACE_BOUND ( 'NONE', #26798, .T. ) ;
#21053 = VECTOR ( 'NONE', #23540, 1000.000000000000114 ) ;
#21052 = CARTESIAN_POINT ( 'NONE',  ( -164.6246685127424882, -175.3837268820161057, -46.20836643930983456 ) ) ;
#21054 = ORIENTED_EDGE ( 'NONE', *, *, #29542, .T. ) ;
#21055 = ADVANCED_FACE ( 'NONE', ( #20258 ), #32334, .T. ) ;
#21056 = PLANE ( 'NONE',  #45144 ) ;
#21057 = LINE ( 'NONE', #37074, #20691 ) ;
#21058 = CARTESIAN_POINT ( 'NONE',  ( -48.47912675150885065, -175.3837268820161057, 6.938893903907228378E-15 ) ) ;
#21059 = DIRECTION ( 'NONE',  ( 0.000000000000000000, 0.000000000000000000, -1.000000000000000000 ) ) ;
#21060 = VERTEX_POINT ( 'NONE', #44445 ) ;
#21061 = LINE ( 'NONE', #37618, #31509 ) ;
#21062 = LINE ( 'NONE', #32360, #18232 ) ;
#21063 = ORIENTED_EDGE ( 'NONE', *, *, #47132, .F. ) ;
#21064 = CARTESIAN_POINT ( 'NONE',  ( -330.4913330509368166, -116.8846903019842927, 58.63009191191280678 ) ) ;
#21065 = FACE_OUTER_BOUND ( 'NONE', #12076, .T. ) ;
#21066 = AXIS2_PLACEMENT_3D ( 'NONE', #31015, #46808, #23401 ) ;
#21067 = FACE_OUTER_BOUND ( 'NONE', #15548, .T. ) ;
#21068 = DIRECTION ( 'NONE',  ( 0.000000000000000000, 0.000000000000000000, -1.000000000000000000 ) ) ;
#21069 = VECTOR ( 'NONE', #51516, 1000.000000000000000 ) ;
#21070 = CARTESIAN_POINT ( 'NONE',  ( 2.669657140899374337, -193.5000000000000000, 114.0561348912355868 ) ) ;
#21071 = CARTESIAN_POINT ( 'NONE',  ( -63.43218022845228887, -193.5000000000000000, 124.1024020384604540 ) ) ;
#21072 = CARTESIAN_POINT ( 'NONE',  ( -47.50057025920934706, -193.5000000000000000, -0.2059786187410884151 ) ) ;
#21074 = ORIENTED_EDGE ( 'NONE', *, *, #2219, .F. ) ;
#21073 = DIRECTION ( 'NONE',  ( 0.000000000000000000, 1.000000000000000000, 0.000000000000000000 ) ) ;
#21075 = ORIENTED_EDGE ( 'NONE', *, *, #42366, .T. ) ;
#21076 = EDGE_CURVE ( 'NONE', #25441, #45944, #29893, .T. ) ;
#21077 = EDGE_CURVE ( 'NONE', #49045, #3432, #9935, .T. ) ;
#21078 = DIRECTION ( 'NONE',  ( 0.000000000000000000, 0.000000000000000000, -1.000000000000000000 ) ) ;
#21079 = DIRECTION ( 'NONE',  ( 1.000000000000000000, 0.000000000000000000, 0.000000000000000000 ) ) ;
#21080 = EDGE_LOOP ( 'NONE', ( #11624, #557, #13994, #20318 ) ) ;
#21081 = ORIENTED_EDGE ( 'NONE', *, *, #29301, .F. ) ;
#21082 = VECTOR ( 'NONE', #42615, 999.9999999999998863 ) ;
#21083 = VERTEX_POINT ( 'NONE', #42231 ) ;
#21084 = DIRECTION ( 'NONE',  ( 0.000000000000000000, -1.000000000000000000, 0.000000000000000000 ) ) ;
#21085 = EDGE_CURVE ( 'NONE', #32877, #6126, #25954, .T. ) ;
#21086 = PLANE ( 'NONE',  #48823 ) ;
#21087 = DIRECTION ( 'NONE',  ( 0.8757349421956379665, 0.000000000000000000, -0.4827922027307427477 ) ) ;
#21088 = ORIENTED_EDGE ( 'NONE', *, *, #2287, .F. ) ;
#21089 = ORIENTED_EDGE ( 'NONE', *, *, #33016, .T. ) ;
#21090 = EDGE_CURVE ( 'NONE', #5101, #27694, #22266, .T. ) ;
#21091 = DIRECTION ( 'NONE',  ( 0.08879589532292483933, 0.000000000000000000, 0.9960498426152178952 ) ) ;
#21093 = EDGE_LOOP ( 'NONE', ( #27486, #26593, #35867, #4856 ) ) ;
#21092 = CARTESIAN_POINT ( 'NONE',  ( -49.46816693883101124, -189.7472609257535510, -0.1476465640024848536 ) ) ;
#21094 = EDGE_CURVE ( 'NONE', #38778, #8625, #42766, .T. ) ;
#21095 = CARTESIAN_POINT ( 'NONE',  ( -330.4913330509368166, -123.5000000000000284, 0.000000000000000000 ) ) ;
#21096 = VERTEX_POINT ( 'NONE', #30404 ) ;
#21097 = PLANE ( 'NONE',  #47362 ) ;
#21098 = VECTOR ( 'NONE', #13568, 1000.000000000000000 ) ;
#21099 = EDGE_CURVE ( 'NONE', #51399, #6061, #33389, .T. ) ;
#21100 = VERTEX_POINT ( 'NONE', #25697 ) ;
#21101 = FACE_OUTER_BOUND ( 'NONE', #16345, .T. ) ;
#21102 = LINE ( 'NONE', #25062, #22312 ) ;
#21103 = AXIS2_PLACEMENT_3D ( 'NONE', #5947, #38750, #30109 ) ;
#21104 = CARTESIAN_POINT ( 'NONE',  ( -48.47912675150885065, -175.3837268820161057, 6.938893903907228378E-15 ) ) ;
#21105 = AXIS2_PLACEMENT_3D ( 'NONE', #37230, #1219, #22693 ) ;
#21106 = EDGE_LOOP ( 'NONE', ( #43987, #16220, #30489, #47609 ) ) ;
#21107 = VERTEX_POINT ( 'NONE', #26200 ) ;
#21108 = DIRECTION ( 'NONE',  ( 0.000000000000000000, 0.3546048870425331789, -0.9350162426854158326 ) ) ;
#21109 = CARTESIAN_POINT ( 'NONE',  ( 46.31065297101394407, -193.5000000000000000, 79.94433946042836681 ) ) ;
#21110 = ORIENTED_EDGE ( 'NONE', *, *, #36008, .F. ) ;
#21111 = DIRECTION ( 'NONE',  ( 0.000000000000000000, -1.000000000000000000, 0.000000000000000000 ) ) ;
#21112 = DIRECTION ( 'NONE',  ( -0.000000000000000000, 1.000000000000000000, -0.000000000000000000 ) ) ;
#21113 = EDGE_LOOP ( 'NONE', ( #1883, #41213, #15041, #2978 ) ) ;
#21114 = LINE ( 'NONE', #49518, #37639 ) ;
#21115 = VECTOR ( 'NONE', #31147, 1000.000000000000000 ) ;
#21116 = CARTESIAN_POINT ( 'NONE',  ( -332.3517673607765914, -111.9361751271348879, -57.91551518289410438 ) ) ;
#21117 = VERTEX_POINT ( 'NONE', #14147 ) ;
#21118 = CARTESIAN_POINT ( 'NONE',  ( -336.3521761649654422, -123.5000000000000284, 0.000000000000000000 ) ) ;
#21119 = ORIENTED_EDGE ( 'NONE', *, *, #9979, .T. ) ;
#21120 = VECTOR ( 'NONE', #48582, 1000.000000000000000 ) ;
#21121 = FACE_OUTER_BOUND ( 'NONE', #13384, .T. ) ;
#21122 = ORIENTED_EDGE ( 'NONE', *, *, #24731, .T. ) ;
#21123 = CARTESIAN_POINT ( 'NONE',  ( 73.87536152799695799, -175.3837268820161057, -25.58083653558413673 ) ) ;
#21124 = FACE_OUTER_BOUND ( 'NONE', #1039, .T. ) ;
#21125 = LINE ( 'NONE', #31915, #42509 ) ;
#21126 = DIRECTION ( 'NONE',  ( 0.000000000000000000, 1.000000000000000000, 0.000000000000000000 ) ) ;
#21127 = EDGE_LOOP ( 'NONE', ( #22702, #28232, #50520, #29766 ) ) ;
#21128 = CARTESIAN_POINT ( 'NONE',  ( -490.0000000000001137, -78.50000000000002842, 14.36509618646847386 ) ) ;
#21129 = EDGE_LOOP ( 'NONE', ( #36242, #22610, #4389, #31920 ) ) ;
#21130 = ADVANCED_FACE ( 'NONE', ( #33836 ), #38292, .T. ) ;
#21131 = ORIENTED_EDGE ( 'NONE', *, *, #36983, .F. ) ;
#21132 = DIRECTION ( 'NONE',  ( 0.000000000000000000, 0.000000000000000000, -1.000000000000000000 ) ) ;
#21134 = ORIENTED_EDGE ( 'NONE', *, *, #20670, .T. ) ;
#21133 = FACE_OUTER_BOUND ( 'NONE', #38186, .T. ) ;
#21135 = VECTOR ( 'NONE', #15557, 1000.000000000000114 ) ;
#21136 = EDGE_CURVE ( 'NONE', #30781, #23810, #6245, .T. ) ;
#21137 = ORIENTED_EDGE ( 'NONE', *, *, #45317, .T. ) ;
#21138 = EDGE_CURVE ( 'NONE', #31867, #21525, #14901, .T. ) ;
#21139 = DIRECTION ( 'NONE',  ( 0.000000000000000000, 0.000000000000000000, 1.000000000000000000 ) ) ;
#21140 = ADVANCED_FACE ( 'NONE', ( #42497 ), #2311, .T. ) ;
#21141 = AXIS2_PLACEMENT_3D ( 'NONE', #23462, #27124, #35275 ) ;
#21142 = ADVANCED_FACE ( 'NONE', ( #50152 ), #46205, .F. ) ;
#21143 = VECTOR ( 'NONE', #51793, 1000.000000000000000 ) ;
#21144 = LINE ( 'NONE', #17990, #20383 ) ;
#21145 = DIRECTION ( 'NONE',  ( 0.9785564922995046988, 0.000000000000000000, -0.2059786187410953262 ) ) ;
#21146 = EDGE_LOOP ( 'NONE', ( #44772, #33022, #850, #18130 ) ) ;
#21147 = DIRECTION ( 'NONE',  ( -0.000000000000000000, 1.000000000000000000, -0.000000000000000000 ) ) ;
#21148 = EDGE_CURVE ( 'NONE', #33963, #37409, #2562, .T. ) ;
#21149 = ORIENTED_EDGE ( 'NONE', *, *, #33660, .F. ) ;
#21150 = CARTESIAN_POINT ( 'NONE',  ( -336.3521761649654422, -182.3871109312487420, -4.498567634386014369 ) ) ;
#21151 = LINE ( 'NONE', #49016, #30027 ) ;
#21152 = ADVANCED_FACE ( 'NONE', ( #41726 ), #10433, .F. ) ;
#21153 = CARTESIAN_POINT ( 'NONE',  ( -336.3521761649654422, -174.3267994849386184, -31.88473700876087591 ) ) ;
#21154 = CARTESIAN_POINT ( 'NONE',  ( 61.06976976088564157, -189.7472609257535510, -60.19999396110169698 ) ) ;
#21155 = VERTEX_POINT ( 'NONE', #50655 ) ;
#21156 = CIRCLE ( 'NONE', #27854, 16.00000000000000000 ) ;
#21157 = VERTEX_POINT ( 'NONE', #38801 ) ;
#21158 = EDGE_CURVE ( 'NONE', #33644, #6394, #40907, .T. ) ;
#21159 = ORIENTED_EDGE ( 'NONE', *, *, #16, .T. ) ;
#21160 = CARTESIAN_POINT ( 'NONE',  ( -339.1964088526558498, -162.2499814621209850, 44.49369547121574442 ) ) ;
#21161 = CARTESIAN_POINT ( 'NONE',  ( -171.2727421180348415, -193.5000000000000000, 23.38221600314377113 ) ) ;
#21162 = CIRCLE ( 'NONE', #8585, 125.0000000000000000 ) ;
#21163 = AXIS2_PLACEMENT_3D ( 'NONE', #31174, #47224, #23310 ) ;
#21164 = EDGE_CURVE ( 'NONE', #43502, #39314, #50981, .T. ) ;
#21165 = FACE_BOUND ( 'NONE', #14338, .T. ) ;
#21166 = CARTESIAN_POINT ( 'NONE',  ( 73.66680038934278230, -189.7472609257535510, -26.55884942729568365 ) ) ;
#21167 = EDGE_LOOP ( 'NONE', ( #45745, #7157, #11770, #44814 ) ) ;
#21168 = EDGE_CURVE ( 'NONE', #3689, #38204, #23296, .T. ) ;
#21169 = ADVANCED_FACE ( 'NONE', ( #11980 ), #32218, .T. ) ;
#21170 = EDGE_CURVE ( 'NONE', #25060, #16474, #8053, .T. ) ;
#21171 = ORIENTED_EDGE ( 'NONE', *, *, #24411, .T. ) ;
#21173 = ORIENTED_EDGE ( 'NONE', *, *, #49768, .F. ) ;
#21172 = FACE_OUTER_BOUND ( 'NONE', #21730, .T. ) ;
#21174 = VERTEX_POINT ( 'NONE', #19620 ) ;
#21175 = CARTESIAN_POINT ( 'NONE',  ( -170.0000000000000284, -113.5000000000000000, -40.00000000000001421 ) ) ;
#21176 = CARTESIAN_POINT ( 'NONE',  ( -330.4913330509368166, -68.51134412508150717, 21.38919645685156112 ) ) ;
#21177 = CIRCLE ( 'NONE', #48036, 125.0000000000000000 ) ;
#21178 = CARTESIAN_POINT ( 'NONE',  ( -330.4913330509368166, -90.39567187580871632, -48.84008046109136814 ) ) ;
#21179 = CARTESIAN_POINT ( 'NONE',  ( 46.00000000000000711, 33.00000000000000000, -56.99999999999999289 ) ) ;
#21180 = CARTESIAN_POINT ( 'NONE',  ( 26.62880456707186383, -175.3837268820161057, 98.66508442481512020 ) ) ;
#21181 = EDGE_LOOP ( 'NONE', ( #9363, #416, #1423, #3137 ) ) ;
#21182 = DIRECTION ( 'NONE',  ( 0.000000000000000000, -2.611337072503753781E-13, -1.000000000000000000 ) ) ;
#21183 = ORIENTED_EDGE ( 'NONE', *, *, #46846, .T. ) ;
#21184 = ADVANCED_FACE ( 'NONE', ( #31185 ), #11469, .T. ) ;
#21185 = CIRCLE ( 'NONE', #6079, 4.999999999999997335 ) ;
#21186 = EDGE_LOOP ( 'NONE', ( #48858, #44491, #40443, #33396 ) ) ;
#21187 = PLANE ( 'NONE',  #31292 ) ;
#21188 = LINE ( 'NONE', #24353, #6033 ) ;
#21189 = ORIENTED_EDGE ( 'NONE', *, *, #44246, .T. ) ;
#21190 = CARTESIAN_POINT ( 'NONE',  ( -47.60339180931321579, -183.6283474603465606, -0.4827922027307358088 ) ) ;
#21191 = CARTESIAN_POINT ( 'NONE',  ( -336.3521761649654422, -159.1821513111375452, -47.06073758877369073 ) ) ;
#21192 = CARTESIAN_POINT ( 'NONE',  ( -173.1763543514842070, -193.5000000000000000, 8.694908215728892387 ) ) ;
#21193 = ORIENTED_EDGE ( 'NONE', *, *, #12262, .T. ) ;
#21194 = CARTESIAN_POINT ( 'NONE',  ( -69.77312546433407192, -193.5000000000000000, 123.1729094355500109 ) ) ;
#21195 = FACE_OUTER_BOUND ( 'NONE', #20362, .T. ) ;
#21196 = VECTOR ( 'NONE', #23653, 1000.000000000000000 ) ;
#21197 = AXIS2_PLACEMENT_3D ( 'NONE', #41085, #28466, #12177 ) ;
#21198 = CARTESIAN_POINT ( 'NONE',  ( -336.3521761649654422, -178.0871407151310279, 22.44790492310219676 ) ) ;
#21199 = FACE_BOUND ( 'NONE', #18421, .T. ) ;
#21200 = VERTEX_POINT ( 'NONE', #39333 ) ;
#21201 = VECTOR ( 'NONE', #4642, 1000.000000000000114 ) ;
#21202 = VECTOR ( 'NONE', #35222, 1000.000000000000000 ) ;
#21203 = DIRECTION ( 'NONE',  ( -0.000000000000000000, 0.8229838658936634577, 0.5680647467311457088 ) ) ;
#21204 = ORIENTED_EDGE ( 'NONE', *, *, #33669, .T. ) ;
#21205 = DIRECTION ( 'NONE',  ( 0.000000000000000000, 1.000000000000000000, -0.000000000000000000 ) ) ;
#21206 = ADVANCED_FACE ( 'NONE', ( #24096 ), #47484, .F. ) ;
#21207 = ORIENTED_EDGE ( 'NONE', *, *, #32883, .T. ) ;
#21208 = EDGE_CURVE ( 'NONE', #16640, #49884, #43272, .T. ) ;
#21209 = DIRECTION ( 'NONE',  ( 0.1182731709213730997, 0.000000000000000000, -0.9929810960135161402 ) ) ;
#21210 = CLOSED_SHELL ( 'NONE', ( #7393, #11973, #48689, #3011, #25257, #42751, #1816, #50114, #33355, #41780, #12151, #46137, #40465, #29791, #3534, #50466, #4803, #40061, #41032, #49219, #21169, #14120, #3884 ) ) ;
#21211 = ORIENTED_EDGE ( 'NONE', *, *, #14382, .T. ) ;
#21212 = ADVANCED_FACE ( 'NONE', ( #26981 ), #19115, .T. ) ;
#21213 = ADVANCED_FACE ( 'NONE', ( #20137 ), #31439, .T. ) ;
#21214 = CARTESIAN_POINT ( 'NONE',  ( -74.51199343215203896, -177.1207230881787780, -122.2591094863194598 ) ) ;
#21215 = CARTESIAN_POINT ( 'NONE',  ( 63.82222181224017277, -193.5000000000000000, 52.57768177182522606 ) ) ;
#21217 = ORIENTED_EDGE ( 'NONE', *, *, #39035, .F. ) ;
#21216 = CARTESIAN_POINT ( 'NONE',  ( -49.21696003055058810, -189.7472609257535510, 0.6749830015182108900 ) ) ;
#21218 = AXIS2_PLACEMENT_3D ( 'NONE', #12523, #28790, #44841 ) ;
#21219 = DIRECTION ( 'NONE',  ( 0.000000000000000000, 0.000000000000000000, -1.000000000000000000 ) ) ;
#21220 = ORIENTED_EDGE ( 'NONE', *, *, #25192, .F. ) ;
#21221 = ORIENTED_EDGE ( 'NONE', *, *, #18248, .F. ) ;
#21222 = AXIS2_PLACEMENT_3D ( 'NONE', #32582, #44676, #45216 ) ;
#21223 = ORIENTED_EDGE ( 'NONE', *, *, #5424, .T. ) ;
#21224 = CARTESIAN_POINT ( 'NONE',  ( -126.2322430781613605, -177.1207230881787780, 97.87467957288053810 ) ) ;
#21225 = LINE ( 'NONE', #45159, #10807 ) ;
#21226 = ADVANCED_FACE ( 'NONE', ( #27505 ), #39829, .T. ) ;
#21227 = VERTEX_POINT ( 'NONE', #39573 ) ;
#21228 = CARTESIAN_POINT ( 'NONE',  ( -155.9608607592036833, -193.5000000000000000, 63.81752780153064464 ) ) ;
#21229 = CARTESIAN_POINT ( 'NONE',  ( -305.0000000000000568, -84.08827740916061089, 45.24064679492014562 ) ) ;
#21230 = DIRECTION ( 'NONE',  ( -0.000000000000000000, 1.000000000000000000, -0.000000000000000000 ) ) ;
#21231 = VERTEX_POINT ( 'NONE', #51693 ) ;
#21232 = CIRCLE ( 'NONE', #23733, 1.951623109906645226 ) ;
#21233 = AXIS2_PLACEMENT_3D ( 'NONE', #29604, #29083, #45151 ) ;
#21234 = ADVANCED_FACE ( 'NONE', ( #35131 ), #31961, .T. ) ;
#21235 = CARTESIAN_POINT ( 'NONE',  ( 75.78974234412359579, -193.5000000000000000, 13.49993235881449394 ) ) ;
#21236 = DIRECTION ( 'NONE',  ( 0.000000000000000000, 0.000000000000000000, -1.000000000000000000 ) ) ;
#21237 = ORIENTED_EDGE ( 'NONE', *, *, #41764, .T. ) ;
#21240 = ORIENTED_EDGE ( 'NONE', *, *, #41356, .F. ) ;
#21239 = LINE ( 'NONE', #41720, #4600 ) ;
#21238 = CARTESIAN_POINT ( 'NONE',  ( -330.4913330509368166, -173.1613497474970416, -33.67120938215288817 ) ) ;
#21241 = VECTOR ( 'NONE', #7173, 1000.000000000000000 ) ;
#21242 = EDGE_LOOP ( 'NONE', ( #6798, #3332, #40078, #13123 ) ) ;
#21243 = FACE_OUTER_BOUND ( 'NONE', #26879, .T. ) ;
#21244 = ORIENTED_EDGE ( 'NONE', *, *, #11162, .F. ) ;
#21245 = LINE ( 'NONE', #41456, #32297 ) ;
#21246 = ORIENTED_EDGE ( 'NONE', *, *, #6987, .T. ) ;
#21247 = CARTESIAN_POINT ( 'NONE',  ( -1.600401561467127700E-24, 58.14470866581338271, -16.45750525699328293 ) ) ;
#21248 = AXIS2_PLACEMENT_3D ( 'NONE', #6217, #38257, #10928 ) ;
#21249 = CARTESIAN_POINT ( 'NONE',  ( -2.700932609314997457, -183.6283474603465606, -116.3157639405751809 ) ) ;
#21250 = VERTEX_POINT ( 'NONE', #15695 ) ;
#21251 = PLANE ( 'NONE',  #47701 ) ;
#21252 = ORIENTED_EDGE ( 'NONE', *, *, #8935, .F. ) ;
#21253 = VERTEX_POINT ( 'NONE', #3857 ) ;
#21254 = FACE_OUTER_BOUND ( 'NONE', #11121, .T. ) ;
#21255 = CARTESIAN_POINT ( 'NONE',  ( -336.3521761649654422, -111.9361751271348879, -57.91551518289410438 ) ) ;
#21256 = CARTESIAN_POINT ( 'NONE',  ( -332.3517673607765914, -70.49953203435293858, 25.97334715265942151 ) ) ;
#21257 = CARTESIAN_POINT ( 'NONE',  ( -172.4792251663439231, -177.1207230881787780, 0.3215015308249278281 ) ) ;
#21258 = ORIENTED_EDGE ( 'NONE', *, *, #47450, .F. ) ;
#21259 = VECTOR ( 'NONE', #5836, 1000.000000000000114 ) ;
#21260 = CARTESIAN_POINT ( 'NONE',  ( -143.3583119192899744, -177.1207230881787780, -81.38144888055202841 ) ) ;
#21261 = APPLICATION_PROTOCOL_DEFINITION ( 'draft international standard', 'automotive_design', 1998, #2506 ) ;
#21262 = LINE ( 'NONE', #13378, #43083 ) ;
#21263 = LINE ( 'NONE', #31582, #13620 ) ;
#21264 = CARTESIAN_POINT ( 'NONE',  ( -339.1964088526558498, -172.3400804610915600, -33.10432812419107051 ) ) ;
#21265 = DIRECTION ( 'NONE',  ( 0.9008942672012963948, 0.4327645661435914337, 0.03323175611351393555 ) ) ;
#21266 = VECTOR ( 'NONE', #8727, 1000.000000000000000 ) ;
#21267 = DIRECTION ( 'NONE',  ( 0.2348860457809842095, 0.000000000000000000, -0.9720229140804107493 ) ) ;
#21268 = ORIENTED_EDGE ( 'NONE', *, *, #25165, .T. ) ;
#21269 = CARTESIAN_POINT ( 'NONE',  ( -170.0000000000000284, -123.5000000000000284, -15.24495751795539000 ) ) ;
#21270 = CARTESIAN_POINT ( 'NONE',  ( 40.30419662299490113, -183.6283474603465606, -87.99159897727903967 ) ) ;
#21271 = ORIENTED_EDGE ( 'NONE', *, *, #43053, .T. ) ;
#21272 = ADVANCED_FACE ( 'NONE', ( #31711 ), #47755, .F. ) ;
#21273 = ORIENTED_EDGE ( 'NONE', *, *, #42247, .F. ) ;
#21274 = VECTOR ( 'NONE', #39692, 1000.000000000000000 ) ;
#21275 = VERTEX_POINT ( 'NONE', #7284 ) ;
#21276 = DIRECTION ( 'NONE',  ( -1.000000000000000000, 3.701062773504747805E-15, -9.758900497077197755E-15 ) ) ;
#21277 = AXIS2_PLACEMENT_3D ( 'NONE', #22269, #25700, #13878 ) ;
#21278 = FACE_OUTER_BOUND ( 'NONE', #13026, .T. ) ;
#21279 = CARTESIAN_POINT ( 'NONE',  ( -48.47912675150885065, -213.5000000000000000, 6.938893903907228378E-15 ) ) ;
#21280 = DIRECTION ( 'NONE',  ( 0.000000000000000000, 0.000000000000000000, 1.000000000000000000 ) ) ;
#21281 = VERTEX_POINT ( 'NONE', #27754 ) ;
#21282 = DIRECTION ( 'NONE',  ( 5.399917434947259359E-17, 1.000000000000000000, -0.000000000000000000 ) ) ;
#21283 = AXIS2_PLACEMENT_3D ( 'NONE', #19843, #7510, #28241 ) ;
#21284 = DIRECTION ( 'NONE',  ( 0.000000000000000000, -0.1205366802553095307, 0.9927088740980556381 ) ) ;
#21285 = PLANE ( 'NONE',  #29843 ) ;
#21286 = VERTEX_POINT ( 'NONE', #43787 ) ;
#21287 = DIRECTION ( 'NONE',  ( 0.000000000000000000, 0.000000000000000000, -1.000000000000000000 ) ) ;
#21288 = VERTEX_POINT ( 'NONE', #19880 ) ;
#21289 = EDGE_CURVE ( 'NONE', #24589, #47106, #6534, .T. ) ;
#21290 = DIRECTION ( 'NONE',  ( -0.000000000000000000, -1.000000000000000000, 0.000000000000000000 ) ) ;
#21291 = AXIS2_PLACEMENT_3D ( 'NONE', #11559, #19690, #36238 ) ;
#21292 = VERTEX_POINT ( 'NONE', #44048 ) ;
#21293 = AXIS2_PLACEMENT_3D ( 'NONE', #41751, #41216, #37794 ) ;
#21294 = ADVANCED_FACE ( 'NONE', ( #23046 ), #4122, .T. ) ;
#21295 = LINE ( 'NONE', #20777, #9795 ) ;
#21296 = ORIENTED_EDGE ( 'NONE', *, *, #26761, .F. ) ;
#21299 = ORIENTED_EDGE ( 'NONE', *, *, #10157, .F. ) ;
#21298 = CARTESIAN_POINT ( 'NONE',  ( -48.88225018079683082, -193.5000000000000000, 0.9151456172430223468 ) ) ;
#21297 = CARTESIAN_POINT ( 'NONE',  ( -339.1964088526558498, -138.1050951016783301, 57.16590939599346655 ) ) ;
#21300 = PLANE ( 'NONE',  #23955 ) ;
#21301 = ORIENTED_EDGE ( 'NONE', *, *, #51189, .T. ) ;
#21302 = DIRECTION ( 'NONE',  ( -0.4566292373937200777, 0.000000000000000000, 0.8896570909947436601 ) ) ;
#21303 = PLANE ( 'NONE',  #23279 ) ;
#21304 = ORIENTED_EDGE ( 'NONE', *, *, #27114, .T. ) ;
#21305 = EDGE_CURVE ( 'NONE', #7980, #10791, #17517, .T. ) ;
#21306 = DIRECTION ( 'NONE',  ( -1.000000000000000000, -0.000000000000000000, -0.000000000000000000 ) ) ;
#21309 = ORIENTED_EDGE ( 'NONE', *, *, #12521, .F. ) ;
#21308 = FACE_OUTER_BOUND ( 'NONE', #10048, .T. ) ;
#21307 = LINE ( 'NONE', #49687, #15734 ) ;
#21310 = VECTOR ( 'NONE', #39616, 1000.000000000000114 ) ;
#21311 = ORIENTED_EDGE ( 'NONE', *, *, #22156, .T. ) ;
#21312 = APPLICATION_CONTEXT ( 'automotive_design' ) ;
#21313 = DIRECTION ( 'NONE',  ( 1.000000000000000000, -0.000000000000000000, -0.000000000000000000 ) ) ;
#21314 = DIRECTION ( 'NONE',  ( 0.000000000000000000, 0.000000000000000000, 1.000000000000000000 ) ) ;
#21315 = DIRECTION ( 'NONE',  ( 0.000000000000000000, 0.000000000000000000, -1.000000000000000000 ) ) ;
#21316 = EDGE_LOOP ( 'NONE', ( #5962, #14273, #34888, #18556 ) ) ;
#21317 = LINE ( 'NONE', #6070, #22479 ) ;
#21318 = CARTESIAN_POINT ( 'NONE',  ( -111.3295483157475445, -189.7472609257535510, 108.0501018472332504 ) ) ;
#21319 = PLANE ( 'NONE',  #52001 ) ;
#21320 = CARTESIAN_POINT ( 'NONE',  ( 60.58466639580034752, -189.7472609257535510, -61.07445476073404222 ) ) ;
#21321 = VERTEX_POINT ( 'NONE', #28779 ) ;
#21322 = LINE ( 'NONE', #41536, #4485 ) ;
#21323 = DIRECTION ( 'NONE',  ( 0.000000000000000000, 0.000000000000000000, 1.000000000000000000 ) ) ;
#21324 = EDGE_CURVE ( 'NONE', #30315, #27694, #50168, .T. ) ;
#21325 = CARTESIAN_POINT ( 'NONE',  ( -332.3517673607765914, -140.1754235130667610, -56.65561927338005432 ) ) ;
#21326 = ORIENTED_EDGE ( 'NONE', *, *, #14448, .T. ) ;
#21327 = LINE ( 'NONE', #49468, #4667 ) ;
#21328 = CARTESIAN_POINT ( 'NONE',  ( -260.0000000000000000, -113.5000000000000000, 60.00000000000000711 ) ) ;
#21329 = VECTOR ( 'NONE', #12774, 1000.000000000000000 ) ;
#21330 = VECTOR ( 'NONE', #49383, 1000.000000000000000 ) ;
#21331 = DIRECTION ( 'NONE',  ( 0.000000000000000000, -0.000000000000000000, 1.000000000000000000 ) ) ;
#21332 = CARTESIAN_POINT ( 'NONE',  ( -170.0000000000000284, -130.6726371812771959, -60.00000000000000711 ) ) ;
#21333 = EDGE_CURVE ( 'NONE', #33835, #43754, #40607, .T. ) ;
#21334 = VECTOR ( 'NONE', #37216, 1000.000000000000114 ) ;
#21335 = CARTESIAN_POINT ( 'NONE',  ( -160.0000000000000284, -123.5000000000000284, -41.63467731922663972 ) ) ;
#21336 = EDGE_CURVE ( 'NONE', #43700, #10047, #36949, .T. ) ;
#21337 = DIRECTION ( 'NONE',  ( -0.1182731709213660498, 0.000000000000000000, 0.9929810960135169173 ) ) ;
#21338 = FACE_OUTER_BOUND ( 'NONE', #29090, .T. ) ;
#21340 = ORIENTED_EDGE ( 'NONE', *, *, #47378, .F. ) ;
#21339 = DIRECTION ( 'NONE',  ( -0.000000000000000000, 1.000000000000000000, -0.000000000000000000 ) ) ;
#21341 = ORIENTED_EDGE ( 'NONE', *, *, #15986, .F. ) ;
#21342 = CARTESIAN_POINT ( 'NONE',  ( -339.1964088526558498, -71.49045607248213230, 27.86139516340826106 ) ) ;
#21343 = AXIS2_PLACEMENT_3D ( 'NONE', #42426, #38730, #29819 ) ;
#21344 = CARTESIAN_POINT ( 'NONE',  ( -49.38192458147459973, -175.3837268820161057, 0.4300652022765185656 ) ) ;
#21346 = EDGE_LOOP ( 'NONE', ( #17684, #23374, #18095, #5039 ) ) ;
#21345 = DIRECTION ( 'NONE',  ( -0.000000000000000000, 1.000000000000000000, -0.000000000000000000 ) ) ;
#21347 = ORIENTED_EDGE ( 'NONE', *, *, #24352, .T. ) ;
#21348 = ORIENTED_EDGE ( 'NONE', *, *, #15728, .T. ) ;
#21349 = EDGE_CURVE ( 'NONE', #23109, #18846, #48259, .T. ) ;
#21350 = CARTESIAN_POINT ( 'NONE',  ( -109.0835867659424281, -183.6283474603465606, -109.3256576763155010 ) ) ;
#21351 = PLANE ( 'NONE',  #22779 ) ;
#21352 = DIRECTION ( 'NONE',  ( 0.000000000000000000, 0.000000000000000000, 1.000000000000000000 ) ) ;
#21353 = ORIENTED_EDGE ( 'NONE', *, *, #1884, .T. ) ;
#21354 = CARTESIAN_POINT ( 'NONE',  ( 0.000000000000000000, -53.50000000000000000, 0.000000000000000000 ) ) ;
#21356 = VERTEX_POINT ( 'NONE', #32486 ) ;
#21355 = DIRECTION ( 'NONE',  ( 0.000000000000000000, 1.000000000000000000, 0.000000000000000000 ) ) ;
#21357 = CARTESIAN_POINT ( 'NONE',  ( 76.46082103836693022, -175.3837268820161057, 3.874202661595785191 ) ) ;
#21358 = VECTOR ( 'NONE', #38090, 1000.000000000000000 ) ;
#21359 = ORIENTED_EDGE ( 'NONE', *, *, #18207, .T. ) ;
#21360 = CARTESIAN_POINT ( 'NONE',  ( -332.3517673607765914, -70.49953203435293858, 25.97334715265942151 ) ) ;
#21361 = VERTEX_POINT ( 'NONE', #21176 ) ;
#21362 = AXIS2_PLACEMENT_3D ( 'NONE', #43946, #7936, #23969 ) ;
#21363 = PLANE ( 'NONE',  #2284 ) ;
#21364 = FACE_OUTER_BOUND ( 'NONE', #11137, .T. ) ;
#21365 = DIRECTION ( 'NONE',  ( -8.718379230999705894E-17, 0.9350162426854158326, 0.3546048870425331789 ) ) ;
#21366 = AXIS2_PLACEMENT_3D ( 'NONE', #43224, #15133, #6725 ) ;
#21367 = ORIENTED_EDGE ( 'NONE', *, *, #4849, .T. ) ;
#21368 = ORIENTED_EDGE ( 'NONE', *, *, #3848, .T. ) ;
#21369 = CARTESIAN_POINT ( 'NONE',  ( -47.57632892154310866, -175.3837268820161057, -0.4300652022765113491 ) ) ;
#21370 = DIRECTION ( 'NONE',  ( -0.9266896074318291543, 0.000000000000000000, -0.3758275821142488260 ) ) ;
#21371 = ORIENTED_EDGE ( 'NONE', *, *, #50286, .T. ) ;
#21372 = LINE ( 'NONE', #6392, #29920 ) ;
#21373 = EDGE_CURVE ( 'NONE', #49425, #46727, #12752, .T. ) ;
#21374 = EDGE_CURVE ( 'NONE', #31030, #34090, #4624, .T. ) ;
#21375 = ORIENTED_EDGE ( 'NONE', *, *, #39775, .T. ) ;
#21376 = FACE_BOUND ( 'NONE', #40266, .T. ) ;
#21377 = VECTOR ( 'NONE', #40018, 1000.000000000000000 ) ;
#21378 = CARTESIAN_POINT ( 'NONE',  ( -330.4913330509368166, -64.86990808808705822, 6.615309698014281814 ) ) ;
#21379 = VERTEX_POINT ( 'NONE', #40346 ) ;
#21380 = CARTESIAN_POINT ( 'NONE',  ( 2.669657140899374337, -193.5000000000000000, 114.0561348912355868 ) ) ;
#21381 = ORIENTED_EDGE ( 'NONE', *, *, #26000, .F. ) ;
#21382 = CARTESIAN_POINT ( 'NONE',  ( -172.3973245609188041, -193.5000000000000000, 4.503971736581664054 ) ) ;
#21383 = DIRECTION ( 'NONE',  ( 0.2348860457809842095, 0.000000000000000000, -0.9720229140804107493 ) ) ;
#21384 = ORIENTED_EDGE ( 'NONE', *, *, #35627, .T. ) ;
#21385 = DIRECTION ( 'NONE',  ( -0.4827922027307551267, 0.000000000000000000, 0.8757349421956311941 ) ) ;
#21386 = FACE_OUTER_BOUND ( 'NONE', #15415, .T. ) ;
#21387 = DIRECTION ( 'NONE',  ( 0.2920567706369764371, 0.000000000000000000, -0.9564009842765223146 ) ) ;
#21388 = EDGE_CURVE ( 'NONE', #13133, #45030, #4366, .T. ) ;
#21389 = DIRECTION ( 'NONE',  ( 0.000000000000000000, -0.000000000000000000, 1.000000000000000000 ) ) ;
#21390 = ADVANCED_FACE ( 'NONE', ( #24339 ), #29315, .T. ) ;
#21391 = ORIENTED_EDGE ( 'NONE', *, *, #42019, .T. ) ;
#21392 = CARTESIAN_POINT ( 'NONE',  ( 29.90148147319959193, -183.6283474603465606, 96.08646119224013660 ) ) ;
#21393 = VERTEX_POINT ( 'NONE', #13295 ) ;
#21394 = ORIENTED_EDGE ( 'NONE', *, *, #13453, .T. ) ;
#21395 = EDGE_CURVE ( 'NONE', #6231, #1159, #1187, .T. ) ;
#21396 = VECTOR ( 'NONE', #22558, 1000.000000000000341 ) ;
#21397 = LINE ( 'NONE', #33498, #44481 ) ;
#21399 = ORIENTED_EDGE ( 'NONE', *, *, #22045, .F. ) ;
#21398 = DIRECTION ( 'NONE',  ( 0.3482016354343995812, 0.000000000000000000, -0.9374196611341205632 ) ) ;
#21400 = AXIS2_PLACEMENT_3D ( 'NONE', #16672, #11917, #31897 ) ;
#21401 = AXIS2_PLACEMENT_3D ( 'NONE', #40117, #31200, #35657 ) ;
#21402 = VERTEX_POINT ( 'NONE', #28526 ) ;
#21403 = CARTESIAN_POINT ( 'NONE',  ( -365.0000000000001137, -78.50000000000002842, 0.000000000000000000 ) ) ;
#21404 = DIRECTION ( 'NONE',  ( 0.000000000000000000, 0.000000000000000000, 1.000000000000000000 ) ) ;
#21405 = ORIENTED_EDGE ( 'NONE', *, *, #42569, .T. ) ;
#21406 = DIRECTION ( 'NONE',  ( -0.02963332782257007553, 0.000000000000000000, 0.9995608365087941261 ) ) ;
#21407 = AXIS2_PLACEMENT_3D ( 'NONE', #18132, #42037, #5540 ) ;
#21408 = ORIENTED_EDGE ( 'NONE', *, *, #27494, .F. ) ;
#21409 = DIRECTION ( 'NONE',  ( -0.000000000000000000, -0.5000000000000013323, 0.8660254037844380415 ) ) ;
#21410 = DIRECTION ( 'NONE',  ( 0.000000000000000000, 0.000000000000000000, 1.000000000000000000 ) ) ;
#21411 = AXIS2_PLACEMENT_3D ( 'NONE', #25601, #30319, #30072 ) ;
#21413 = CIRCLE ( 'NONE', #44945, 125.0000000000000000 ) ;
#21412 = DIRECTION ( 'NONE',  ( -0.000000000000000000, -0.2393156642875615969, -0.9709418174260511236 ) ) ;
#21414 = LINE ( 'NONE', #49286, #48387 ) ;
#21415 = EDGE_LOOP ( 'NONE', ( #42370, #22868, #14802, #17739 ) ) ;
#21416 = VERTEX_POINT ( 'NONE', #44569 ) ;
#21417 = ORIENTED_EDGE ( 'NONE', *, *, #19038, .T. ) ;
#21418 = VECTOR ( 'NONE', #40158, 1000.000000000000000 ) ;
#21419 = PLANE ( 'NONE',  #24937 ) ;
#21420 = CARTESIAN_POINT ( 'NONE',  ( 2.066935079424583765, -193.5000000000000000, -114.3245189510257802 ) ) ;
#21421 = DIRECTION ( 'NONE',  ( -0.000000000000000000, -1.000000000000000000, 0.000000000000000000 ) ) ;
#21422 = PLANE ( 'NONE',  #33110 ) ;
#21423 = VERTEX_POINT ( 'NONE', #44834 ) ;
#21424 = ORIENTED_EDGE ( 'NONE', *, *, #39292, .T. ) ;
#21426 = ORIENTED_EDGE ( 'NONE', *, *, #48800, .T. ) ;
#21425 = CARTESIAN_POINT ( 'NONE',  ( -149.5539421794694306, -175.3837268820161057, 73.54509967498654532 ) ) ;
#21427 = EDGE_LOOP ( 'NONE', ( #30208, #9803, #6205, #3643 ) ) ;
#21428 = AXIS2_PLACEMENT_3D ( 'NONE', #37402, #49519, #26614 ) ;
#21429 = DIRECTION ( 'NONE',  ( -0.000000000000000000, 1.000000000000000000, -0.000000000000000000 ) ) ;
#21430 = DIRECTION ( 'NONE',  ( 1.000000000000000000, -0.000000000000000000, -0.000000000000000000 ) ) ;
#21431 = CIRCLE ( 'NONE', #18922, 4.000000000000003553 ) ;
#21432 = VECTOR ( 'NONE', #4521, 1000.000000000000000 ) ;
#21433 = ADVANCED_FACE ( 'NONE', ( #12242 ), #48784, .T. ) ;
#21434 = CARTESIAN_POINT ( 'NONE',  ( -332.3517673607765914, -172.9832938399466684, -32.17247266903247294 ) ) ;
#21435 = ADVANCED_FACE ( 'NONE', ( #4902 ), #940, .T. ) ;
#21436 = ADVANCED_FACE ( 'NONE', ( #32989 ), #49039, .T. ) ;
#21437 = CARTESIAN_POINT ( 'NONE',  ( -41.90263914168910730, -189.7472609257535510, -124.8268793598473536 ) ) ;
#21438 = VERTEX_POINT ( 'NONE', #45111 ) ;
#21439 = DIRECTION ( 'NONE',  ( 0.000000000000000000, 0.000000000000000000, 1.000000000000000000 ) ) ;
#21440 = ORIENTED_EDGE ( 'NONE', *, *, #966, .T. ) ;
#21441 = VECTOR ( 'NONE', #6984, 1000.000000000000000 ) ;
#21442 = EDGE_CURVE ( 'NONE', #8221, #36738, #31684, .T. ) ;
#21443 = EDGE_CURVE ( 'NONE', #3275, #18160, #48472, .T. ) ;
#21444 = ORIENTED_EDGE ( 'NONE', *, *, #21021, .F. ) ;
#21445 = CARTESIAN_POINT ( 'NONE',  ( -336.3521761649654422, -132.2320517616439020, -58.37307289257706344 ) ) ;
#21446 = ADVANCED_FACE ( 'NONE', ( #37459 ), #13813, .F. ) ;
#21447 = VECTOR ( 'NONE', #41451, 1000.000000000000000 ) ;
#21448 = DIRECTION ( 'NONE',  ( -0.000000000000000000, -0.3546048870425300148, 0.9350162426854169428 ) ) ;
#21449 = ORIENTED_EDGE ( 'NONE', *, *, #11248, .F. ) ;
#21450 = EDGE_CURVE ( 'NONE', #14876, #43567, #38503, .T. ) ;
#21451 = VECTOR ( 'NONE', #34145, 1000.000000000000000 ) ;
#21452 = CARTESIAN_POINT ( 'NONE',  ( -142.3192003680973130, -177.1207230881787780, 82.57748230379306165 ) ) ;
#21453 = CARTESIAN_POINT ( 'NONE',  ( -21.46839590530488451, -183.6283474603465606, 122.0467960216650738 ) ) ;
#21454 = FACE_OUTER_BOUND ( 'NONE', #15618, .T. ) ;
#21455 = ADVANCED_FACE ( 'NONE', ( #33776 ), #9871, .T. ) ;
#21456 = AXIS2_PLACEMENT_3D ( 'NONE', #37842, #10492, #1837 ) ;
#21457 = DIRECTION ( 'NONE',  ( 0.000000000000000000, 0.9709418174260519008, -0.2393156642875582940 ) ) ;
#21458 = ADVANCED_FACE ( 'NONE', ( #50085 ), #1977, .T. ) ;
#21460 = VECTOR ( 'NONE', #12166, 1000.000000000000000 ) ;
#21459 = CARTESIAN_POINT ( 'NONE',  ( -339.1964088526558498, -64.86990808808717190, -6.615309698015097162 ) ) ;
#21461 = CARTESIAN_POINT ( 'NONE',  ( -330.4913330509368166, -124.0000000000001990, -59.00000000000002132 ) ) ;
#21462 = ORIENTED_EDGE ( 'NONE', *, *, #35816, .T. ) ;
#21463 = EDGE_CURVE ( 'NONE', #51023, #44188, #13548, .T. ) ;
#21464 = DIRECTION ( 'NONE',  ( 1.043714542225393381E-14, 0.2393156642875449158, -0.9709418174260553425 ) ) ;
#21465 = VERTEX_POINT ( 'NONE', #18019 ) ;
#21466 = EDGE_CURVE ( 'NONE', #1126, #25732, #22731, .T. ) ;
#21467 = ORIENTED_EDGE ( 'NONE', *, *, #39598, .F. ) ;
#21468 = LINE ( 'NONE', #29599, #10359 ) ;
#21469 = EDGE_LOOP ( 'NONE', ( #5905, #22377, #2753, #5870 ) ) ;
#21470 = DIRECTION ( 'NONE',  ( 0.000000000000000000, 0.8229838658936516893, -0.5680647467311626952 ) ) ;
#21471 = VECTOR ( 'NONE', #45705, 1000.000000000000000 ) ;
#21472 = DIRECTION ( 'NONE',  ( 0.000000000000000000, 1.029269262412905585E-13, 1.000000000000000000 ) ) ;
#21474 = VERTEX_POINT ( 'NONE', #45878 ) ;
#21473 = DIRECTION ( 'NONE',  ( 0.000000000000000000, -1.000000000000000000, 0.000000000000000000 ) ) ;
#21475 = CIRCLE ( 'NONE', #46688, 125.0000000000000000 ) ;
#21476 = CARTESIAN_POINT ( 'NONE',  ( -48.47912675150885065, -183.6283474603465606, 6.938893903907228378E-15 ) ) ;
#21477 = EDGE_CURVE ( 'NONE', #41880, #26860, #45625, .T. ) ;
#21478 = EDGE_LOOP ( 'NONE', ( #18904, #19387, #34294, #7744 ) ) ;
#21479 = ORIENTED_EDGE ( 'NONE', *, *, #44471, .T. ) ;
#21480 = VERTEX_POINT ( 'NONE', #10127 ) ;
#21481 = FACE_BOUND ( 'NONE', #44839, .T. ) ;
#21482 = CARTESIAN_POINT ( 'NONE',  ( 34.93559171950835918, -193.5000000000000000, -93.09664195018497423 ) ) ;
#21483 = VERTEX_POINT ( 'NONE', #30596 ) ;
#21484 = AXIS2_PLACEMENT_3D ( 'NONE', #15553, #35253, #39694 ) ;
#21485 = DIRECTION ( 'NONE',  ( 0.000000000000000000, -1.000000000000000000, 0.000000000000000000 ) ) ;
#21486 = AXIS2_PLACEMENT_3D ( 'NONE', #15381, #48487, #43223 ) ;
#21487 = CARTESIAN_POINT ( 'NONE',  ( -95.18697522258266019, -193.5000000000000000, 115.9455772817713353 ) ) ;
#21488 = CARTESIAN_POINT ( 'NONE',  ( 73.66680038934278230, -193.5000000000000000, -26.55884942729568365 ) ) ;
#21489 = CIRCLE ( 'NONE', #48309, 125.0000000000000000 ) ;
#21490 = CARTESIAN_POINT ( 'NONE',  ( -339.1964088526558498, -71.49045607248255862, -27.86139516340906397 ) ) ;
#21491 = EDGE_CURVE ( 'NONE', #9298, #13843, #34543, .T. ) ;
#21492 = CARTESIAN_POINT ( 'NONE',  ( -336.3521761649654422, -93.75055682584159911, 51.01861988938794923 ) ) ;
#21493 = ORIENTED_EDGE ( 'NONE', *, *, #50436, .T. ) ;
#21495 = ORIENTED_EDGE ( 'NONE', *, *, #49419, .T. ) ;
#21494 = DIRECTION ( 'NONE',  ( 0.9995608365087946812, 0.000000000000000000, -0.02963332782254913048 ) ) ;
#21496 = VERTEX_POINT ( 'NONE', #26142 ) ;
#21497 = ORIENTED_EDGE ( 'NONE', *, *, #47933, .T. ) ;
#21498 = LINE ( 'NONE', #16598, #35845 ) ;
#21499 = CARTESIAN_POINT ( 'NONE',  ( -15.24927435600542047, -183.6283474603465606, 120.5021863277719092 ) ) ;
#21500 = ORIENTED_EDGE ( 'NONE', *, *, #1460, .F. ) ;
#21501 = EDGE_CURVE ( 'NONE', #25767, #39566, #38230, .T. ) ;
#21502 = PLANE ( 'NONE',  #15434 ) ;
#21503 = EDGE_CURVE ( 'NONE', #38453, #13810, #44303, .T. ) ;
#21504 = EDGE_CURVE ( 'NONE', #46459, #10671, #29829, .T. ) ;
#21505 = CARTESIAN_POINT ( 'NONE',  ( -330.4913330509368166, -84.08827740916061089, 45.24064679492014562 ) ) ;
#21506 = EDGE_LOOP ( 'NONE', ( #44300, #7525, #46685, #24467 ) ) ;
#21507 = DIRECTION ( 'NONE',  ( 0.3202698538628416247, 0.000000000000000000, -0.9473263538541900619 ) ) ;
#21508 = ORIENTED_EDGE ( 'NONE', *, *, #25349, .F. ) ;
#21509 = EDGE_CURVE ( 'NONE', #19400, #50173, #19127, .T. ) ;
#21510 = ORIENTED_EDGE ( 'NONE', *, *, #39485, .F. ) ;
#21511 = DIRECTION ( 'NONE',  ( 0.000000000000000000, -0.5680647467311457088, 0.8229838658936633466 ) ) ;
#21512 = VECTOR ( 'NONE', #29333, 1000.000000000000000 ) ;
#21513 = DIRECTION ( 'NONE',  ( -0.000000000000000000, 0.000000000000000000, 1.000000000000000000 ) ) ;
#21514 = AXIS2_PLACEMENT_3D ( 'NONE', #43031, #30673, #50667 ) ;
#21515 = DIRECTION ( 'NONE',  ( 0.000000000000000000, 1.000000000000000000, 0.000000000000000000 ) ) ;
#21516 = CARTESIAN_POINT ( 'NONE',  ( -332.3517673607765914, -148.5878911270064009, 53.46519113769075204 ) ) ;
#21517 = ORIENTED_EDGE ( 'NONE', *, *, #36402, .T. ) ;
#21518 = CIRCLE ( 'NONE', #50895, 125.0000000000000000 ) ;
#21519 = DIRECTION ( 'NONE',  ( -0.000000000000000000, 0.000000000000000000, -1.000000000000000000 ) ) ;
#21520 = CARTESIAN_POINT ( 'NONE',  ( -48.71401279728984690, -183.6283474603465606, 0.9720229140804159673 ) ) ;
#21521 = CIRCLE ( 'NONE', #32375, 125.0000000000000000 ) ;
#21522 = FACE_OUTER_BOUND ( 'NONE', #49776, .T. ) ;
#21523 = CARTESIAN_POINT ( 'NONE',  ( -330.4913330509368166, -122.9999999999994600, 59.99791663049642665 ) ) ;
#21524 = ADVANCED_FACE ( 'NONE', ( #6460 ), #21952, .T. ) ;
#21525 = VERTEX_POINT ( 'NONE', #42169 ) ;
#21526 = CARTESIAN_POINT ( 'NONE',  ( -164.2512865680372727, -189.7472609257535510, -47.13604789772048775 ) ) ;
#21527 = PLANE ( 'NONE',  #3004 ) ;
#21528 = CARTESIAN_POINT ( 'NONE',  ( -172.4728835572423975, -183.6283474603465606, 1.322128892812083123 ) ) ;
#21529 = ORIENTED_EDGE ( 'NONE', *, *, #12799, .F. ) ;
#21530 = CIRCLE ( 'NONE', #51033, 60.00000000000000000 ) ;
#21531 = ADVANCED_FACE ( 'NONE', ( #6193 ), #18283, .T. ) ;
#21532 = AXIS2_PLACEMENT_3D ( 'NONE', #41624, #29011, #1160 ) ;
#21533 = CIRCLE ( 'NONE', #36639, 125.0000000000000000 ) ;
#21534 = VECTOR ( 'NONE', #25202, 1000.000000000000000 ) ;
#21535 = DIRECTION ( 'NONE',  ( -0.000000000000000000, 1.000000000000000000, -0.000000000000000000 ) ) ;
#21536 = EDGE_CURVE ( 'NONE', #24293, #41262, #30347, .T. ) ;
#21537 = LINE ( 'NONE', #21793, #3595 ) ;
#21538 = ORIENTED_EDGE ( 'NONE', *, *, #41068, .T. ) ;
#21539 = ORIENTED_EDGE ( 'NONE', *, *, #16737, .T. ) ;
#21540 = VECTOR ( 'NONE', #43084, 1000.000000000000114 ) ;
#21541 = ORIENTED_EDGE ( 'NONE', *, *, #45914, .T. ) ;
#21542 = ADVANCED_FACE ( 'NONE', ( #18529 ), #38740, .F. ) ;
#21543 = AXIS2_PLACEMENT_3D ( 'NONE', #21104, #45808, #17701 ) ;
#21544 = CARTESIAN_POINT ( 'NONE',  ( 48.66843973345087448, 35.00000000000000000, -40.95752564483601788 ) ) ;
#21545 = AXIS2_PLACEMENT_3D ( 'NONE', #21822, #37837, #2363 ) ;
#21546 = DIRECTION ( 'NONE',  ( 0.000000000000000000, -0.1205366802553095168, 0.9927088740980556381 ) ) ;
#21547 = CARTESIAN_POINT ( 'NONE',  ( -48.47912675150885065, -175.3837268820161057, 6.938893903907228378E-15 ) ) ;
#21548 = CARTESIAN_POINT ( 'NONE',  ( -143.2689064740322067, -177.1207230881787780, -79.94433946042767047 ) ) ;
#21549 = CARTESIAN_POINT ( 'NONE',  ( -48.47912675150885065, -175.3837268820161057, 6.938893903907228378E-15 ) ) ;
#21550 = DIRECTION ( 'NONE',  ( -0.9720229140804139689, 0.000000000000000000, 0.2348860457809708036 ) ) ;
#21551 = ORIENTED_EDGE ( 'NONE', *, *, #30337, .F. ) ;
#21553 = EDGE_CURVE ( 'NONE', #48128, #51755, #43208, .T. ) ;
#21552 = DIRECTION ( 'NONE',  ( 0.000000000000000000, -0.000000000000000000, -1.000000000000000000 ) ) ;
#21554 = EDGE_LOOP ( 'NONE', ( #11748, #21479, #21408, #21467 ) ) ;
#21555 = DIRECTION ( 'NONE',  ( 0.000000000000000000, 0.000000000000000000, 1.000000000000000000 ) ) ;
#21556 = VECTOR ( 'NONE', #11872, 1000.000000000000114 ) ;
#21557 = EDGE_LOOP ( 'NONE', ( #18457, #15377, #29373, #49636 ) ) ;
#21558 = CARTESIAN_POINT ( 'NONE',  ( -49.30901192927172616, -175.3837268820161057, -123.9972451320097093 ) ) ;
#21559 = VECTOR ( 'NONE', #49186, 1000.000000000000114 ) ;
#21560 = ORIENTED_EDGE ( 'NONE', *, *, #34404, .T. ) ;
#21561 =( NAMED_UNIT ( * ) SI_UNIT ( $, .STERADIAN. ) SOLID_ANGLE_UNIT ( ) );
#21562 = DIRECTION ( 'NONE',  ( 0.000000000000000000, 0.000000000000000000, 1.000000000000000000 ) ) ;
#21563 = ORIENTED_EDGE ( 'NONE', *, *, #36950, .T. ) ;
#21566 = ORIENTED_EDGE ( 'NONE', *, *, #48018, .F. ) ;
#21565 = DIRECTION ( 'NONE',  ( 0.000000000000000000, 0.5680647467311626952, 0.8229838658936516893 ) ) ;
#21564 = DIRECTION ( 'NONE',  ( 0.000000000000000000, -1.000000000000000000, 0.000000000000000000 ) ) ;
#21567 = VECTOR ( 'NONE', #39815, 999.9999999999998863 ) ;
#21568 = CIRCLE ( 'NONE', #45059, 10.99999999999999645 ) ;
#21569 = AXIS2_PLACEMENT_3D ( 'NONE', #21891, #49506, #10063 ) ;
#21570 = CARTESIAN_POINT ( 'NONE',  ( -156.7610986364826999, -193.5000000000000000, -62.45009659481510766 ) ) ;
#21572 = ORIENTED_EDGE ( 'NONE', *, *, #31926, .F. ) ;
#21571 = AXIS2_PLACEMENT_3D ( 'NONE', #7925, #39973, #23202 ) ;
#21573 = CARTESIAN_POINT ( 'NONE',  ( -164.6246685127424882, -189.7472609257535510, -46.20836643930982035 ) ) ;
#21574 = VERTEX_POINT ( 'NONE', #15120 ) ;
#21575 = ADVANCED_FACE ( 'NONE', ( #47172 ), #26921, .F. ) ;
#21576 = EDGE_CURVE ( 'NONE', #24073, #22978, #3784, .T. ) ;
#21577 = AXIS2_PLACEMENT_3D ( 'NONE', #44552, #1444, #25360 ) ;
#21578 = LINE ( 'NONE', #1328, #14113 ) ;
#21581 = ORIENTED_EDGE ( 'NONE', *, *, #19689, .F. ) ;
#21580 = FACE_OUTER_BOUND ( 'NONE', #50458, .T. ) ;
#21579 = CARTESIAN_POINT ( 'NONE',  ( -96.30460367372253927, -193.5000000000000000, -114.4068333132746176 ) ) ;
#21582 = VERTEX_POINT ( 'NONE', #19808 ) ;
#21583 = AXIS2_PLACEMENT_3D ( 'NONE', #13942, #37846, #6059 ) ;
#21584 = LINE ( 'NONE', #41525, #24864 ) ;
#21585 = CARTESIAN_POINT ( 'NONE',  ( -12.13476221271688615, -193.5000000000000000, 119.5996955107804638 ) ) ;
#21586 = LINE ( 'NONE', #1611, #22326 ) ;
#21587 = ORIENTED_EDGE ( 'NONE', *, *, #42140, .T. ) ;
#21588 = CARTESIAN_POINT ( 'NONE',  ( -339.1964088526558498, -123.5000000000000284, 0.000000000000000000 ) ) ;
#21589 = DIRECTION ( 'NONE',  ( -0.000000000000000000, 1.000000000000000000, 0.000000000000000000 ) ) ;
#21590 = DIRECTION ( 'NONE',  ( -1.000000000000000000, 0.000000000000000000, 0.000000000000000000 ) ) ;
#21591 = ORIENTED_EDGE ( 'NONE', *, *, #537, .T. ) ;
#21592 = LINE ( 'NONE', #1345, #50628 ) ;
#21593 = CARTESIAN_POINT ( 'NONE',  ( -122.3978016498073202, -183.6283474603465606, -100.8019320314827212 ) ) ;
#21594 = DIRECTION ( 'NONE',  ( -0.1182731709213523247, 0.000000000000000000, -0.9929810960135185827 ) ) ;
#21595 = ORIENTED_EDGE ( 'NONE', *, *, #23977, .T. ) ;
#21596 = VECTOR ( 'NONE', #13164, 1000.000000000000114 ) ;
#21597 = AXIS2_PLACEMENT_3D ( 'NONE', #37089, #49198, #43106 ) ;
#21598 = DIRECTION ( 'NONE',  ( 1.000000000000000000, -0.000000000000000000, -0.000000000000000000 ) ) ;
#21599 = DIRECTION ( 'NONE',  ( -0.000000000000000000, 1.000000000000000000, -0.000000000000000000 ) ) ;
#21600 = EDGE_CURVE ( 'NONE', #27297, #47014, #11401, .T. ) ;
#21601 = AXIS2_PLACEMENT_3D ( 'NONE', #38468, #14047, #2976 ) ;
#21602 = DIRECTION ( 'NONE',  ( -0.4031234292879600778, 0.000000000000000000, -0.9151456172430237901 ) ) ;
#21603 = DIRECTION ( 'NONE',  ( 0.000000000000000000, 0.000000000000000000, 1.000000000000000000 ) ) ;
#21604 = EDGE_CURVE ( 'NONE', #45638, #38775, #22989, .T. ) ;
#21605 = CARTESIAN_POINT ( 'NONE',  ( -339.1964088526558498, -162.2499814621216672, -44.49369547121515467 ) ) ;
#21606 = AXIS2_PLACEMENT_3D ( 'NONE', #38727, #18770, #26392 ) ;
#21607 = AXIS2_PLACEMENT_3D ( 'NONE', #42938, #12427, #48705 ) ;
#21608 = CARTESIAN_POINT ( 'NONE',  ( -339.1964088526558498, -64.86990808808717190, -6.615309698015097162 ) ) ;
#21609 = DIRECTION ( 'NONE',  ( 0.000000000000000000, 1.000000000000000000, 0.000000000000000000 ) ) ;
#21611 = ORIENTED_EDGE ( 'NONE', *, *, #23419, .T. ) ;
#21610 = DIRECTION ( 'NONE',  ( -1.000000000000000000, 9.241633304753506654E-15, -4.850383327712056395E-15 ) ) ;
#21612 = AXIS2_PLACEMENT_3D ( 'NONE', #18346, #34362, #30157 ) ;
#21613 = EDGE_LOOP ( 'NONE', ( #44530, #10354 ) ) ;
#21614 = DIRECTION ( 'NONE',  ( -0.000000000000000000, 1.000000000000000000, 0.000000000000000000 ) ) ;
#21615 = VECTOR ( 'NONE', #32346, 1000.000000000000000 ) ;
#21616 = VECTOR ( 'NONE', #16536, 1000.000000000000000 ) ;
#21618 = VERTEX_POINT ( 'NONE', #15893 ) ;
#21617 = DIRECTION ( 'NONE',  ( -0.000000000000000000, 1.000000000000000000, -0.000000000000000000 ) ) ;
#21619 = EDGE_LOOP ( 'NONE', ( #3307, #41768, #37014, #7341 ) ) ;
#21620 = ORIENTED_EDGE ( 'NONE', *, *, #46384, .T. ) ;
#21621 = CARTESIAN_POINT ( 'NONE',  ( -26.53529504715431031, -175.3837268820161057, 123.0587999703026725 ) ) ;
#21622 = DIRECTION ( 'NONE',  ( -0.6300878435817094392, 0.000000000000000000, -0.7765238627180437447 ) ) ;
#21623 = CARTESIAN_POINT ( 'NONE',  ( -89.73513343757494454, -193.5000000000000000, -117.9955164924467397 ) ) ;
#21624 = ORIENTED_EDGE ( 'NONE', *, *, #30977, .T. ) ;
#21625 = APPLICATION_CONTEXT ( 'automotive_design' ) ;
#21626 = DIRECTION ( 'NONE',  ( -0.000000000000000000, 1.000000000000000000, -0.000000000000000000 ) ) ;
#21627 = AXIS2_PLACEMENT_3D ( 'NONE', #10640, #31376, #11399 ) ;
#21629 = ORIENTED_EDGE ( 'NONE', *, *, #43369, .F. ) ;
#21628 = FACE_OUTER_BOUND ( 'NONE', #45314, .T. ) ;
#21630 = AXIS2_PLACEMENT_3D ( 'NONE', #30228, #2096, #26269 ) ;
#21631 = CYLINDRICAL_SURFACE ( 'NONE', #37354, 125.0000000000000000 ) ;
#21632 = ORIENTED_EDGE ( 'NONE', *, *, #28169, .T. ) ;
#21633 = CARTESIAN_POINT ( 'NONE',  ( -305.0000000000000568, -123.5000000000000284, 0.000000000000000000 ) ) ;
#21634 = VECTOR ( 'NONE', #21282, 1000.000000000000000 ) ;
#21635 = EDGE_LOOP ( 'NONE', ( #12802, #13358, #10052, #34232 ) ) ;
#21636 = EDGE_CURVE ( 'NONE', #2495, #29872, #21530, .T. ) ;
#21637 = LINE ( 'NONE', #2163, #10643 ) ;
#21638 = CARTESIAN_POINT ( 'NONE',  ( -123.6678354051270077, -193.5000000000000000, 99.85818990449067201 ) ) ;
#21639 = DIRECTION ( 'NONE',  ( -0.000000000000000000, -0.1205366802553268363, -0.9927088740980534176 ) ) ;
#21640 = ORIENTED_EDGE ( 'NONE', *, *, #25312, .F. ) ;
#21641 = CIRCLE ( 'NONE', #51027, 4.999999999999997335 ) ;
#21642 = ORIENTED_EDGE ( 'NONE', *, *, #18982, .F. ) ;
#21643 = DIRECTION ( 'NONE',  ( 0.3758275821142422202, 0.000000000000000000, -0.9266896074318318188 ) ) ;
#21644 = CARTESIAN_POINT ( 'NONE',  ( -305.0000000000000568, -100.7053649598255163, 55.50139289590170222 ) ) ;
#21645 = EDGE_LOOP ( 'NONE', ( #40581, #24722, #3828, #47625 ) ) ;
#21646 = DIRECTION ( 'NONE',  ( 0.000000000000000000, 1.000000000000000000, 0.000000000000000000 ) ) ;
#21647 = AXIS2_PLACEMENT_3D ( 'NONE', #42433, #42709, #21706 ) ;
#21648 = ORIENTED_EDGE ( 'NONE', *, *, #21832, .T. ) ;
#21649 = CARTESIAN_POINT ( 'NONE',  ( -110.8210171970983140, -193.5000000000000000, 107.1890582354659074 ) ) ;
#21650 = FACE_OUTER_BOUND ( 'NONE', #45905, .T. ) ;
#21651 = CIRCLE ( 'NONE', #35070, 125.0000000000000000 ) ;
#21652 = ORIENTED_EDGE ( 'NONE', *, *, #51528, .T. ) ;
#21653 = DIRECTION ( 'NONE',  ( -0.000000000000000000, 1.000000000000000000, -0.000000000000000000 ) ) ;
#21654 = VERTEX_POINT ( 'NONE', #11920 ) ;
#21655 = CARTESIAN_POINT ( 'NONE',  ( -82.67254833784559764, -183.6283474603465606, -120.2323164553483963 ) ) ;
#21656 = DIRECTION ( 'NONE',  ( -0.000000000000000000, 1.000000000000000000, -0.000000000000000000 ) ) ;
#21657 = DIRECTION ( 'NONE',  ( 0.000000000000000000, 1.535808517398133130E-13, 1.000000000000000000 ) ) ;
#21658 = ADVANCED_FACE ( 'NONE', ( #39519 ), #31901, .T. ) ;
#21659 = ORIENTED_EDGE ( 'NONE', *, *, #17667, .F. ) ;
#21660 = EDGE_CURVE ( 'NONE', #42791, #20194, #15626, .T. ) ;
#21661 = DIRECTION ( 'NONE',  ( 0.000000000000000000, 0.000000000000000000, 1.000000000000000000 ) ) ;
#21662 = PLANE ( 'NONE',  #44853 ) ;
#21663 = DIRECTION ( 'NONE',  ( -1.000000000000000000, 0.000000000000000000, 0.000000000000000000 ) ) ;
#21664 = DIRECTION ( 'NONE',  ( 0.000000000000000000, -1.082467449009527627E-13, 1.000000000000000000 ) ) ;
#21665 = VERTEX_POINT ( 'NONE', #46925 ) ;
#21666 = DIRECTION ( 'NONE',  ( -0.000000000000000000, 1.000000000000000000, -0.000000000000000000 ) ) ;
#21667 = VERTEX_POINT ( 'NONE', #24017 ) ;
#21668 = VECTOR ( 'NONE', #12247, 1000.000000000000000 ) ;
#21669 = CARTESIAN_POINT ( 'NONE',  ( -339.1964088526558498, -157.4273119900853146, -48.27201571435997352 ) ) ;
#21671 = ORIENTED_EDGE ( 'NONE', *, *, #26631, .T. ) ;
#21670 = LINE ( 'NONE', #2468, #48017 ) ;
#21672 = AXIS2_PLACEMENT_3D ( 'NONE', #28175, #35548, #325 ) ;
#21673 = ORIENTED_EDGE ( 'NONE', *, *, #46092, .T. ) ;
#21674 = LINE ( 'NONE', #8787, #40782 ) ;
#21675 = CARTESIAN_POINT ( 'NONE',  ( -330.4913330509368166, -130.1153096980145563, 58.63009191191294178 ) ) ;
#21676 = AXIS2_PLACEMENT_3D ( 'NONE', #48174, #51870, #47914 ) ;
#21677 = ORIENTED_EDGE ( 'NONE', *, *, #29077, .T. ) ;
#21678 = DIRECTION ( 'NONE',  ( -0.9374196611341254481, 0.000000000000000000, 0.3482016354343867026 ) ) ;
#21679 = ORIENTED_EDGE ( 'NONE', *, *, #6019, .F. ) ;
#21680 = FACE_OUTER_BOUND ( 'NONE', #29747, .T. ) ;
#21681 = DIRECTION ( 'NONE',  ( -0.9027978299657477557, 0.000000000000000000, 0.4300652022765115712 ) ) ;
#21682 = ADVANCED_FACE ( 'NONE', ( #47941 ), #35326, .F. ) ;
#21683 = DIRECTION ( 'NONE',  ( -1.000000000000000000, 0.000000000000000000, -0.000000000000000000 ) ) ;
#21684 = DIRECTION ( 'NONE',  ( 1.000000000000000000, 0.000000000000000000, 0.000000000000000000 ) ) ;
#21685 = EDGE_LOOP ( 'NONE', ( #25548, #43727, #15075, #2058 ) ) ;
#21686 = ORIENTED_EDGE ( 'NONE', *, *, #3831, .F. ) ;
#21687 = EDGE_LOOP ( 'NONE', ( #2567, #883, #8661, #41852 ) ) ;
#21688 = AXIS2_PLACEMENT_3D ( 'NONE', #37008, #1003, #17059 ) ;
#21689 = EDGE_CURVE ( 'NONE', #36746, #41934, #48377, .T. ) ;
#21690 = CARTESIAN_POINT ( 'NONE',  ( -305.0000000000000568, -139.4384828369889249, -57.84431488793872944 ) ) ;
#21691 = CARTESIAN_POINT ( 'NONE',  ( -339.1964088526558498, -84.75001853787809125, 44.49369547121489887 ) ) ;
#21692 = CARTESIAN_POINT ( 'NONE',  ( -365.0000000000001137, -168.5000000000000284, -10.00000000000000711 ) ) ;
#21693 = DIRECTION ( 'NONE',  ( -0.000000000000000000, 1.000000000000000000, 0.000000000000000000 ) ) ;
#21694 = EDGE_LOOP ( 'NONE', ( #46447, #3738, #36168, #22025 ) ) ;
#21695 = UNCERTAINTY_MEASURE_WITH_UNIT (LENGTH_MEASURE( 1.000000000000000082E-05 ), #7587, 'distance_accuracy_value', 'NONE');
#21696 = EDGE_CURVE ( 'NONE', #25065, #28841, #30864, .T. ) ;
#21697 = EDGE_CURVE ( 'NONE', #45030, #11192, #43731, .T. ) ;
#21698 = ORIENTED_EDGE ( 'NONE', *, *, #24333, .F. ) ;
#21700 = ORIENTED_EDGE ( 'NONE', *, *, #45218, .F. ) ;
#21699 = CARTESIAN_POINT ( 'NONE',  ( -48.47912675150885065, -183.6283474603465606, 6.938893903907228378E-15 ) ) ;
#21701 = ORIENTED_EDGE ( 'NONE', *, *, #31999, .T. ) ;
#21702 = AXIS2_PLACEMENT_3D ( 'NONE', #22932, #50797, #14278 ) ;
#21703 = EDGE_CURVE ( 'NONE', #7739, #30234, #41786, .T. ) ;
#21705 = AXIS2_PLACEMENT_3D ( 'NONE', #47540, #19662, #24389 ) ;
#21704 = DIRECTION ( 'NONE',  ( 0.000000000000000000, 1.000000000000000000, -0.000000000000000000 ) ) ;
#21706 = DIRECTION ( 'NONE',  ( 0.000000000000000000, 0.000000000000000000, 1.000000000000000000 ) ) ;
#21707 = AXIS2_PLACEMENT_3D ( 'NONE', #27085, #14507, #50260 ) ;
#21708 = CARTESIAN_POINT ( 'NONE',  ( 19.33815737959698566, -177.1207230881787780, 105.0038855142078091 ) ) ;
#21709 = FACE_OUTER_BOUND ( 'NONE', #30662, .T. ) ;
#21710 = ORIENTED_EDGE ( 'NONE', *, *, #19774, .T. ) ;
#21711 = CARTESIAN_POINT ( 'NONE',  ( -339.1964088526558498, -66.33409060400650503, 14.60509510167813474 ) ) ;
#21712 = EDGE_LOOP ( 'NONE', ( #48221, #25139, #18968, #48989 ) ) ;
#21713 = ORIENTED_EDGE ( 'NONE', *, *, #6738, .F. ) ;
#21714 = CARTESIAN_POINT ( 'NONE',  ( -47.66663987350317200, -193.5000000000000000, -0.5829794791144634614 ) ) ;
#21715 = VECTOR ( 'NONE', #14908, 1000.000000000000000 ) ;
#21716 = DIRECTION ( 'NONE',  ( -1.000000000000000000, 0.000000000000000000, -0.000000000000000000 ) ) ;
#21717 = VERTEX_POINT ( 'NONE', #7487 ) ;
#21718 = LINE ( 'NONE', #37736, #40751 ) ;
#21719 = DIRECTION ( 'NONE',  ( 0.8124868780056742068, 0.000000000000000000, 0.5829794791144820021 ) ) ;
#21720 = DIRECTION ( 'NONE',  ( 0.7575112421616236880, 0.000000000000000000, -0.6528221181905174975 ) ) ;
#21721 = DIRECTION ( 'NONE',  ( 0.000000000000000000, -1.000000000000000000, 0.000000000000000000 ) ) ;
#21722 = VECTOR ( 'NONE', #2037, 1000.000000000000114 ) ;
#21723 = FACE_OUTER_BOUND ( 'NONE', #44660, .T. ) ;
#21724 = LINE ( 'NONE', #13318, #12280 ) ;
#21725 = ORIENTED_EDGE ( 'NONE', *, *, #28783, .F. ) ;
#21726 = LINE ( 'NONE', #10144, #12197 ) ;
#21727 = ORIENTED_EDGE ( 'NONE', *, *, #20800, .F. ) ;
#21728 = ORIENTED_EDGE ( 'NONE', *, *, #43566, .T. ) ;
#21729 = DIRECTION ( 'NONE',  ( 0.9374196611341183427, 0.000000000000000000, 0.3482016354344059095 ) ) ;
#21730 = EDGE_LOOP ( 'NONE', ( #18781, #18716, #6761, #21296 ) ) ;
#21731 = DIRECTION ( 'NONE',  ( -0.000000000000000000, 1.000000000000000000, -0.000000000000000000 ) ) ;
#21732 = VECTOR ( 'NONE', #11619, 1000.000000000000000 ) ;
#21733 = VECTOR ( 'NONE', #37568, 1000.000000000000000 ) ;
#21734 = PLANE ( 'NONE',  #1608 ) ;
#21736 = ORIENTED_EDGE ( 'NONE', *, *, #10218, .F. ) ;
#21735 = DIRECTION ( 'NONE',  ( 0.000000000000000000, 0.000000000000000000, 1.000000000000000000 ) ) ;
#21737 = CIRCLE ( 'NONE', #32643, 124.9999999999999858 ) ;
#21738 = EDGE_CURVE ( 'NONE', #8223, #38711, #38999, .T. ) ;
#21739 = EDGE_CURVE ( 'NONE', #6345, #43598, #47694, .T. ) ;
#21740 = DIRECTION ( 'NONE',  ( 0.000000000000000000, 0.000000000000000000, -1.000000000000000000 ) ) ;
#21741 = ORIENTED_EDGE ( 'NONE', *, *, #46082, .T. ) ;
#21742 = VERTEX_POINT ( 'NONE', #11674 ) ;
#21743 = ORIENTED_EDGE ( 'NONE', *, *, #27236, .T. ) ;
#21744 = CARTESIAN_POINT ( 'NONE',  ( -48.93575598890257794, -175.3837268820161057, 0.8896570909947506545 ) ) ;
#21745 = VECTOR ( 'NONE', #25925, 1000.000000000000000 ) ;
#21746 = DIRECTION ( 'NONE',  ( -0.7765238627180349740, 0.000000000000000000, -0.6300878435817203194 ) ) ;
#21747 = CARTESIAN_POINT ( 'NONE',  ( -339.1964088526558498, -116.8846903019842927, 58.63009191191280678 ) ) ;
#21748 = ADVANCED_FACE ( 'NONE', ( #35075 ), #7734, .F. ) ;
#21749 = DIRECTION ( 'NONE',  ( 0.9995608365087942371, 0.000000000000000000, 0.02963332782256331357 ) ) ;
#21750 = FACE_OUTER_BOUND ( 'NONE', #45108, .T. ) ;
#21751 = ORIENTED_EDGE ( 'NONE', *, *, #24518, .T. ) ;
#21752 = ADVANCED_FACE ( 'NONE', ( #4307 ), #36101, .T. ) ;
#21753 = EDGE_CURVE ( 'NONE', #13544, #17366, #28208, .T. ) ;
#21754 = AXIS2_PLACEMENT_3D ( 'NONE', #50230, #13954, #2389 ) ;
#21755 = CARTESIAN_POINT ( 'NONE',  ( -332.3517673607765914, -111.9361751271348879, -57.91551518289410438 ) ) ;
#21756 = DIRECTION ( 'NONE',  ( 0.000000000000000000, 0.000000000000000000, 1.000000000000000000 ) ) ;
#21757 = VERTEX_POINT ( 'NONE', #16676 ) ;
#21759 = ORIENTED_EDGE ( 'NONE', *, *, #38703, .T. ) ;
#21758 = CARTESIAN_POINT ( 'NONE',  ( -48.47912675150885065, -183.6283474603465606, 6.938893903907228378E-15 ) ) ;
#21760 = ORIENTED_EDGE ( 'NONE', *, *, #50429, .F. ) ;
#21761 = EDGE_CURVE ( 'NONE', #51645, #35821, #40548, .T. ) ;
#21762 = ORIENTED_EDGE ( 'NONE', *, *, #16978, .T. ) ;
#21763 = DIRECTION ( 'NONE',  ( -0.000000000000000000, 1.000000000000000000, 0.000000000000000000 ) ) ;
#21764 = CARTESIAN_POINT ( 'NONE',  ( 56.13126667599141939, 28.00000000000000355, -29.70424671247935677 ) ) ;
#21765 = ORIENTED_EDGE ( 'NONE', *, *, #19211, .F. ) ;
#21766 = EDGE_CURVE ( 'NONE', #29802, #12404, #41651, .T. ) ;
#21767 = CARTESIAN_POINT ( 'NONE',  ( 21.49274850782854074, -193.5000000000000000, -103.5805805771126700 ) ) ;
#21768 = DIRECTION ( 'NONE',  ( -0.000000000000000000, 1.000000000000000000, -0.000000000000000000 ) ) ;
#21769 = ORIENTED_EDGE ( 'NONE', *, *, #37150, .T. ) ;
#21770 = DIRECTION ( 'NONE',  ( 0.000000000000000000, 0.000000000000000000, 1.000000000000000000 ) ) ;
#21771 = ORIENTED_EDGE ( 'NONE', *, *, #16071, .T. ) ;
#21772 = ORIENTED_EDGE ( 'NONE', *, *, #46229, .T. ) ;
#21773 = CARTESIAN_POINT ( 'NONE',  ( -48.47912675150885065, -177.1207230881787780, 6.938893903907228378E-15 ) ) ;
#21774 = CARTESIAN_POINT ( 'NONE',  ( 0.000000000000000000, -63.50000000000000000, 0.000000000000000000 ) ) ;
#21775 = VECTOR ( 'NONE', #5193, 1000.000000000000227 ) ;
#21776 = DIRECTION ( 'NONE',  ( 0.000000000000000000, 0.000000000000000000, 1.000000000000000000 ) ) ;
#21777 = DIRECTION ( 'NONE',  ( 0.000000000000000000, -0.3546048870425267951, 0.9350162426854181641 ) ) ;
#21778 = EDGE_LOOP ( 'NONE', ( #44224, #38876, #33477, #12078 ) ) ;
#21779 = DIRECTION ( 'NONE',  ( 0.9890401873221654760, 0.000000000000000000, -0.1476465640024710868 ) ) ;
#21780 = AXIS2_PLACEMENT_3D ( 'NONE', #23807, #23309, #3322 ) ;
#21781 = DIRECTION ( 'NONE',  ( -0.000000000000000000, 1.000000000000000000, -0.000000000000000000 ) ) ;
#21782 = DIRECTION ( 'NONE',  ( 0.5085311186492216251, 0.000000000000000000, -0.8610436117673548884 ) ) ;
#21783 = CARTESIAN_POINT ( 'NONE',  ( -305.0000000000000568, -73.83865025250295844, 33.67120938215276738 ) ) ;
#21784 = ORIENTED_EDGE ( 'NONE', *, *, #20873, .T. ) ;
#21785 = FACE_OUTER_BOUND ( 'NONE', #38620, .T. ) ;
#21786 = DIRECTION ( 'NONE',  ( -0.000000000000000000, 1.000000000000000000, -0.000000000000000000 ) ) ;
#21787 = DIRECTION ( 'NONE',  ( -0.000000000000000000, -1.000000000000000000, 0.000000000000000000 ) ) ;
#21788 = ORIENTED_EDGE ( 'NONE', *, *, #1448, .F. ) ;
#21789 = EDGE_CURVE ( 'NONE', #1606, #1505, #17342, .T. ) ;
#21790 = VERTEX_POINT ( 'NONE', #876 ) ;
#21791 = CARTESIAN_POINT ( 'NONE',  ( -49.08592689732745384, -193.5000000000000000, 0.7948544414133550395 ) ) ;
#21792 = DIRECTION ( 'NONE',  ( -0.8455960035018311727, 0.000000000000000000, 0.5338233779647826305 ) ) ;
#21793 = CARTESIAN_POINT ( 'NONE',  ( -173.4460699164830260, -189.7472609257535510, -2.874563619423202265 ) ) ;
#21794 = ORIENTED_EDGE ( 'NONE', *, *, #13771, .F. ) ;
#21795 = LINE ( 'NONE', #33363, #12828 ) ;
#21796 = ORIENTED_EDGE ( 'NONE', *, *, #27189, .F. ) ;
#21797 = AXIS2_PLACEMENT_3D ( 'NONE', #21161, #41386, #49025 ) ;
#21798 = ADVANCED_FACE ( 'NONE', ( #13238 ), #48978, .F. ) ;
#21799 = CARTESIAN_POINT ( 'NONE',  ( -126.8597349762179931, -193.5000000000000000, -96.08646119223955395 ) ) ;
#21800 = FACE_OUTER_BOUND ( 'NONE', #33500, .T. ) ;
#21801 = CARTESIAN_POINT ( 'NONE',  ( 29.40217425202905588, -193.5000000000000000, -96.49160960477044569 ) ) ;
#21802 = EDGE_CURVE ( 'NONE', #40321, #50633, #34933, .T. ) ;
#21803 = EDGE_CURVE ( 'NONE', #41454, #5269, #97, .T. ) ;
#21804 = ADVANCED_FACE ( 'NONE', ( #36359 ), #44510, .T. ) ;
#21805 = CARTESIAN_POINT ( 'NONE',  ( -129.4514457347087557, -189.7472609257535510, 95.22858582633116953 ) ) ;
#21806 = ADVANCED_FACE ( 'NONE', ( #36623 ), #20867, .F. ) ;
#21807 = FACE_OUTER_BOUND ( 'NONE', #2941, .T. ) ;
#21808 = ORIENTED_EDGE ( 'NONE', *, *, #490, .T. ) ;
#21809 = EDGE_CURVE ( 'NONE', #42763, #14211, #48471, .T. ) ;
#21810 = CARTESIAN_POINT ( 'NONE',  ( -180.0000000000000568, -115.7896721143442278, 18.45401972188388839 ) ) ;
#21811 = ORIENTED_EDGE ( 'NONE', *, *, #27902, .F. ) ;
#21812 = CARTESIAN_POINT ( 'NONE',  ( 32.59960422616972409, -175.3837268820161057, -93.82025162277999186 ) ) ;
#21813 = VECTOR ( 'NONE', #8020, 1000.000000000000000 ) ;
#21814 = EDGE_LOOP ( 'NONE', ( #1749, #48245, #22319, #7781 ) ) ;
#21815 = EDGE_CURVE ( 'NONE', #41523, #44900, #28721, .T. ) ;
#21816 = CARTESIAN_POINT ( 'NONE',  ( -145.4373324222574126, -193.5000000000000000, -78.89300572996837957 ) ) ;
#21817 = VERTEX_POINT ( 'NONE', #44776 ) ;
#21818 = ADVANCED_FACE ( 'NONE', ( #33196 ), #32157, .T. ) ;
#21819 = EDGE_CURVE ( 'NONE', #19493, #25155, #8759, .T. ) ;
#21820 = CARTESIAN_POINT ( 'NONE',  ( -330.4913330509368166, -109.8658467157464571, 57.40522506028071348 ) ) ;
#21821 = PRODUCT_DEFINITION_SHAPE ( 'NONE', 'NONE',  #25740 ) ;
#21822 = CARTESIAN_POINT ( 'NONE',  ( -48.47912675150885065, -177.1207230881787780, 6.938893903907228378E-15 ) ) ;
#21823 = ORIENTED_EDGE ( 'NONE', *, *, #5448, .F. ) ;
#21826 = ORIENTED_EDGE ( 'NONE', *, *, #15331, .T. ) ;
#21825 = FACE_OUTER_BOUND ( 'NONE', #15209, .T. ) ;
#21824 = LINE ( 'NONE', #40998, #40089 ) ;
#21827 = EDGE_CURVE ( 'NONE', #27512, #32747, #37456, .T. ) ;
#21828 = FACE_OUTER_BOUND ( 'NONE', #41723, .T. ) ;
#21829 = ORIENTED_EDGE ( 'NONE', *, *, #44486, .T. ) ;
#21830 = CARTESIAN_POINT ( 'NONE',  ( -336.3521761649654422, -64.61288906875131488, 4.498567634385603142 ) ) ;
#21831 = ORIENTED_EDGE ( 'NONE', *, *, #4123, .F. ) ;
#21832 = EDGE_CURVE ( 'NONE', #2077, #42496, #47565, .T. ) ;
#21833 = CARTESIAN_POINT ( 'NONE',  ( -336.3521761649654422, -65.82380048139334860, 12.53476669029061519 ) ) ;
#21836 = VERTEX_POINT ( 'NONE', #28464 ) ;
#21835 = DIRECTION ( 'NONE',  ( 0.000000000000000000, 0.000000000000000000, 1.000000000000000000 ) ) ;
#21834 = DIRECTION ( 'NONE',  ( -0.000000000000000000, -0.8854560256532110207, -0.4647231720437664526 ) ) ;
#21837 = ORIENTED_EDGE ( 'NONE', *, *, #47808, .T. ) ;
#21838 = EDGE_CURVE ( 'NONE', #3688, #2653, #16497, .T. ) ;
#21839 = VECTOR ( 'NONE', #48704, 1000.000000000000000 ) ;
#21840 = VECTOR ( 'NONE', #24555, 1000.000000000000000 ) ;
#21841 = DIRECTION ( 'NONE',  ( -0.8124868780056863082, 0.000000000000000000, 0.5829794791144649047 ) ) ;
#21842 = DIRECTION ( 'NONE',  ( 0.000000000000000000, 0.000000000000000000, 1.000000000000000000 ) ) ;
#21843 = DIRECTION ( 'NONE',  ( -0.000000000000000000, 1.000000000000000000, -0.000000000000000000 ) ) ;
#21844 = ORIENTED_EDGE ( 'NONE', *, *, #10555, .T. ) ;
#21845 = CARTESIAN_POINT ( 'NONE',  ( -47.70260288879081401, -193.5000000000000000, 0.6300878435817218737 ) ) ;
#21846 = DIRECTION ( 'NONE',  ( 0.000000000000000000, 0.000000000000000000, -1.000000000000000000 ) ) ;
#21847 = DIRECTION ( 'NONE',  ( 0.000000000000000000, 0.000000000000000000, 1.000000000000000000 ) ) ;
#21848 = CARTESIAN_POINT ( 'NONE',  ( -48.18706998087188254, -193.5000000000000000, 0.9564009842765313074 ) ) ;
#21849 = ORIENTED_EDGE ( 'NONE', *, *, #40946, .F. ) ;
#21850 = LINE ( 'NONE', #37861, #35524 ) ;
#21851 = ADVANCED_FACE ( 'NONE', ( #22153 ), #25837, .T. ) ;
#21852 = DIRECTION ( 'NONE',  ( -0.6528221181905280446, 0.000000000000000000, 0.7575112421616145841 ) ) ;
#21853 = EDGE_CURVE ( 'NONE', #3589, #32593, #49763, .T. ) ;
#21854 = CARTESIAN_POINT ( 'NONE',  ( -47.63353074800702558, -183.6283474603465606, -0.5338233779647817423 ) ) ;
#21855 = VERTEX_POINT ( 'NONE', #41592 ) ;
#21856 = VECTOR ( 'NONE', #34645, 1000.000000000000000 ) ;
#21857 = CARTESIAN_POINT ( 'NONE',  ( -305.0000000000000568, -63.87926739338334414, -6.735595255826709149 ) ) ;
#21858 = LINE ( 'NONE', #21328, #915 ) ;
#21859 = LINE ( 'NONE', #22108, #6753 ) ;
#21860 = DIRECTION ( 'NONE',  ( -0.000000000000000000, 1.000000000000000000, 0.000000000000000000 ) ) ;
#21861 = LINE ( 'NONE', #13452, #6982 ) ;
#21862 = CARTESIAN_POINT ( 'NONE',  ( -101.5170032742336446, -177.1207230881787780, 112.0852863853383212 ) ) ;
#21863 = CARTESIAN_POINT ( 'NONE',  ( -305.0000000000000568, -175.3529239922484351, 30.18731974611377211 ) ) ;
#21865 = ORIENTED_EDGE ( 'NONE', *, *, #29796, .F. ) ;
#21864 = CARTESIAN_POINT ( 'NONE',  ( -59.16959496120700379, -177.1207230881787780, 123.5388265266452237 ) ) ;
#21866 = ORIENTED_EDGE ( 'NONE', *, *, #35795, .T. ) ;
#21867 = EDGE_CURVE ( 'NONE', #36669, #39834, #45815, .T. ) ;
#21868 = ADVANCED_FACE ( 'NONE', ( #50284 ), #46088, .F. ) ;
#21869 = VECTOR ( 'NONE', #33699, 1000.000000000000000 ) ;
#21870 = EDGE_CURVE ( 'NONE', #9658, #8272, #10072, .T. ) ;
#21871 = AXIS2_PLACEMENT_3D ( 'NONE', #33150, #49197, #4524 ) ;
#21872 = EDGE_CURVE ( 'NONE', #3584, #25092, #33717, .T. ) ;
#21873 = CARTESIAN_POINT ( 'NONE',  ( -339.1964088526558498, -130.1153096980153236, -58.63009191191284941 ) ) ;
#21875 = ORIENTED_EDGE ( 'NONE', *, *, #30251, .T. ) ;
#21874 = CARTESIAN_POINT ( 'NONE',  ( -332.3517673607765914, -182.5000000000000568, 2.632288850093980503 ) ) ;
#21876 = VERTEX_POINT ( 'NONE', #30038 ) ;
#21877 = ORIENTED_EDGE ( 'NONE', *, *, #3949, .F. ) ;
#21878 = CARTESIAN_POINT ( 'NONE',  ( -162.7543581613524282, -183.6283474603465606, 50.65739320402011003 ) ) ;
#21879 = FACE_OUTER_BOUND ( 'NONE', #1669, .T. ) ;
#21880 = CARTESIAN_POINT ( 'NONE',  ( -160.0000000000000284, -123.5000000000000284, 37.63467731922665394 ) ) ;
#21881 = EDGE_LOOP ( 'NONE', ( #5092, #16942, #24345, #49814 ) ) ;
#21882 = DIRECTION ( 'NONE',  ( 1.000000000000000000, 0.000000000000000000, 0.000000000000000000 ) ) ;
#21883 = CARTESIAN_POINT ( 'NONE',  ( -339.1964088526558498, -137.1341532842531876, -57.40522506028080585 ) ) ;
#21885 = ORIENTED_EDGE ( 'NONE', *, *, #37390, .T. ) ;
#21884 = CARTESIAN_POINT ( 'NONE',  ( -339.1964088526558498, -167.3305728129748786, -39.49849221029221269 ) ) ;
#21886 = AXIS2_PLACEMENT_3D ( 'NONE', #2289, #13337, #29350 ) ;
#21887 = LINE ( 'NONE', #17941, #36477 ) ;
#21888 = ORIENTED_EDGE ( 'NONE', *, *, #42548, .F. ) ;
#21889 = DIRECTION ( 'NONE',  ( 1.000000000000000000, -4.952603889763928634E-17, 7.175085443855162194E-17 ) ) ;
#21890 = VERTEX_POINT ( 'NONE', #45563 ) ;
#21891 = CARTESIAN_POINT ( 'NONE',  ( -124.1938582159088327, -193.5000000000000000, -99.45993886622791536 ) ) ;
#21892 = CARTESIAN_POINT ( 'NONE',  ( 46.01898237923984425, -183.6283474603465606, -81.82363577055903647 ) ) ;
#21893 = CARTESIAN_POINT ( 'NONE',  ( 53.18081239921338721, -193.5000000000000000, -72.73415134495935774 ) ) ;
#21894 = EDGE_CURVE ( 'NONE', #24400, #51107, #21372, .T. ) ;
#21895 = ORIENTED_EDGE ( 'NONE', *, *, #34549, .T. ) ;
#21896 = EDGE_LOOP ( 'NONE', ( #39581, #28949, #42862, #27714 ) ) ;
#21897 = PLANE ( 'NONE',  #3843 ) ;
#21898 = CARTESIAN_POINT ( 'NONE',  ( -158.3442440847887269, -175.3837268820161057, -59.62093586438114556 ) ) ;
#21899 = ORIENTED_EDGE ( 'NONE', *, *, #40701, .F. ) ;
#21900 = LINE ( 'NONE', #46338, #34976 ) ;
#21901 = VECTOR ( 'NONE', #45825, 1000.000000000000000 ) ;
#21902 = VERTEX_POINT ( 'NONE', #49516 ) ;
#21903 = CARTESIAN_POINT ( 'NONE',  ( -339.1964088526558498, -175.5095439275177398, -27.86139516340860212 ) ) ;
#21904 = DIRECTION ( 'NONE',  ( -0.9646355819083556327, 0.000000000000000000, -0.2635871660690782825 ) ) ;
#21905 = AXIS2_PLACEMENT_3D ( 'NONE', #28617, #21010, #44665 ) ;
#21906 = VERTEX_POINT ( 'NONE', #34487 ) ;
#21907 = LINE ( 'NONE', #42650, #35807 ) ;
#21908 = ORIENTED_EDGE ( 'NONE', *, *, #49139, .F. ) ;
#21909 = DIRECTION ( 'NONE',  ( 0.000000000000000000, -0.000000000000000000, 1.000000000000000000 ) ) ;
#21910 = DIRECTION ( 'NONE',  ( -0.000000000000000000, 0.8229838658936613482, 0.5680647467311485954 ) ) ;
#21911 = DIRECTION ( 'NONE',  ( -1.000000000000000000, -0.000000000000000000, -0.000000000000000000 ) ) ;
#21912 = ORIENTED_EDGE ( 'NONE', *, *, #49555, .T. ) ;
#21913 = CARTESIAN_POINT ( 'NONE',  ( -107.1845112550870027, -193.5000000000000000, 109.2239789693437331 ) ) ;
#21914 = DIRECTION ( 'NONE',  ( 0.000000000000000000, -1.000000000000000000, 0.000000000000000000 ) ) ;
#21915 = PLANE ( 'NONE',  #48411 ) ;
#21916 = DIRECTION ( 'NONE',  ( 0.000000000000000000, 1.595945597898662527E-14, -1.000000000000000000 ) ) ;
#21917 = VERTEX_POINT ( 'NONE', #42115 ) ;
#21918 = CARTESIAN_POINT ( 'NONE',  ( -330.4913330509368166, -70.60684477890994515, -28.32515014536850018 ) ) ;
#21919 = VERTEX_POINT ( 'NONE', #2445 ) ;
#21920 = VECTOR ( 'NONE', #43519, 1000.000000000000000 ) ;
#21921 = CARTESIAN_POINT ( 'NONE',  ( -336.3521761649654422, -123.5000000000000284, 0.000000000000000000 ) ) ;
#21923 = ORIENTED_EDGE ( 'NONE', *, *, #31118, .T. ) ;
#21922 = DIRECTION ( 'NONE',  ( 0.000000000000000000, -0.000000000000000000, -1.000000000000000000 ) ) ;
#21924 = VERTEX_POINT ( 'NONE', #13490 ) ;
#21925 = EDGE_CURVE ( 'NONE', #4153, #26290, #2176, .T. ) ;
#21926 = CARTESIAN_POINT ( 'NONE',  ( -330.4913330509368166, -162.2499814621210419, 44.49369547121568758 ) ) ;
#21927 = VERTEX_POINT ( 'NONE', #5622 ) ;
#21928 = CARTESIAN_POINT ( 'NONE',  ( -280.0000000000000000, -153.5000000000000284, 60.00000000000002132 ) ) ;
#21929 = VERTEX_POINT ( 'NONE', #29509 ) ;
#21930 = PLANE ( 'NONE',  #19158 ) ;
#21931 = CARTESIAN_POINT ( 'NONE',  ( -173.3294908491238004, -183.6283474603465606, -6.114457023560960991 ) ) ;
#21932 = AXIS2_PLACEMENT_3D ( 'NONE', #1351, #17662, #2121 ) ;
#21933 = DIRECTION ( 'NONE',  ( 0.000000000000000000, 0.9927088740980538617, -0.1205366802553232974 ) ) ;
#21934 = CARTESIAN_POINT ( 'NONE',  ( 8.448131207122518305, -189.7472609257535510, 111.2847127925100068 ) ) ;
#21935 = ORIENTED_EDGE ( 'NONE', *, *, #44612, .F. ) ;
#21936 = VERTEX_POINT ( 'NONE', #9810 ) ;
#21938 = ORIENTED_EDGE ( 'NONE', *, *, #26241, .T. ) ;
#21937 = VECTOR ( 'NONE', #18241, 1000.000000000000000 ) ;
#21939 = DIRECTION ( 'NONE',  ( 0.9785564922995032555, 0.000000000000000000, 0.2059786187411021818 ) ) ;
#21940 = CARTESIAN_POINT ( 'NONE',  ( 3.686287386450715076E-15, 20.00000000000000000, -46.00000000000000711 ) ) ;
#21941 = ADVANCED_FACE ( 'NONE', ( #37667 ), #5883, .F. ) ;
#21942 = DIRECTION ( 'NONE',  ( -0.8124868780056825335, 0.000000000000000000, 0.5829794791144703447 ) ) ;
#21943 = LINE ( 'NONE', #2233, #7893 ) ;
#21944 = ORIENTED_EDGE ( 'NONE', *, *, #40290, .T. ) ;
#21945 = VECTOR ( 'NONE', #12469, 999.9999999999998863 ) ;
#21946 = EDGE_LOOP ( 'NONE', ( #14356, #20338, #26978, #40858 ) ) ;
#21948 = EDGE_LOOP ( 'NONE', ( #45106, #28006, #34121, #20154 ) ) ;
#21947 = DIRECTION ( 'NONE',  ( -0.000000000000000000, 1.000000000000000000, 0.000000000000000000 ) ) ;
#21949 = AXIS2_PLACEMENT_3D ( 'NONE', #12418, #20564, #15602 ) ;
#21950 = LINE ( 'NONE', #49568, #17479 ) ;
#21951 = EDGE_CURVE ( 'NONE', #23290, #8865, #20689, .T. ) ;
#21952 = PLANE ( 'NONE',  #44170 ) ;
#21953 = DIRECTION ( 'NONE',  ( 0.000000000000000000, -0.5000000000000054401, 0.8660254037844354880 ) ) ;
#21954 = FACE_OUTER_BOUND ( 'NONE', #9076, .T. ) ;
#21955 = ORIENTED_EDGE ( 'NONE', *, *, #12180, .F. ) ;
#21957 = EDGE_CURVE ( 'NONE', #20647, #10130, #1919, .T. ) ;
#21956 = CARTESIAN_POINT ( 'NONE',  ( -25.00456841203573077, 45.00000000000000000, 0.000000000000000000 ) ) ;
#21958 = ORIENTED_EDGE ( 'NONE', *, *, #24543, .T. ) ;
#21959 = EDGE_LOOP ( 'NONE', ( #14282, #23801, #45664, #1858 ) ) ;
#21960 = CARTESIAN_POINT ( 'NONE',  ( -339.1964088526558498, -123.5000000000000284, 0.000000000000000000 ) ) ;
#21961 = EDGE_CURVE ( 'NONE', #5935, #43387, #21900, .T. ) ;
#21962 = DIRECTION ( 'NONE',  ( 0.000000000000000000, 0.000000000000000000, -1.000000000000000000 ) ) ;
#21963 = EDGE_LOOP ( 'NONE', ( #15693, #19025, #16493, #34443 ) ) ;
#21964 = VECTOR ( 'NONE', #36711, 1000.000000000000000 ) ;
#21965 = FACE_OUTER_BOUND ( 'NONE', #41252, .T. ) ;
#21966 = DIRECTION ( 'NONE',  ( 0.000000000000000000, -1.000000000000000000, 0.000000000000000000 ) ) ;
#21967 = DIRECTION ( 'NONE',  ( 0.000000000000000000, 1.000000000000000000, -0.000000000000000000 ) ) ;
#21968 = VECTOR ( 'NONE', #13889, 1000.000000000000000 ) ;
#21969 = CARTESIAN_POINT ( 'NONE',  ( -339.1964088526558498, -144.8891964568526305, -54.98865587491811624 ) ) ;
#21970 = CIRCLE ( 'NONE', #35388, 60.00000000000000000 ) ;
#21971 = EDGE_CURVE ( 'NONE', #29510, #28239, #31595, .T. ) ;
#21972 = CARTESIAN_POINT ( 'NONE',  ( 16.00000000000000000, -63.50000000000000000, 1.959434878635766315E-15 ) ) ;
#21973 = DIRECTION ( 'NONE',  ( -1.000000000000000000, 0.000000000000000000, 0.000000000000000000 ) ) ;
#21974 = VERTEX_POINT ( 'NONE', #37397 ) ;
#21975 = FACE_OUTER_BOUND ( 'NONE', #32904, .T. ) ;
#21976 = ORIENTED_EDGE ( 'NONE', *, *, #10249, .T. ) ;
#21977 = ORIENTED_EDGE ( 'NONE', *, *, #25687, .T. ) ;
#21978 = DIRECTION ( 'NONE',  ( -1.000000000000000000, -0.000000000000000000, -0.000000000000000000 ) ) ;
#21979 = ADVANCED_FACE ( 'NONE', ( #38438 ), #30541, .T. ) ;
#21980 = ORIENTED_EDGE ( 'NONE', *, *, #37215, .F. ) ;
#21981 = VECTOR ( 'NONE', #20038, 999.9999999999998863 ) ;
#21982 = ADVANCED_FACE ( 'NONE', ( #43147 ), #23452, .F. ) ;
#21983 = FACE_OUTER_BOUND ( 'NONE', #16820, .T. ) ;
#21984 = VECTOR ( 'NONE', #1888, 1000.000000000000227 ) ;
#21985 = EDGE_CURVE ( 'NONE', #39885, #44797, #23195, .T. ) ;
#21986 = AXIS2_PLACEMENT_3D ( 'NONE', #21999, #50640, #30389 ) ;
#21987 = CARTESIAN_POINT ( 'NONE',  ( -36.09284319799462537, -177.1207230881787780, 124.3848060646152476 ) ) ;
#21989 = VERTEX_POINT ( 'NONE', #50793 ) ;
#21988 = DIRECTION ( 'NONE',  ( 0.000000000000000000, 0.8229838658936536877, -0.5680647467311596976 ) ) ;
#21990 = CARTESIAN_POINT ( 'NONE',  ( -14.52059121095390992, -177.1207230881787780, 119.2602935412682399 ) ) ;
#21991 = CARTESIAN_POINT ( 'NONE',  ( -106.2948367055610106, -193.5000000000000000, -110.8257356506552185 ) ) ;
#21992 = ORIENTED_EDGE ( 'NONE', *, *, #51366, .T. ) ;
#21993 = VERTEX_POINT ( 'NONE', #46859 ) ;
#21994 = ORIENTED_EDGE ( 'NONE', *, *, #25234, .F. ) ;
#21995 = DIRECTION ( 'NONE',  ( 0.000000000000000000, 0.000000000000000000, -1.000000000000000000 ) ) ;
#21996 = DIRECTION ( 'NONE',  ( -0.000000000000000000, 1.000000000000000000, -0.000000000000000000 ) ) ;
#21997 = EDGE_CURVE ( 'NONE', #36797, #172, #19252, .T. ) ;
#21998 = DIRECTION ( 'NONE',  ( -0.000000000000000000, 1.000000000000000000, -0.000000000000000000 ) ) ;
#21999 = CARTESIAN_POINT ( 'NONE',  ( -332.3517673607765914, -67.40061919120938683, 18.46045550523129819 ) ) ;
#22000 = DIRECTION ( 'NONE',  ( 0.000000000000000000, -1.000000000000000000, -0.000000000000000000 ) ) ;
#22001 = CIRCLE ( 'NONE', #15289, 125.0000000000000000 ) ;
#22002 = EDGE_LOOP ( 'NONE', ( #4411, #14118, #17304, #32024 ) ) ;
#22003 = EDGE_CURVE ( 'NONE', #33649, #38645, #35011, .T. ) ;
#22004 = VECTOR ( 'NONE', #25475, 1000.000000000000000 ) ;
#22005 = DIRECTION ( 'NONE',  ( 0.000000000000000000, 0.000000000000000000, 1.000000000000000000 ) ) ;
#22006 = VERTEX_POINT ( 'NONE', #47884 ) ;
#22008 = ORIENTED_EDGE ( 'NONE', *, *, #35392, .T. ) ;
#22007 = FACE_OUTER_BOUND ( 'NONE', #26275, .T. ) ;
#22009 = ORIENTED_EDGE ( 'NONE', *, *, #31274, .F. ) ;
#22010 = ORIENTED_EDGE ( 'NONE', *, *, #25783, .F. ) ;
#22011 = DIRECTION ( 'NONE',  ( 0.000000000000000000, -1.000000000000000000, 0.000000000000000000 ) ) ;
#22012 = ORIENTED_EDGE ( 'NONE', *, *, #47987, .T. ) ;
#22013 = CARTESIAN_POINT ( 'NONE',  ( -48.93575598890255662, -177.1207230881787780, -0.8896570909947461026 ) ) ;
#22014 = PLANE ( 'NONE',  #15018 ) ;
#22015 = ORIENTED_EDGE ( 'NONE', *, *, #10116, .F. ) ;
#22016 = CARTESIAN_POINT ( 'NONE',  ( -48.47912675150885065, -175.3837268820161057, 6.938893903907228378E-15 ) ) ;
#22017 = ORIENTED_EDGE ( 'NONE', *, *, #16737, .F. ) ;
#22018 = VECTOR ( 'NONE', #19217, 1000.000000000000000 ) ;
#22019 = VECTOR ( 'NONE', #34798, 1000.000000000000000 ) ;
#22020 = ORIENTED_EDGE ( 'NONE', *, *, #47791, .T. ) ;
#22021 = LINE ( 'NONE', #38569, #18673 ) ;
#22022 = VECTOR ( 'NONE', #708, 1000.000000000000114 ) ;
#22023 = DIRECTION ( 'NONE',  ( 0.000000000000000000, 1.047444401652940007E-14, 1.000000000000000000 ) ) ;
#22024 = CARTESIAN_POINT ( 'NONE',  ( -94.25732089370191602, -177.1207230881787780, 116.3157639405754935 ) ) ;
#22025 = ORIENTED_EDGE ( 'NONE', *, *, #17351, .F. ) ;
#22026 = PLANE ( 'NONE',  #8898 ) ;
#22027 = CARTESIAN_POINT ( 'NONE',  ( -144.8751831225492310, -175.3837268820161057, 77.99872144864771428 ) ) ;
#22028 = EDGE_CURVE ( 'NONE', #41304, #31069, #18988, .T. ) ;
#22029 = EDGE_CURVE ( 'NONE', #27228, #45277, #6896, .T. ) ;
#22030 = DIRECTION ( 'NONE',  ( 0.000000000000000000, 5.851800525628429686E-14, -1.000000000000000000 ) ) ;
#22031 = LINE ( 'NONE', #2332, #16138 ) ;
#22032 = ORIENTED_EDGE ( 'NONE', *, *, #16836, .F. ) ;
#22033 = DIRECTION ( 'NONE',  ( 0.000000000000000000, 0.000000000000000000, -1.000000000000000000 ) ) ;
#22034 = PLANE ( 'NONE',  #26489 ) ;
#22035 = LINE ( 'NONE', #9965, #29085 ) ;
#22036 = ORIENTED_EDGE ( 'NONE', *, *, #46192, .T. ) ;
#22037 = EDGE_LOOP ( 'NONE', ( #517, #15002, #21223, #1797 ) ) ;
#22038 = CARTESIAN_POINT ( 'NONE',  ( -48.47912675150885065, -117.5479369270332057, -14.99999999999999289 ) ) ;
#22039 = CIRCLE ( 'NONE', #2715, 60.00000000000000000 ) ;
#22040 = FACE_BOUND ( 'NONE', #44042, .T. ) ;
#22041 = VERTEX_POINT ( 'NONE', #2948 ) ;
#22042 = CARTESIAN_POINT ( 'NONE',  ( 25.43954814678888710, -177.1207230881787780, 100.8019320314832754 ) ) ;
#22043 = EDGE_CURVE ( 'NONE', #28733, #23058, #18729, .T. ) ;
#22044 = ORIENTED_EDGE ( 'NONE', *, *, #12505, .T. ) ;
#22045 = EDGE_CURVE ( 'NONE', #24942, #41052, #11615, .T. ) ;
#22046 = AXIS2_PLACEMENT_3D ( 'NONE', #38906, #18438, #30504 ) ;
#22047 = FACE_OUTER_BOUND ( 'NONE', #14944, .T. ) ;
#22048 = EDGE_CURVE ( 'NONE', #50461, #37855, #3716, .T. ) ;
#22049 = DIRECTION ( 'NONE',  ( -0.1768902751225802927, 0.000000000000000000, 0.9842305779475953864 ) ) ;
#22050 = DIRECTION ( 'NONE',  ( 0.9027978299657446470, 0.000000000000000000, -0.4300652022765183435 ) ) ;
#22051 = EDGE_CURVE ( 'NONE', #51292, #24976, #50947, .T. ) ;
#22052 = LINE ( 'NONE', #6031, #43425 ) ;
#22053 = CARTESIAN_POINT ( 'NONE',  ( -48.47912675150885065, -177.1207230881787780, 6.938893903907228378E-15 ) ) ;
#22054 = VECTOR ( 'NONE', #37753, 1000.000000000000114 ) ;
#22055 = ORIENTED_EDGE ( 'NONE', *, *, #10772, .F. ) ;
#22056 = LINE ( 'NONE', #37825, #35729 ) ;
#22057 = ORIENTED_EDGE ( 'NONE', *, *, #46917, .F. ) ;
#22058 = CARTESIAN_POINT ( 'NONE',  ( -48.18706998087188254, -193.5000000000000000, 0.9564009842765313074 ) ) ;
#22059 = VECTOR ( 'NONE', #26372, 1000.000000000000000 ) ;
#22060 = VECTOR ( 'NONE', #45322, 1000.000000000000000 ) ;
#22061 = ORIENTED_EDGE ( 'NONE', *, *, #13146, .F. ) ;
#22062 = DIRECTION ( 'NONE',  ( -0.6300878435817094392, 0.000000000000000000, -0.7765238627180437447 ) ) ;
#22063 = CIRCLE ( 'NONE', #13665, 60.00000000000000000 ) ;
#22064 = FACE_OUTER_BOUND ( 'NONE', #44278, .T. ) ;
#22065 = DIRECTION ( 'NONE',  ( 0.000000000000000000, 0.000000000000000000, 1.000000000000000000 ) ) ;
#22066 = VERTEX_POINT ( 'NONE', #15302 ) ;
#22069 = ORIENTED_EDGE ( 'NONE', *, *, #5882, .T. ) ;
#22068 = CYLINDRICAL_SURFACE ( 'NONE', #24750, 125.0000000000000000 ) ;
#22067 = CARTESIAN_POINT ( 'NONE',  ( 5.761208793373444359E-16, 50.59471834446340921, -21.36672353920344491 ) ) ;
#22070 = FACE_OUTER_BOUND ( 'NONE', #47387, .T. ) ;
#22071 = VERTEX_POINT ( 'NONE', #22928 ) ;
#22072 = CARTESIAN_POINT ( 'NONE',  ( -161.8276685539205744, -177.1207230881787780, 50.28156562190587664 ) ) ;
#22073 = VECTOR ( 'NONE', #48214, 1000.000000000000000 ) ;
#22074 = EDGE_LOOP ( 'NONE', ( #33740, #31540, #18253, #19815 ) ) ;
#22075 = LINE ( 'NONE', #38094, #39269 ) ;
#22078 = ORIENTED_EDGE ( 'NONE', *, *, #46441, .F. ) ;
#22077 = LINE ( 'NONE', #26021, #47483 ) ;
#22076 = CARTESIAN_POINT ( 'NONE',  ( -109.9568094315246185, -177.1207230881787780, -108.8370090194290754 ) ) ;
#22079 = EDGE_LOOP ( 'NONE', ( #43828, #49428, #28879, #2878 ) ) ;
#22080 = VECTOR ( 'NONE', #4023, 1000.000000000000000 ) ;
#22081 = DIRECTION ( 'NONE',  ( -0.4827922027307427477, 0.000000000000000000, -0.8757349421956379665 ) ) ;
#22082 = ORIENTED_EDGE ( 'NONE', *, *, #19539, .F. ) ;
#22083 = PLANE ( 'NONE',  #45502 ) ;
#22084 = CARTESIAN_POINT ( 'NONE',  ( -113.4314575050762102, -123.5000000000000284, 6.938893903907228378E-15 ) ) ;
#22085 = ORIENTED_EDGE ( 'NONE', *, *, #15654, .T. ) ;
#22086 = EDGE_CURVE ( 'NONE', #44410, #6055, #11340, .T. ) ;
#22087 = DIRECTION ( 'NONE',  ( -1.000000000000000000, -1.036104688092336522E-14, -1.258058860540498485E-15 ) ) ;
#22088 = DIRECTION ( 'NONE',  ( 0.000000000000000000, -1.595945597898662527E-14, -1.000000000000000000 ) ) ;
#22089 = CARTESIAN_POINT ( 'NONE',  ( -46.00000000000000711, 20.00000000000000000, -51.00000000000000000 ) ) ;
#22090 = CARTESIAN_POINT ( 'NONE',  ( -260.0000000000000000, -93.50000000000002842, 51.54700538379266561 ) ) ;
#22091 = DIRECTION ( 'NONE',  ( 0.000000000000000000, -0.000000000000000000, -1.000000000000000000 ) ) ;
#22092 = EDGE_CURVE ( 'NONE', #9490, #14709, #43671, .T. ) ;
#22093 = EDGE_CURVE ( 'NONE', #14725, #27177, #26572, .T. ) ;
#22094 = ORIENTED_EDGE ( 'NONE', *, *, #34306, .T. ) ;
#22095 = ADVANCED_FACE ( 'NONE', ( #6654 ), #7154, .T. ) ;
#22096 = SHAPE_REPRESENTATION_RELATIONSHIP ( 'NONE' , 'NONE' ,  #6277, #39951 ) ;
#22097 = CIRCLE ( 'NONE', #17041, 125.0000000000000000 ) ;
#22098 = PLANE ( 'NONE',  #22943 ) ;
#22099 = VECTOR ( 'NONE', #19090, 1000.000000000000114 ) ;
#22100 = DIRECTION ( 'NONE',  ( -0.1182731709213523247, 0.000000000000000000, -0.9929810960135185827 ) ) ;
#22101 = ADVANCED_FACE ( 'NONE', ( #31318 ), #47361, .T. ) ;
#22102 = CARTESIAN_POINT ( 'NONE',  ( 70.49476099643867144, -183.6283474603465606, 34.94873081740416865 ) ) ;
#22103 = VERTEX_POINT ( 'NONE', #7664 ) ;
#22104 = CIRCLE ( 'NONE', #23743, 125.0000000000000000 ) ;
#22105 = LINE ( 'NONE', #5842, #35719 ) ;
#22106 = EDGE_CURVE ( 'NONE', #19400, #44532, #3460, .T. ) ;
#22107 = CARTESIAN_POINT ( 'NONE',  ( -106.4764934152196645, -213.5000000000000000, -110.7307791902283043 ) ) ;
#22108 = CARTESIAN_POINT ( 'NONE',  ( 17.15229921100054611, -183.6283474603465606, -106.3838142112212921 ) ) ;
#22109 = DIRECTION ( 'NONE',  ( 1.000000000000000000, -0.000000000000000000, -0.000000000000000000 ) ) ;
#22110 = AXIS2_PLACEMENT_3D ( 'NONE', #9129, #13324, #34066 ) ;
#22111 = EDGE_CURVE ( 'NONE', #48301, #17063, #19744, .T. ) ;
#22112 = EDGE_CURVE ( 'NONE', #9601, #30050, #4351, .T. ) ;
#22113 = FACE_OUTER_BOUND ( 'NONE', #32570, .T. ) ;
#22114 = EDGE_CURVE ( 'NONE', #6993, #49807, #44557, .T. ) ;
#22115 = CARTESIAN_POINT ( 'NONE',  ( -339.1964088526558498, -167.9936954712150339, 38.74998146212178796 ) ) ;
#22116 = LINE ( 'NONE', #37881, #37981 ) ;
#22117 = DIRECTION ( 'NONE',  ( -0.000000000000000000, 1.000000000000000000, -0.000000000000000000 ) ) ;
#22118 = AXIS2_PLACEMENT_3D ( 'NONE', #39282, #4066, #35081 ) ;
#22119 = EDGE_CURVE ( 'NONE', #4209, #35348, #3569, .T. ) ;
#22120 = ORIENTED_EDGE ( 'NONE', *, *, #33724, .F. ) ;
#22121 = CARTESIAN_POINT ( 'NONE',  ( -2.174401709722253440, -183.6283474603465606, -115.0304316645280096 ) ) ;
#22122 = EDGE_CURVE ( 'NONE', #20850, #25612, #24074, .T. ) ;
#22123 = CIRCLE ( 'NONE', #28815, 60.00000000000000000 ) ;
#22124 = CARTESIAN_POINT ( 'NONE',  ( -49.17567778057185990, -175.3837268820161057, 0.7175072570443320474 ) ) ;
#22126 = ORIENTED_EDGE ( 'NONE', *, *, #28128, .F. ) ;
#22125 = DIRECTION ( 'NONE',  ( -0.000000000000000000, 0.000000000000000000, 1.000000000000000000 ) ) ;
#22127 = ORIENTED_EDGE ( 'NONE', *, *, #17032, .F. ) ;
#22128 = ORIENTED_EDGE ( 'NONE', *, *, #4359, .F. ) ;
#22129 = FACE_OUTER_BOUND ( 'NONE', #44830, .T. ) ;
#22130 = PLANE ( 'NONE',  #27785 ) ;
#22131 = CARTESIAN_POINT ( 'NONE',  ( -330.4913330509368166, -123.5000000000000284, 0.000000000000000000 ) ) ;
#22133 = ORIENTED_EDGE ( 'NONE', *, *, #49530, .T. ) ;
#22132 = AXIS2_PLACEMENT_3D ( 'NONE', #5612, #16666, #32673 ) ;
#22134 = ADVANCED_FACE ( 'NONE', ( #27999 ), #8542, .F. ) ;
#22135 = DIRECTION ( 'NONE',  ( 0.000000000000000000, -1.000000000000000000, 0.000000000000000000 ) ) ;
#22136 = CARTESIAN_POINT ( 'NONE',  ( -330.4913330509368166, -109.8658467157472813, -57.40522506028090532 ) ) ;
#22139 = EDGE_LOOP ( 'NONE', ( #18042, #5450, #44860, #51674 ) ) ;
#22138 = CARTESIAN_POINT ( 'NONE',  ( 56.77503207194100554, -175.3837268820161057, -67.42819922234311036 ) ) ;
#22137 = DIRECTION ( 'NONE',  ( 0.9473263538541876194, 0.000000000000000000, 0.3202698538628486746 ) ) ;
#22140 = VECTOR ( 'NONE', #8377, 1000.000000000000000 ) ;
#22141 = CARTESIAN_POINT ( 'NONE',  ( -80.17897391495031911, -193.5000000000000000, 120.9136869416132498 ) ) ;
#22142 = ORIENTED_EDGE ( 'NONE', *, *, #29275, .F. ) ;
#22143 = DIRECTION ( 'NONE',  ( 0.000000000000000000, 0.000000000000000000, 1.000000000000000000 ) ) ;
#22144 = ORIENTED_EDGE ( 'NONE', *, *, #30976, .T. ) ;
#22145 = DIRECTION ( 'NONE',  ( 0.000000000000000000, 1.047444401652940007E-14, 1.000000000000000000 ) ) ;
#22146 = CARTESIAN_POINT ( 'NONE',  ( -332.3517673607765914, -153.2494431741581025, -51.01861988938816950 ) ) ;
#22147 = LINE ( 'NONE', #21893, #8097 ) ;
#22148 = ADVANCED_FACE ( 'NONE', ( #142 ), #43525, .T. ) ;
#22149 = ORIENTED_EDGE ( 'NONE', *, *, #46754, .T. ) ;
#22150 = FACE_OUTER_BOUND ( 'NONE', #28335, .T. ) ;
#22151 = DIRECTION ( 'NONE',  ( -0.000000000000000000, 0.000000000000000000, -1.000000000000000000 ) ) ;
#22152 = ORIENTED_EDGE ( 'NONE', *, *, #30859, .T. ) ;
#22153 = FACE_OUTER_BOUND ( 'NONE', #50320, .T. ) ;
#22154 = VECTOR ( 'NONE', #1278, 1000.000000000000000 ) ;
#22155 = EDGE_CURVE ( 'NONE', #38089, #33159, #8954, .T. ) ;
#22156 = EDGE_CURVE ( 'NONE', #43203, #7649, #4794, .T. ) ;
#22157 = VERTEX_POINT ( 'NONE', #31692 ) ;
#22158 = FACE_BOUND ( 'NONE', #11153, .T. ) ;
#22159 = DIRECTION ( 'NONE',  ( -0.000000000000000000, 0.8229838658936556861, -0.5680647467311569221 ) ) ;
#22160 = ADVANCED_FACE ( 'NONE', ( #40090 ), #44033, .T. ) ;
#22161 = ORIENTED_EDGE ( 'NONE', *, *, #50844, .T. ) ;
#22162 = DIRECTION ( 'NONE',  ( 1.000000000000000000, 0.000000000000000000, 0.000000000000000000 ) ) ;
#22163 = ORIENTED_EDGE ( 'NONE', *, *, #42974, .F. ) ;
#22164 = CARTESIAN_POINT ( 'NONE',  ( -46.06708674231131084, -193.5000000000000000, -124.9767260852756863 ) ) ;
#22165 = LINE ( 'NONE', #34250, #31221 ) ;
#22166 = ORIENTED_EDGE ( 'NONE', *, *, #39755, .T. ) ;
#22167 = DIRECTION ( 'NONE',  ( -0.000000000000000000, 1.000000000000000000, -0.000000000000000000 ) ) ;
#22168 = CARTESIAN_POINT ( 'NONE',  ( -339.1964088526558498, -79.00630452878473875, -38.74998146212148953 ) ) ;
#22169 = CARTESIAN_POINT ( 'NONE',  ( 24.63024857337166296, -193.5000000000000000, 101.3904297239426597 ) ) ;
#22170 = VECTOR ( 'NONE', #18194, 1000.000000000000000 ) ;
#22171 = VERTEX_POINT ( 'NONE', #19862 ) ;
#22172 = DIRECTION ( 'NONE',  ( -0.000000000000000000, 1.000000000000000000, -0.000000000000000000 ) ) ;
#22173 = ORIENTED_EDGE ( 'NONE', *, *, #37212, .T. ) ;
#22174 = EDGE_CURVE ( 'NONE', #44157, #13761, #20375, .T. ) ;
#22175 = FACE_OUTER_BOUND ( 'NONE', #19947, .T. ) ;
#22176 = DIRECTION ( 'NONE',  ( 0.000000000000000000, 0.000000000000000000, -1.000000000000000000 ) ) ;
#22178 = EDGE_LOOP ( 'NONE', ( #47527, #44610, #23792, #47960 ) ) ;
#22177 = LINE ( 'NONE', #18243, #6045 ) ;
#22179 = EDGE_CURVE ( 'NONE', #51005, #34028, #35896, .T. ) ;
#22180 = ORIENTED_EDGE ( 'NONE', *, *, #40145, .F. ) ;
#22181 = DIRECTION ( 'NONE',  ( 0.000000000000000000, 0.6631226582408017434, 0.7485107481710954191 ) ) ;
#22182 = EDGE_CURVE ( 'NONE', #36635, #45987, #32468, .T. ) ;
#22183 = DIRECTION ( 'NONE',  ( -1.000000000000000000, -0.000000000000000000, 0.000000000000000000 ) ) ;
#22184 = ORIENTED_EDGE ( 'NONE', *, *, #19532, .T. ) ;
#22185 = LINE ( 'NONE', #38473, #23910 ) ;
#22186 = VERTEX_POINT ( 'NONE', #8300 ) ;
#22187 = CARTESIAN_POINT ( 'NONE',  ( -339.1964088526558498, -75.22798428563942252, 33.92731199008440512 ) ) ;
#22188 = DIRECTION ( 'NONE',  ( -8.718379230999709592E-17, 0.8854560256532079121, -0.4647231720437725033 ) ) ;
#22189 = VECTOR ( 'NONE', #2674, 1000.000000000000114 ) ;
#22190 = AXIS2_PLACEMENT_3D ( 'NONE', #48608, #8641, #45437 ) ;
#22191 = CARTESIAN_POINT ( 'NONE',  ( -123.0610352593084400, -175.3837268820161057, 99.06333546307732263 ) ) ;
#22192 = DIRECTION ( 'NONE',  ( 0.000000000000000000, 0.000000000000000000, 1.000000000000000000 ) ) ;
#22193 = VERTEX_POINT ( 'NONE', #51944 ) ;
#22194 = VERTEX_POINT ( 'NONE', #20118 ) ;
#22195 = CIRCLE ( 'NONE', #18002, 4.999999999999997335 ) ;
#22196 = ORIENTED_EDGE ( 'NONE', *, *, #41593, .F. ) ;
#22197 = DIRECTION ( 'NONE',  ( -0.000000000000000000, -0.1205366802553233113, -0.9927088740980538617 ) ) ;
#22198 = DIRECTION ( 'NONE',  ( 0.000000000000000000, 0.000000000000000000, 1.000000000000000000 ) ) ;
#22199 = DIRECTION ( 'NONE',  ( -0.5829794791144703447, 0.000000000000000000, -0.8124868780056825335 ) ) ;
#22200 = LINE ( 'NONE', #26909, #44862 ) ;
#22201 = VERTEX_POINT ( 'NONE', #24325 ) ;
#22202 = CIRCLE ( 'NONE', #48209, 125.0000000000000000 ) ;
#22203 = CARTESIAN_POINT ( 'NONE',  ( 72.31641062551800303, -189.7472609257535510, 32.14713283941990341 ) ) ;
#22204 = ORIENTED_EDGE ( 'NONE', *, *, #10648, .T. ) ;
#22206 = VERTEX_POINT ( 'NONE', #16723 ) ;
#22205 = CARTESIAN_POINT ( 'NONE',  ( -332.3517673607765914, -148.5878911270064009, 53.46519113769075204 ) ) ;
#22207 = CARTESIAN_POINT ( 'NONE',  ( -114.9451385648675767, -183.6283474603465606, -104.6823626202120181 ) ) ;
#22208 = DIRECTION ( 'NONE',  ( -0.000000000000000000, -0.5680647467311596976, -0.8229838658936536877 ) ) ;
#22209 = CARTESIAN_POINT ( 'NONE',  ( -339.1964088526558498, -162.9984922102927385, -43.83057281297435992 ) ) ;
#22210 = EDGE_CURVE ( 'NONE', #44850, #2592, #8036, .T. ) ;
#22212 = EDGE_CURVE ( 'NONE', #17102, #19374, #32727, .T. ) ;
#22211 = LINE ( 'NONE', #17520, #782 ) ;
#22213 = EDGE_LOOP ( 'NONE', ( #34980, #49303, #33127, #5156 ) ) ;
#22214 = DIRECTION ( 'NONE',  ( 0.000000000000000000, -1.000000000000000000, 0.000000000000000000 ) ) ;
#22215 = ORIENTED_EDGE ( 'NONE', *, *, #45149, .F. ) ;
#22216 = EDGE_LOOP ( 'NONE', ( #29883, #18167, #35614, #3262 ) ) ;
#22217 = FACE_OUTER_BOUND ( 'NONE', #8390, .T. ) ;
#22218 = LINE ( 'NONE', #1988, #8527 ) ;
#22219 = EDGE_LOOP ( 'NONE', ( #21938, #49431, #21686, #1600 ) ) ;
#22220 = AXIS2_PLACEMENT_3D ( 'NONE', #51296, #42879, #38927 ) ;
#22221 = AXIS2_PLACEMENT_3D ( 'NONE', #23889, #35718, #51773 ) ;
#22222 = LINE ( 'NONE', #50607, #49217 ) ;
#22223 = DIRECTION ( 'NONE',  ( 0.000000000000000000, 0.9709418174260526779, 0.2393156642875547968 ) ) ;
#22224 = PLANE ( 'NONE',  #31572 ) ;
#22225 = LINE ( 'NONE', #2265, #22368 ) ;
#22226 = AXIS2_PLACEMENT_3D ( 'NONE', #45984, #48680, #12650 ) ;
#22227 = CARTESIAN_POINT ( 'NONE',  ( -332.3517673607765914, -110.9652333097088217, -57.67619951860654481 ) ) ;
#22228 = VERTEX_POINT ( 'NONE', #40331 ) ;
#22229 = ADVANCED_FACE ( 'NONE', ( #28512 ), #27740, .T. ) ;
#22230 = CYLINDRICAL_SURFACE ( 'NONE', #16818, 125.0000000000000000 ) ;
#22231 = ORIENTED_EDGE ( 'NONE', *, *, #1190, .F. ) ;
#22232 = ORIENTED_EDGE ( 'NONE', *, *, #13966, .F. ) ;
#22233 = FACE_OUTER_BOUND ( 'NONE', #321, .T. ) ;
#22234 = AXIS2_PLACEMENT_3D ( 'NONE', #39264, #31626, #3770 ) ;
#22235 = ORIENTED_EDGE ( 'NONE', *, *, #19070, .F. ) ;
#22236 = EDGE_CURVE ( 'NONE', #11493, #46287, #46740, .T. ) ;
#22237 = LINE ( 'NONE', #21214, #23460 ) ;
#22238 = DIRECTION ( 'NONE',  ( -1.000000000000000000, 0.000000000000000000, 0.000000000000000000 ) ) ;
#22239 = DIRECTION ( 'NONE',  ( 0.000000000000000000, -0.8854560256532044704, 0.4647231720437789981 ) ) ;
#22240 = ORIENTED_EDGE ( 'NONE', *, *, #47190, .F. ) ;
#22241 = DIRECTION ( 'NONE',  ( 0.000000000000000000, 0.000000000000000000, -1.000000000000000000 ) ) ;
#22242 = LINE ( 'NONE', #13585, #36124 ) ;
#22243 = CARTESIAN_POINT ( 'NONE',  ( -305.0000000000000568, -123.5000000000000284, 0.000000000000000000 ) ) ;
#22244 = VERTEX_POINT ( 'NONE', #5925 ) ;
#22245 = ORIENTED_EDGE ( 'NONE', *, *, #11556, .T. ) ;
#22246 = ORIENTED_EDGE ( 'NONE', *, *, #3694, .F. ) ;
#22247 = CARTESIAN_POINT ( 'NONE',  ( -330.4913330509368166, -103.0458197858324496, 55.34326076196052213 ) ) ;
#22248 = DIRECTION ( 'NONE',  ( -0.3482016354343928088, 0.000000000000000000, -0.9374196611341231167 ) ) ;
#22249 = VECTOR ( 'NONE', #18086, 1000.000000000000227 ) ;
#22250 = SURFACE_SIDE_STYLE ('',( #18331 ) ) ;
#22251 = AXIS2_PLACEMENT_3D ( 'NONE', #26919, #17816, #18784 ) ;
#22252 = LINE ( 'NONE', #5469, #37929 ) ;
#22253 = DIRECTION ( 'NONE',  ( -0.000000000000000000, -0.4647231720437724478, -0.8854560256532078011 ) ) ;
#22254 = EDGE_LOOP ( 'NONE', ( #33447, #698, #38783, #32077 ) ) ;
#22255 = CIRCLE ( 'NONE', #21401, 125.0000000000000000 ) ;
#22256 = CIRCLE ( 'NONE', #51643, 125.0000000000000000 ) ;
#22257 = EDGE_CURVE ( 'NONE', #42284, #16002, #41908, .T. ) ;
#22258 = DIRECTION ( 'NONE',  ( 0.000000000000000000, 0.000000000000000000, 1.000000000000000000 ) ) ;
#22259 = ORIENTED_EDGE ( 'NONE', *, *, #50961, .F. ) ;
#22261 = ORIENTED_EDGE ( 'NONE', *, *, #51905, .T. ) ;
#22260 = LINE ( 'NONE', #18340, #34858 ) ;
#22262 = EDGE_LOOP ( 'NONE', ( #25051, #46005, #3909, #24686 ) ) ;
#22263 = CARTESIAN_POINT ( 'NONE',  ( -58.29063029684667185, -183.6283474603465606, 124.6143426664034877 ) ) ;
#22264 = CIRCLE ( 'NONE', #7189, 125.0000000000000000 ) ;
#22265 = ORIENTED_EDGE ( 'NONE', *, *, #20245, .T. ) ;
#22266 = LINE ( 'NONE', #50921, #2328 ) ;
#22267 = VECTOR ( 'NONE', #2721, 1000.000000000000000 ) ;
#22268 = VERTEX_POINT ( 'NONE', #25615 ) ;
#22269 = CARTESIAN_POINT ( 'NONE',  ( -48.30223647638627682, -193.5000000000000000, -0.9842305779475897243 ) ) ;
#22270 = EDGE_CURVE ( 'NONE', #20473, #40560, #32975, .T. ) ;
#22271 = CARTESIAN_POINT ( 'NONE',  ( -305.0000000000000568, -103.7577981350106313, -56.65902810251876787 ) ) ;
#22272 = ORIENTED_EDGE ( 'NONE', *, *, #29337, .T. ) ;
#22273 = DIRECTION ( 'NONE',  ( 0.000000000000000000, 1.000000000000000000, -0.000000000000000000 ) ) ;
#22274 = VECTOR ( 'NONE', #38865, 1000.000000000000000 ) ;
#22275 = VERTEX_POINT ( 'NONE', #12739 ) ;
#22276 = CIRCLE ( 'NONE', #8843, 125.0000000000000000 ) ;
#22277 = VERTEX_POINT ( 'NONE', #17226 ) ;
#22278 = CARTESIAN_POINT ( 'NONE',  ( 32.49319223169170101, -189.7472609257535510, -95.22858582633061530 ) ) ;
#22279 = EDGE_CURVE ( 'NONE', #20473, #31066, #45862, .T. ) ;
#22280 = CARTESIAN_POINT ( 'NONE',  ( -336.3521761649654422, -121.8677111499054320, 59.00000000000001421 ) ) ;
#22281 = DIRECTION ( 'NONE',  ( 0.000000000000000000, 0.000000000000000000, -1.000000000000000000 ) ) ;
#22282 = EDGE_LOOP ( 'NONE', ( #46380, #42127, #26816, #10375 ) ) ;
#22283 = CARTESIAN_POINT ( 'NONE',  ( -330.4913330509368166, -64.50000000000000000, -0.4999999999999549249 ) ) ;
#22284 = DIRECTION ( 'NONE',  ( -0.000000000000000000, 1.000000000000000000, -0.000000000000000000 ) ) ;
#22285 = CARTESIAN_POINT ( 'NONE',  ( -171.0948786228703398, -193.5000000000000000, -18.47640724094508258 ) ) ;
#22286 = DIRECTION ( 'NONE',  ( 0.000000000000000000, 0.5000000000000012212, -0.8660254037844378194 ) ) ;
#22287 = ORIENTED_EDGE ( 'NONE', *, *, #43060, .T. ) ;
#22288 = PLANE ( 'NONE',  #11221 ) ;
#22289 = DIRECTION ( 'NONE',  ( 8.659560562354969836E-17, 0.7071067811865444641, -0.7071067811865505703 ) ) ;
#22290 = CARTESIAN_POINT ( 'NONE',  ( -172.6359455740846442, -177.1207230881787780, -14.49428645563791562 ) ) ;
#22291 = ORIENTED_EDGE ( 'NONE', *, *, #23285, .T. ) ;
#22292 = AXIS2_PLACEMENT_3D ( 'NONE', #49190, #24742, #41281 ) ;
#22293 = ADVANCED_FACE ( 'NONE', ( #16970 ), #3096, .T. ) ;
#22294 = CARTESIAN_POINT ( 'NONE',  ( 46.00000000000000711, 20.00000000000000000, -46.00000000000000000 ) ) ;
#22295 = CIRCLE ( 'NONE', #27316, 125.0000000000000000 ) ;
#22296 = VECTOR ( 'NONE', #12646, 999.9999999999998863 ) ;
#22297 = PLANE ( 'NONE',  #2584 ) ;
#22298 = ORIENTED_EDGE ( 'NONE', *, *, #34380, .T. ) ;
#22299 = CARTESIAN_POINT ( 'NONE',  ( -147.0463339291296165, -177.1207230881787780, 76.87330921200147316 ) ) ;
#22300 = EDGE_LOOP ( 'NONE', ( #33043, #3861 ) ) ;
#22301 = CYLINDRICAL_SURFACE ( 'NONE', #20916, 125.0000000000000000 ) ;
#22302 = CARTESIAN_POINT ( 'NONE',  ( -336.3521761649654422, -127.9985676343858501, 58.88711093124869222 ) ) ;
#22303 = AXIS2_PLACEMENT_3D ( 'NONE', #17509, #33525, #9606 ) ;
#22304 = CARTESIAN_POINT ( 'NONE',  ( -336.3521761649654422, -169.4076645216271402, -37.15394033962039089 ) ) ;
#22305 = AXIS2_PLACEMENT_3D ( 'NONE', #17259, #44847, #49837 ) ;
#22306 = LINE ( 'NONE', #30443, #4828 ) ;
#22307 = AXIS2_PLACEMENT_3D ( 'NONE', #34034, #2746, #18782 ) ;
#22308 = PLANE ( 'NONE',  #5880 ) ;
#22309 = ORIENTED_EDGE ( 'NONE', *, *, #21971, .T. ) ;
#22310 = CARTESIAN_POINT ( 'NONE',  ( 50.08808042611237710, -193.5000000000000000, -76.87330921200083367 ) ) ;
#22311 = ORIENTED_EDGE ( 'NONE', *, *, #44941, .F. ) ;
#22312 = VECTOR ( 'NONE', #40540, 1000.000000000000000 ) ;
#22313 = DIRECTION ( 'NONE',  ( 0.000000000000000000, 0.000000000000000000, 1.000000000000000000 ) ) ;
#22314 = VERTEX_POINT ( 'NONE', #924 ) ;
#22315 = LINE ( 'NONE', #10232, #9972 ) ;
#22316 = ADVANCED_FACE ( 'NONE', ( #49024 ), #37963, .T. ) ;
#22317 = CARTESIAN_POINT ( 'NONE',  ( -81.14588623932564815, -183.6283474603465606, 120.6560517527617833 ) ) ;
#22318 = DIRECTION ( 'NONE',  ( 0.000000000000000000, -0.1205366802553095168, 0.9927088740980556381 ) ) ;
#22319 = ORIENTED_EDGE ( 'NONE', *, *, #48074, .T. ) ;
#22322 = ORIENTED_EDGE ( 'NONE', *, *, #20435, .F. ) ;
#22321 = CARTESIAN_POINT ( 'NONE',  ( -48.47912675150885065, -183.6283474603465606, 6.938893903907228378E-15 ) ) ;
#22320 = CARTESIAN_POINT ( 'NONE',  ( -78.64590280292341617, -189.7472609257535510, -121.3052580173827408 ) ) ;
#22323 = VECTOR ( 'NONE', #34385, 1000.000000000000000 ) ;
#22324 = AXIS2_PLACEMENT_3D ( 'NONE', #50935, #18853, #43553 ) ;
#22325 = DIRECTION ( 'NONE',  ( -1.000000000000000000, 0.000000000000000000, 0.000000000000000000 ) ) ;
#22326 = VECTOR ( 'NONE', #17648, 1000.000000000000000 ) ;
#22327 = ORIENTED_EDGE ( 'NONE', *, *, #20136, .F. ) ;
#22328 = CARTESIAN_POINT ( 'NONE',  ( -339.1964088526558498, -84.00150778970699150, 43.83057281297409702 ) ) ;
#22329 = ORIENTED_EDGE ( 'NONE', *, *, #45830, .F. ) ;
#22330 = VECTOR ( 'NONE', #32826, 1000.000000000000000 ) ;
#22331 = EDGE_CURVE ( 'NONE', #33929, #14578, #16542, .T. ) ;
#22332 = DIRECTION ( 'NONE',  ( -0.000000000000000000, 0.3546048870425235200, -0.9350162426854194964 ) ) ;
#22335 = ORIENTED_EDGE ( 'NONE', *, *, #43042, .T. ) ;
#22334 = CARTESIAN_POINT ( 'NONE',  ( -339.1964088526558498, -143.9541802141672235, -55.34326076196065003 ) ) ;
#22333 = CARTESIAN_POINT ( 'NONE',  ( -305.0000000000000568, -122.9999999999997158, 59.99791663049642665 ) ) ;
#22336 = ORIENTED_EDGE ( 'NONE', *, *, #13498, .T. ) ;
#22337 = EDGE_CURVE ( 'NONE', #4879, #51539, #22378, .T. ) ;
#22338 = EDGE_CURVE ( 'NONE', #41080, #47840, #25117, .T. ) ;
#22339 = CARTESIAN_POINT ( 'NONE',  ( -336.3521761649654422, -83.15397741537739762, 43.07972642080338233 ) ) ;
#22340 = ORIENTED_EDGE ( 'NONE', *, *, #8914, .T. ) ;
#22341 = CARTESIAN_POINT ( 'NONE',  ( -140.8230258362169707, -175.3837268820161057, 84.24728067916045404 ) ) ;
#22342 = ADVANCED_FACE ( 'NONE', ( #13282 ), #21419, .T. ) ;
#22343 = DIRECTION ( 'NONE',  ( -0.000000000000000000, 1.000000000000000000, -0.000000000000000000 ) ) ;
#22344 = VERTEX_POINT ( 'NONE', #17750 ) ;
#22345 = EDGE_CURVE ( 'NONE', #5747, #33733, #44818, .T. ) ;
#22346 = AXIS2_PLACEMENT_3D ( 'NONE', #44803, #5385, #21139 ) ;
#22347 = CARTESIAN_POINT ( 'NONE',  ( -172.4728835572423975, -177.1207230881787780, 1.322128892812083123 ) ) ;
#22348 = DIRECTION ( 'NONE',  ( -0.000000000000000000, 1.000000000000000000, -0.000000000000000000 ) ) ;
#22349 = DIRECTION ( 'NONE',  ( 0.000000000000000000, -0.000000000000000000, 1.000000000000000000 ) ) ;
#22350 = DIRECTION ( 'NONE',  ( 0.9995608365087942371, 0.000000000000000000, 0.02963332782256331357 ) ) ;
#22351 = AXIS2_PLACEMENT_3D ( 'NONE', #1418, #8512, #40828 ) ;
#22352 = AXIS2_PLACEMENT_3D ( 'NONE', #38886, #7099, #23389 ) ;
#22353 = CARTESIAN_POINT ( 'NONE',  ( -55.05561436132770581, -189.7472609257535510, 124.8268793598474105 ) ) ;
#22354 = EDGE_LOOP ( 'NONE', ( #20371, #22962, #24973, #4024 ) ) ;
#22355 =( NAMED_UNIT ( * ) PLANE_ANGLE_UNIT ( ) SI_UNIT ( $, .RADIAN. ) );
#22356 = VECTOR ( 'NONE', #10939, 1000.000000000000000 ) ;
#22357 = LINE ( 'NONE', #31261, #20415 ) ;
#22358 = PLANE ( 'NONE',  #40770 ) ;
#22359 = AXIS2_PLACEMENT_3D ( 'NONE', #11161, #3024, #26691 ) ;
#22360 = PLANE ( 'NONE',  #30446 ) ;
#22361 = ORIENTED_EDGE ( 'NONE', *, *, #1448, .T. ) ;
#22362 = DIRECTION ( 'NONE',  ( 0.000000000000000000, -1.000000000000000000, 0.000000000000000000 ) ) ;
#22363 = CARTESIAN_POINT ( 'NONE',  ( -330.4913330509368166, -89.57268800991444380, 48.27201571435978877 ) ) ;
#22364 = CARTESIAN_POINT ( 'NONE',  ( -332.3517673607765914, -143.2422018649890276, 56.65902810251888155 ) ) ;
#22365 = CARTESIAN_POINT ( 'NONE',  ( -0.6536498292959382894, -193.5000000000000000, 114.4068333132749160 ) ) ;
#22366 = EDGE_LOOP ( 'NONE', ( #1431, #20325, #3430, #5851 ) ) ;
#22367 = DIRECTION ( 'NONE',  ( 0.000000000000000000, 0.000000000000000000, -1.000000000000000000 ) ) ;
#22368 = VECTOR ( 'NONE', #10660, 1000.000000000000227 ) ;
#22369 = CIRCLE ( 'NONE', #50108, 60.00000000000000000 ) ;
#22370 = CARTESIAN_POINT ( 'NONE',  ( -336.3521761649654422, -126.1322888500942270, -59.94223098458773080 ) ) ;
#22371 = CARTESIAN_POINT ( 'NONE',  ( -49.03777351731250889, -175.3837268820161057, 0.8294056854502042109 ) ) ;
#22372 = PLANE ( 'NONE',  #20317 ) ;
#22373 = ORIENTED_EDGE ( 'NONE', *, *, #8283, .F. ) ;
#22374 = DIRECTION ( 'NONE',  ( 0.000000000000000000, 0.9709418174260553425, 0.2393156642875448881 ) ) ;
#22375 = CARTESIAN_POINT ( 'NONE',  ( -24.23284180386169950, -193.5000000000000000, -121.6072260099953581 ) ) ;
#22377 = ORIENTED_EDGE ( 'NONE', *, *, #11810, .F. ) ;
#22376 = DIRECTION ( 'NONE',  ( 0.000000000000000000, 0.000000000000000000, -1.000000000000000000 ) ) ;
#22378 = CIRCLE ( 'NONE', #11494, 60.00000000000000000 ) ;
#22379 = ORIENTED_EDGE ( 'NONE', *, *, #14171, .F. ) ;
#22380 = AXIS2_PLACEMENT_3D ( 'NONE', #32030, #24171, #4194 ) ;
#22381 = ORIENTED_EDGE ( 'NONE', *, *, #45856, .T. ) ;
#22382 = FACE_OUTER_BOUND ( 'NONE', #8959, .T. ) ;
#22383 = AXIS2_PLACEMENT_3D ( 'NONE', #39350, #10458, #47510 ) ;
#22384 = AXIS2_PLACEMENT_3D ( 'NONE', #42510, #2825, #46990 ) ;
#22385 = ADVANCED_FACE ( 'NONE', ( #29303 ), #29555, .F. ) ;
#22386 = ADVANCED_FACE ( 'NONE', ( #5147 ), #5404, .F. ) ;
#22387 = EDGE_CURVE ( 'NONE', #20132, #16530, #25366, .T. ) ;
#22389 = AXIS2_PLACEMENT_3D ( 'NONE', #27994, #24069, #31164 ) ;
#22388 = CARTESIAN_POINT ( 'NONE',  ( 62.59443091842027940, -193.5000000000000000, -57.33816169485140790 ) ) ;
#22390 = DIRECTION ( 'NONE',  ( -1.000000000000000000, -0.000000000000000000, 0.000000000000000000 ) ) ;
#22391 = ORIENTED_EDGE ( 'NONE', *, *, #51826, .T. ) ;
#22392 = EDGE_CURVE ( 'NONE', #35941, #4690, #29815, .T. ) ;
#22393 = AXIS2_PLACEMENT_3D ( 'NONE', #51823, #24462, #28652 ) ;
#22394 = DIRECTION ( 'NONE',  ( 0.000000000000000000, 0.000000000000000000, 1.000000000000000000 ) ) ;
#22395 = LINE ( 'NONE', #22136, #21033 ) ;
#22398 = ORIENTED_EDGE ( 'NONE', *, *, #1048, .T. ) ;
#22397 = DIRECTION ( 'NONE',  ( -0.000000000000000000, 1.000000000000000000, -0.000000000000000000 ) ) ;
#22396 = DIRECTION ( 'NONE',  ( 0.000000000000000000, 0.000000000000000000, -1.000000000000000000 ) ) ;
#22399 = EDGE_CURVE ( 'NONE', #19699, #17256, #5669, .T. ) ;
#22400 = CARTESIAN_POINT ( 'NONE',  ( -336.3521761649654422, -180.4803820837415458, -18.79457521708939183 ) ) ;
#22401 = ORIENTED_EDGE ( 'NONE', *, *, #4499, .T. ) ;
#22402 = DIRECTION ( 'NONE',  ( 0.000000000000000000, 1.000000000000000000, 0.000000000000000000 ) ) ;
#22403 = ORIENTED_EDGE ( 'NONE', *, *, #4421, .T. ) ;
#22404 = DIRECTION ( 'NONE',  ( 0.000000000000000000, 0.000000000000000000, -1.000000000000000000 ) ) ;
#22405 = EDGE_CURVE ( 'NONE', #6473, #26602, #1707, .T. ) ;
#22406 = CARTESIAN_POINT ( 'NONE',  ( -365.0000000000001137, -168.5000000000000284, 0.000000000000000000 ) ) ;
#22407 = DIRECTION ( 'NONE',  ( -0.3758275821142488260, 0.000000000000000000, 0.9266896074318291543 ) ) ;
#22408 = EDGE_CURVE ( 'NONE', #24976, #18993, #13798, .T. ) ;
#22409 = FACE_OUTER_BOUND ( 'NONE', #6115, .T. ) ;
#22410 = VECTOR ( 'NONE', #17474, 1000.000000000000000 ) ;
#22411 = ORIENTED_EDGE ( 'NONE', *, *, #26895, .F. ) ;
#22412 = DIRECTION ( 'NONE',  ( -0.000000000000000000, 1.000000000000000000, -0.000000000000000000 ) ) ;
#22413 = VECTOR ( 'NONE', #26815, 1000.000000000000000 ) ;
#22414 = EDGE_CURVE ( 'NONE', #11641, #21393, #29998, .T. ) ;
#22415 = DIRECTION ( 'NONE',  ( -0.000000000000000000, 1.000000000000000000, -0.000000000000000000 ) ) ;
#22416 = ORIENTED_EDGE ( 'NONE', *, *, #23134, .F. ) ;
#22417 = CARTESIAN_POINT ( 'NONE',  ( -47.63353074800703268, -177.1207230881787780, 0.5338233779648018373 ) ) ;
#22418 = CIRCLE ( 'NONE', #50111, 125.0000000000000000 ) ;
#22419 = CARTESIAN_POINT ( 'NONE',  ( -332.3517673607765914, -126.1322888500942270, -59.00000000000001421 ) ) ;
#22420 = EDGE_CURVE ( 'NONE', #28114, #23398, #7345, .T. ) ;
#22421 = ORIENTED_EDGE ( 'NONE', *, *, #46537, .F. ) ;
#22422 = FACE_BOUND ( 'NONE', #40445, .T. ) ;
#22423 = DIRECTION ( 'NONE',  ( 0.000000000000000000, -0.000000000000000000, -1.000000000000000000 ) ) ;
#22424 = EDGE_LOOP ( 'NONE', ( #24996, #22173, #16709, #33306 ) ) ;
#22425 = CARTESIAN_POINT ( 'NONE',  ( -332.3517673607765914, -174.5186198893880771, 29.74944317415823392 ) ) ;
#22426 = ORIENTED_EDGE ( 'NONE', *, *, #21388, .F. ) ;
#22427 = AXIS2_PLACEMENT_3D ( 'NONE', #19092, #11186, #30378 ) ;
#22428 = DIRECTION ( 'NONE',  ( -0.2348860457809911206, 0.000000000000000000, 0.9720229140804089729 ) ) ;
#22429 = VECTOR ( 'NONE', #38667, 1000.000000000000000 ) ;
#22430 = CARTESIAN_POINT ( 'NONE',  ( -330.4913330509368166, -157.1712093821527390, 49.66134974749710551 ) ) ;
#22431 = ORIENTED_EDGE ( 'NONE', *, *, #29493, .T. ) ;
#22432 = AXIS2_PLACEMENT_3D ( 'NONE', #38675, #18718, #25442 ) ;
#22433 = VECTOR ( 'NONE', #26355, 1000.000000000000000 ) ;
#22434 = DIRECTION ( 'NONE',  ( 0.000000000000000000, 0.000000000000000000, -1.000000000000000000 ) ) ;
#22435 = LINE ( 'NONE', #34254, #4560 ) ;
#22436 = CARTESIAN_POINT ( 'NONE',  ( 40.30419662299490113, -193.5000000000000000, -87.99159897727903967 ) ) ;
#22437 = AXIS2_PLACEMENT_3D ( 'NONE', #854, #45024, #48440 ) ;
#22438 = EDGE_CURVE ( 'NONE', #3300, #27708, #34529, .T. ) ;
#22439 = ORIENTED_EDGE ( 'NONE', *, *, #6398, .F. ) ;
#22441 = VECTOR ( 'NONE', #37601, 1000.000000000000000 ) ;
#22440 = LINE ( 'NONE', #46108, #6946 ) ;
#22442 = ORIENTED_EDGE ( 'NONE', *, *, #2922, .T. ) ;
#22443 = FACE_OUTER_BOUND ( 'NONE', #6305, .T. ) ;
#22444 = PLANE ( 'NONE',  #3365 ) ;
#22446 = ORIENTED_EDGE ( 'NONE', *, *, #15402, .T. ) ;
#22445 = PLANE ( 'NONE',  #1007 ) ;
#22447 = ORIENTED_EDGE ( 'NONE', *, *, #18247, .F. ) ;
#22448 = DIRECTION ( 'NONE',  ( 0.2348860457809842095, 0.000000000000000000, -0.9720229140804107493 ) ) ;
#22449 = ADVANCED_FACE ( 'NONE', ( #2488 ), #26657, .T. ) ;
#22450 = FACE_OUTER_BOUND ( 'NONE', #40374, .T. ) ;
#22451 = AXIS2_PLACEMENT_3D ( 'NONE', #21044, #30155, #46203 ) ;
#22452 = AXIS2_PLACEMENT_3D ( 'NONE', #18660, #30727, #3393 ) ;
#22453 = VERTEX_POINT ( 'NONE', #50328 ) ;
#22454 = FACE_OUTER_BOUND ( 'NONE', #11117, .T. ) ;
#22455 = EDGE_LOOP ( 'NONE', ( #3925, #24707, #21539, #26779 ) ) ;
#22456 = CARTESIAN_POINT ( 'NONE',  ( -48.47912675150885065, -175.3837268820161057, 6.938893903907228378E-15 ) ) ;
#22457 = DIRECTION ( 'NONE',  ( -1.000000000000000000, -0.000000000000000000, 0.000000000000000000 ) ) ;
#22458 = AXIS2_PLACEMENT_3D ( 'NONE', #4098, #32719, #8293 ) ;
#22459 = ADVANCED_FACE ( 'NONE', ( #26904 ), #2732, .T. ) ;
#22460 = EDGE_CURVE ( 'NONE', #18213, #47040, #30081, .T. ) ;
#22461 = EDGE_CURVE ( 'NONE', #49313, #7901, #6181, .T. ) ;
#22462 = EDGE_CURVE ( 'NONE', #45033, #2959, #2226, .T. ) ;
#22463 = CARTESIAN_POINT ( 'NONE',  ( 66.42899531795131907, -193.5000000000000000, 49.20491319441622124 ) ) ;
#22464 = CARTESIAN_POINT ( 'NONE',  ( -167.4530144994566285, -183.6283474603465606, -34.94873081740328757 ) ) ;
#22465 = ORIENTED_EDGE ( 'NONE', *, *, #38782, .F. ) ;
#22466 = EDGE_LOOP ( 'NONE', ( #52000, #6414, #1530, #10809 ) ) ;
#22467 = EDGE_CURVE ( 'NONE', #4655, #21321, #22715, .T. ) ;
#22468 = ORIENTED_EDGE ( 'NONE', *, *, #6092, .F. ) ;
#22469 = FACE_OUTER_BOUND ( 'NONE', #50113, .T. ) ;
#22470 = CARTESIAN_POINT ( 'NONE',  ( -48.02249751411513756, -183.6283474603465606, -0.8896570909947397743 ) ) ;
#22471 = CIRCLE ( 'NONE', #14104, 60.00000000000000000 ) ;
#22472 = AXIS2_PLACEMENT_3D ( 'NONE', #40999, #40470, #5021 ) ;
#22473 = ADVANCED_FACE ( 'NONE', ( #22469 ), #14317, .T. ) ;
#22474 = EDGE_CURVE ( 'NONE', #15796, #17439, #11131, .T. ) ;
#22475 = VECTOR ( 'NONE', #26402, 999.9999999999998863 ) ;
#22476 = LINE ( 'NONE', #13801, #51409 ) ;
#22477 = DIRECTION ( 'NONE',  ( 1.000000000000000000, -0.000000000000000000, -0.000000000000000000 ) ) ;
#22478 = ORIENTED_EDGE ( 'NONE', *, *, #48652, .T. ) ;
#22479 = VECTOR ( 'NONE', #17397, 1000.000000000000000 ) ;
#22480 = ADVANCED_FACE ( 'NONE', ( #10365 ), #30860, .F. ) ;
#22481 = DIRECTION ( 'NONE',  ( -0.5586467658036594619, 0.000000000000000000, 0.8294056854501971054 ) ) ;
#22482 = EDGE_CURVE ( 'NONE', #18723, #5376, #28299, .T. ) ;
#22483 = AXIS2_PLACEMENT_3D ( 'NONE', #32020, #19420, #35442 ) ;
#22484 = ORIENTED_EDGE ( 'NONE', *, *, #3052, .T. ) ;
#22485 = ORIENTED_EDGE ( 'NONE', *, *, #1061, .F. ) ;
#22486 = EDGE_CURVE ( 'NONE', #37313, #23381, #14579, .T. ) ;
#22487 = DIRECTION ( 'NONE',  ( -0.8294056854502011022, 0.000000000000000000, -0.5586467658036535777 ) ) ;
#22488 = DIRECTION ( 'NONE',  ( -0.05924062789370006937, 0.000000000000000000, -0.9982437317643222396 ) ) ;
#22489 = EDGE_CURVE ( 'NONE', #48882, #30266, #46905, .T. ) ;
#22490 = DIRECTION ( 'NONE',  ( -0.000000000000000000, 1.000000000000000000, -0.000000000000000000 ) ) ;
#22491 = CARTESIAN_POINT ( 'NONE',  ( -140.1460956102404509, -175.3837268820161057, 84.98333260264821831 ) ) ;
#22492 = ORIENTED_EDGE ( 'NONE', *, *, #40415, .T. ) ;
#22493 = LINE ( 'NONE', #38508, #5780 ) ;
#22494 = EDGE_CURVE ( 'NONE', #13319, #37838, #22972, .T. ) ;
#22495 = EDGE_LOOP ( 'NONE', ( #34822, #15053, #43896, #31633 ) ) ;
#22496 = DIRECTION ( 'NONE',  ( 0.000000000000000000, -7.100801428331730794E-14, 1.000000000000000000 ) ) ;
#22497 = VECTOR ( 'NONE', #18282, 1000.000000000000000 ) ;
#22498 = VECTOR ( 'NONE', #24407, 1000.000000000000000 ) ;
#22499 = DIRECTION ( 'NONE',  ( -0.000000000000000000, 1.000000000000000000, 0.000000000000000000 ) ) ;
#22500 = ORIENTED_EDGE ( 'NONE', *, *, #9928, .T. ) ;
#22501 = CIRCLE ( 'NONE', #4032, 125.0000000000000000 ) ;
#22502 = DIRECTION ( 'NONE',  ( 0.4031234292879665171, 0.000000000000000000, 0.9151456172430210145 ) ) ;
#22503 = CARTESIAN_POINT ( 'NONE',  ( -98.10897907742933910, -189.7472609257535510, 114.7252272087849434 ) ) ;
#22504 = LINE ( 'NONE', #50102, #49757 ) ;
#22505 = DIRECTION ( 'NONE',  ( -1.000000000000000000, 0.000000000000000000, 8.718379230999707126E-17 ) ) ;
#22506 = EDGE_CURVE ( 'NONE', #15659, #6808, #51119, .T. ) ;
#22507 = DIRECTION ( 'NONE',  ( 0.000000000000000000, 0.000000000000000000, 1.000000000000000000 ) ) ;
#22508 = ORIENTED_EDGE ( 'NONE', *, *, #19277, .T. ) ;
#22509 = VECTOR ( 'NONE', #34771, 1000.000000000000000 ) ;
#22510 = DIRECTION ( 'NONE',  ( 0.000000000000000000, -0.7485107481710954191, 0.6631226582408017434 ) ) ;
#22511 = ORIENTED_EDGE ( 'NONE', *, *, #32294, .T. ) ;
#22512 = ORIENTED_EDGE ( 'NONE', *, *, #22093, .F. ) ;
#22513 = DIRECTION ( 'NONE',  ( 1.000000000000000000, 2.086444717177488260E-17, -8.465038975556413550E-17 ) ) ;
#22514 = ORIENTED_EDGE ( 'NONE', *, *, #24571, .F. ) ;
#22515 = VECTOR ( 'NONE', #4762, 1000.000000000000000 ) ;
#22516 = FACE_OUTER_BOUND ( 'NONE', #7640, .T. ) ;
#22517 = ORIENTED_EDGE ( 'NONE', *, *, #19428, .T. ) ;
#22518 = DIRECTION ( 'NONE',  ( 0.000000000000000000, 0.000000000000000000, -1.000000000000000000 ) ) ;
#22519 = LINE ( 'NONE', #6744, #4465 ) ;
#22520 = EDGE_LOOP ( 'NONE', ( #10430, #12701, #4999, #24317 ) ) ;
#22521 = CARTESIAN_POINT ( 'NONE',  ( -41.96187976958283627, -175.3837268820161057, -123.8286356280830205 ) ) ;
#22522 = EDGE_CURVE ( 'NONE', #35097, #11813, #14068, .T. ) ;
#22523 = EDGE_CURVE ( 'NONE', #40799, #38866, #7961, .T. ) ;
#22524 = DIRECTION ( 'NONE',  ( -1.000000000000000000, 0.000000000000000000, 0.000000000000000000 ) ) ;
#22525 = FACE_OUTER_BOUND ( 'NONE', #2600, .T. ) ;
#22526 = VERTEX_POINT ( 'NONE', #20056 ) ;
#22527 = EDGE_LOOP ( 'NONE', ( #33410, #51745, #25450, #33288 ) ) ;
#22528 = ORIENTED_EDGE ( 'NONE', *, *, #29837, .T. ) ;
#22529 = DIRECTION ( 'NONE',  ( -0.2920567706369628924, 0.000000000000000000, -0.9564009842765264224 ) ) ;
#22530 = VECTOR ( 'NONE', #5620, 1000.000000000000000 ) ;
#22531 = LINE ( 'NONE', #38546, #40255 ) ;
#22532 = CIRCLE ( 'NONE', #51910, 60.00000000000000000 ) ;
#22533 = VECTOR ( 'NONE', #40996, 1000.000000000000000 ) ;
#22534 = DIRECTION ( 'NONE',  ( 0.000000000000000000, -0.000000000000000000, 1.000000000000000000 ) ) ;
#22535 = CARTESIAN_POINT ( 'NONE',  ( -336.3521761649654422, -176.5004679656469477, -25.97334715265976612 ) ) ;
#22536 = CARTESIAN_POINT ( 'NONE',  ( -180.0000000000000568, -115.7896721143442278, -18.45401972188387418 ) ) ;
#22537 = EDGE_LOOP ( 'NONE', ( #38212, #37916, #51430, #22591 ) ) ;
#22538 = AXIS2_PLACEMENT_3D ( 'NONE', #21621, #851, #1892 ) ;
#22539 = DIRECTION ( 'NONE',  ( 0.000000000000000000, -1.000000000000000000, 0.000000000000000000 ) ) ;
#22540 = ORIENTED_EDGE ( 'NONE', *, *, #23560, .T. ) ;
#22542 = EDGE_LOOP ( 'NONE', ( #19281, #30040, #45330, #26334 ) ) ;
#22541 = LINE ( 'NONE', #14385, #5522 ) ;
#22543 = AXIS2_PLACEMENT_3D ( 'NONE', #29165, #45225, #21287 ) ;
#22544 = ORIENTED_EDGE ( 'NONE', *, *, #7912, .T. ) ;
#22545 = CARTESIAN_POINT ( 'NONE',  ( 63.54086012517504400, -189.7472609257535510, -53.17445600718541954 ) ) ;
#22546 = EDGE_CURVE ( 'NONE', #38453, #33832, #40267, .T. ) ;
#22547 = ORIENTED_EDGE ( 'NONE', *, *, #11561, .T. ) ;
#22548 = CARTESIAN_POINT ( 'NONE',  ( 59.29945538372744807, -177.1207230881787780, 63.31490529818492519 ) ) ;
#22549 = LINE ( 'NONE', #50155, #50650 ) ;
#22550 = CARTESIAN_POINT ( 'NONE',  ( -305.0000000000000568, -157.1712093821529947, 49.66134974749694209 ) ) ;
#22551 = ORIENTED_EDGE ( 'NONE', *, *, #42988, .T. ) ;
#22552 = CYLINDRICAL_SURFACE ( 'NONE', #689, 16.00000000000000000 ) ;
#22553 = ORIENTED_EDGE ( 'NONE', *, *, #41299, .F. ) ;
#22554 = EDGE_CURVE ( 'NONE', #39207, #50756, #41741, .T. ) ;
#22555 = AXIS2_PLACEMENT_3D ( 'NONE', #26203, #34104, #9418 ) ;
#22556 = ORIENTED_EDGE ( 'NONE', *, *, #21085, .T. ) ;
#22557 = DIRECTION ( 'NONE',  ( 0.000000000000000000, 0.000000000000000000, -1.000000000000000000 ) ) ;
#22558 = DIRECTION ( 'NONE',  ( -0.9646355819083556327, 0.000000000000000000, -0.2635871660690782825 ) ) ;
#22559 = DIRECTION ( 'NONE',  ( 0.7378332790417333475, 0.000000000000000000, -0.6749830015182038956 ) ) ;
#22560 = ORIENTED_EDGE ( 'NONE', *, *, #32645, .T. ) ;
#22561 = PLANE ( 'NONE',  #8303 ) ;
#22562 = CARTESIAN_POINT ( 'NONE',  ( -305.0000000000000568, -89.00580675195290326, 49.09328500076543378 ) ) ;
#22563 = CARTESIAN_POINT ( 'NONE',  ( -89.73513343757494454, -183.6283474603465606, -117.9955164924467397 ) ) ;
#22564 = CARTESIAN_POINT ( 'NONE',  ( 0.000000000000000000, -89.98417994286123189, 48.55604808772534398 ) ) ;
#22565 = EDGE_LOOP ( 'NONE', ( #12279, #9210, #33239, #49745, #23246, #29973, #796, #50408 ) ) ;
#22566 = CARTESIAN_POINT ( 'NONE',  ( -109.5001801941309338, -193.5000000000000000, -107.9473519284343155 ) ) ;
#22567 = DIRECTION ( 'NONE',  ( 0.000000000000000000, -0.000000000000000000, 1.000000000000000000 ) ) ;
#22568 = FACE_OUTER_BOUND ( 'NONE', #129, .T. ) ;
#22569 =( GEOMETRIC_REPRESENTATION_CONTEXT ( 3 ) GLOBAL_UNCERTAINTY_ASSIGNED_CONTEXT ( ( #14854 ) ) GLOBAL_UNIT_ASSIGNED_CONTEXT ( ( #6843, #42584, #10025 ) ) REPRESENTATION_CONTEXT ( 'NONE', 'WORKASPACE' ) );
#22570 = ORIENTED_EDGE ( 'NONE', *, *, #9578, .F. ) ;
#22571 = AXIS2_PLACEMENT_3D ( 'NONE', #4310, #8502, #12447 ) ;
#22572 = AXIS2_PLACEMENT_3D ( 'NONE', #16786, #28580, #29103 ) ;
#22573 = CARTESIAN_POINT ( 'NONE',  ( -171.7300019102062549, -177.1207230881787780, -20.83798868929510562 ) ) ;
#22574 = AXIS2_PLACEMENT_3D ( 'NONE', #44956, #40995, #9721 ) ;
#22575 = FACE_BOUND ( 'NONE', #5691, .T. ) ;
#22576 = VERTEX_POINT ( 'NONE', #4284 ) ;
#22577 = CARTESIAN_POINT ( 'NONE',  ( -332.3517673607765914, -123.5000000000000284, 0.000000000000000000 ) ) ;
#22578 = VERTEX_POINT ( 'NONE', #15875 ) ;
#22579 = AXIS2_PLACEMENT_3D ( 'NONE', #9397, #40924, #21995 ) ;
#22580 = DIRECTION ( 'NONE',  ( 1.000000000000000000, 3.091579882402645797E-17, 8.151826190875899055E-17 ) ) ;
#22581 = DIRECTION ( 'NONE',  ( 0.000000000000000000, 0.8229838658936556861, -0.5680647467311569221 ) ) ;
#22582 = DIRECTION ( 'NONE',  ( -0.7378332790417333475, 0.000000000000000000, 0.6749830015182038956 ) ) ;
#22583 = CARTESIAN_POINT ( 'NONE',  ( -77.43961373357959133, -189.7472609257535510, -120.5706864261535145 ) ) ;
#22584 = EDGE_CURVE ( 'NONE', #36852, #38638, #12424, .T. ) ;
#22585 = LINE ( 'NONE', #37575, #30210 ) ;
#22586 = VERTEX_POINT ( 'NONE', #51878 ) ;
#22587 = VECTOR ( 'NONE', #42500, 1000.000000000000000 ) ;
#22588 = CARTESIAN_POINT ( 'NONE',  ( 46.00000000000000000, 20.00000000000000000, 0.000000000000000000 ) ) ;
#22589 = ORIENTED_EDGE ( 'NONE', *, *, #39063, .F. ) ;
#22590 = DIRECTION ( 'NONE',  ( -0.8610436117673621048, 0.000000000000000000, 0.5085311186492095237 ) ) ;
#22591 = ORIENTED_EDGE ( 'NONE', *, *, #50643, .T. ) ;
#22592 = DIRECTION ( 'NONE',  ( -0.7765238627180437447, 0.000000000000000000, 0.6300878435817094392 ) ) ;
#22593 = DIRECTION ( 'NONE',  ( 0.000000000000000000, 0.000000000000000000, 1.000000000000000000 ) ) ;
#22594 = CARTESIAN_POINT ( 'NONE',  ( -336.3521761649654422, -178.0871407151310279, 22.44790492310219676 ) ) ;
#22595 = VERTEX_POINT ( 'NONE', #43714 ) ;
#22598 = ORIENTED_EDGE ( 'NONE', *, *, #29619, .T. ) ;
#22597 = LINE ( 'NONE', #18648, #39019 ) ;
#22596 = CARTESIAN_POINT ( 'NONE',  ( -4.460811323677677187, 53.88842563715992640, -18.70041964591998607 ) ) ;
#22599 = AXIS2_PLACEMENT_3D ( 'NONE', #6803, #11506, #27533 ) ;
#22600 = EDGE_CURVE ( 'NONE', #36650, #35348, #12152, .T. ) ;
#22601 = FACE_OUTER_BOUND ( 'NONE', #39089, .T. ) ;
#22602 = ORIENTED_EDGE ( 'NONE', *, *, #5432, .T. ) ;
#22603 = CARTESIAN_POINT ( 'NONE',  ( -48.47912675150885065, -175.3837268820161057, 6.938893903907228378E-15 ) ) ;
#22604 = VECTOR ( 'NONE', #10167, 1000.000000000000000 ) ;
#22605 = ORIENTED_EDGE ( 'NONE', *, *, #19828, .F. ) ;
#22606 = CARTESIAN_POINT ( 'NONE',  ( 22.73247662810271308, -177.1207230881787780, -101.5140743725395254 ) ) ;
#22609 = ORIENTED_EDGE ( 'NONE', *, *, #32930, .F. ) ;
#22608 = CARTESIAN_POINT ( 'NONE',  ( -48.47912675150885065, -183.6283474603465606, 6.938893903907228378E-15 ) ) ;
#22607 = CARTESIAN_POINT ( 'NONE',  ( -280.0000000000000000, -153.5000000000000284, -59.99999999999999289 ) ) ;
#22610 = ORIENTED_EDGE ( 'NONE', *, *, #5735, .F. ) ;
#22611 = DIRECTION ( 'NONE',  ( 0.9785564922995017012, 0.000000000000000000, 0.2059786187411094538 ) ) ;
#22612 = ORIENTED_EDGE ( 'NONE', *, *, #28833, .T. ) ;
#22613 = CARTESIAN_POINT ( 'NONE',  ( -156.7610986364826999, -177.1207230881787780, -62.45009659481509345 ) ) ;
#22614 = DIRECTION ( 'NONE',  ( 0.8757349421956345248, 0.000000000000000000, 0.4827922027307490205 ) ) ;
#22615 = ORIENTED_EDGE ( 'NONE', *, *, #15210, .T. ) ;
#22616 = CARTESIAN_POINT ( 'NONE',  ( -339.1964088526558498, -116.8846903019852164, -58.63009191191289915 ) ) ;
#22617 = DIRECTION ( 'NONE',  ( 0.000000000000000000, -1.000000000000000000, 0.000000000000000000 ) ) ;
#22618 = FACE_OUTER_BOUND ( 'NONE', #42771, .T. ) ;
#22619 = DIRECTION ( 'NONE',  ( -0.000000000000000000, 1.000000000000000000, -0.000000000000000000 ) ) ;
#22620 = CARTESIAN_POINT ( 'NONE',  ( -43.48323084606168720, -183.6283474603465606, 124.9001241957026167 ) ) ;
#22621 = ORIENTED_EDGE ( 'NONE', *, *, #42085, .F. ) ;
#22622 = EDGE_CURVE ( 'NONE', #26421, #17429, #40529, .T. ) ;
#22623 = DIRECTION ( 'NONE',  ( -0.000000000000000000, 1.000000000000000000, -0.000000000000000000 ) ) ;
#22624 = LINE ( 'NONE', #50741, #5542 ) ;
#22625 = AXIS2_PLACEMENT_3D ( 'NONE', #42172, #6195, #17244 ) ;
#22626 = DIRECTION ( 'NONE',  ( -0.000000000000000000, -0.3546048870425267951, 0.9350162426854181641 ) ) ;
#22627 = ORIENTED_EDGE ( 'NONE', *, *, #23490, .T. ) ;
#22628 = CARTESIAN_POINT ( 'NONE',  ( 28.62116745695382392, -177.1207230881787780, -97.11716833071837129 ) ) ;
#22629 = CARTESIAN_POINT ( 'NONE',  ( -336.3521761649654422, -182.5000000000000568, 2.632288850093980503 ) ) ;
#22630 = DIRECTION ( 'NONE',  ( 0.000000000000000000, 0.000000000000000000, -1.000000000000000000 ) ) ;
#22631 = EDGE_CURVE ( 'NONE', #35575, #16039, #24510, .T. ) ;
#22632 = LINE ( 'NONE', #10797, #50149 ) ;
#22633 = EDGE_LOOP ( 'NONE', ( #46605, #2991, #2436, #29898 ) ) ;
#22634 = EDGE_CURVE ( 'NONE', #24439, #26043, #31883, .T. ) ;
#22635 = AXIS2_PLACEMENT_3D ( 'NONE', #43818, #48031, #12012 ) ;
#22636 = DIRECTION ( 'NONE',  ( 1.000000000000000000, 0.000000000000000000, -0.000000000000000000 ) ) ;
#22637 = FACE_OUTER_BOUND ( 'NONE', #36855, .T. ) ;
#22638 = AXIS2_PLACEMENT_3D ( 'NONE', #25755, #33635, #4747 ) ;
#22639 = VERTEX_POINT ( 'NONE', #7469 ) ;
#22640 = EDGE_CURVE ( 'NONE', #43567, #41906, #24119, .T. ) ;
#22641 = LINE ( 'NONE', #5130, #5049 ) ;
#22642 = EDGE_CURVE ( 'NONE', #45491, #43537, #15350, .T. ) ;
#22643 = CARTESIAN_POINT ( 'NONE',  ( -0.3054481938615447034, -183.6283474603465606, 115.3442529744090592 ) ) ;
#22644 = EDGE_LOOP ( 'NONE', ( #33222, #7392, #29575, #33802 ) ) ;
#22645 = ORIENTED_EDGE ( 'NONE', *, *, #32772, .F. ) ;
#22646 = ADVANCED_FACE ( 'NONE', ( #24265 ), #11901, .F. ) ;
#22647 = ORIENTED_EDGE ( 'NONE', *, *, #25952, .T. ) ;
#22648 = DIRECTION ( 'NONE',  ( 0.000000000000000000, 0.000000000000000000, -1.000000000000000000 ) ) ;
#22649 = LINE ( 'NONE', #39185, #42948 ) ;
#22650 = LINE ( 'NONE', #38662, #48168 ) ;
#22651 = VERTEX_POINT ( 'NONE', #15609 ) ;
#22652 = AXIS2_PLACEMENT_3D ( 'NONE', #50638, #38274, #42215 ) ;
#22653 = AXIS2_PLACEMENT_3D ( 'NONE', #50310, #18750, #22176 ) ;
#22654 = DIRECTION ( 'NONE',  ( -0.000000000000000000, 1.000000000000000000, -0.000000000000000000 ) ) ;
#22655 = DIRECTION ( 'NONE',  ( 0.000000000000000000, 0.2393156642875615969, 0.9709418174260511236 ) ) ;
#22658 = ORIENTED_EDGE ( 'NONE', *, *, #4429, .F. ) ;
#22657 = CARTESIAN_POINT ( 'NONE',  ( -98.71382891444390850, -189.7472609257535510, -114.4616734920523839 ) ) ;
#22656 = DIRECTION ( 'NONE',  ( -0.000000000000000000, 1.000000000000000000, -0.000000000000000000 ) ) ;
#22659 = EDGE_CURVE ( 'NONE', #32832, #13489, #30822, .T. ) ;
#22660 = DIRECTION ( 'NONE',  ( 1.000000000000000000, -0.000000000000000000, -0.000000000000000000 ) ) ;
#22661 = EDGE_LOOP ( 'NONE', ( #6585, #7654, #4357, #31748 ) ) ;
#22662 = DIRECTION ( 'NONE',  ( 0.000000000000000000, 0.000000000000000000, -1.000000000000000000 ) ) ;
#22663 = ORIENTED_EDGE ( 'NONE', *, *, #15111, .F. ) ;
#22664 = PLANE ( 'NONE',  #27441 ) ;
#22665 = DIRECTION ( 'NONE',  ( -0.000000000000000000, 1.000000000000000000, -0.000000000000000000 ) ) ;
#22666 = CARTESIAN_POINT ( 'NONE',  ( -91.49662025983752756, -175.3837268820161057, -116.2991637277475405 ) ) ;
#22667 = ORIENTED_EDGE ( 'NONE', *, *, #7472, .F. ) ;
#22668 = ORIENTED_EDGE ( 'NONE', *, *, #46933, .F. ) ;
#22669 = PLANE ( 'NONE',  #14769 ) ;
#22671 = AXIS2_PLACEMENT_3D ( 'NONE', #11581, #19220, #27342 ) ;
#22670 = CARTESIAN_POINT ( 'NONE',  ( -94.25732089370191602, -193.5000000000000000, 116.3157639405754935 ) ) ;
#22672 = ORIENTED_EDGE ( 'NONE', *, *, #7668, .T. ) ;
#22673 = DIRECTION ( 'NONE',  ( -0.000000000000000000, 1.000000000000000000, -0.000000000000000000 ) ) ;
#22674 = CARTESIAN_POINT ( 'NONE',  ( -129.9529520667707914, -193.5000000000000000, -94.79987230211959570 ) ) ;
#22675 = ORIENTED_EDGE ( 'NONE', *, *, #8310, .F. ) ;
#22676 = FACE_BOUND ( 'NONE', #31931, .T. ) ;
#22677 = CARTESIAN_POINT ( 'NONE',  ( -48.47912675150885065, -189.7472609257535510, 124.0000000000000142 ) ) ;
#22678 = PRODUCT_DEFINITION_SHAPE ( 'NONE', 'NONE',  #52047 ) ;
#22679 = VERTEX_POINT ( 'NONE', #8477 ) ;
#22680 = CARTESIAN_POINT ( 'NONE',  ( 28.62116745695382392, -183.6283474603465606, -97.11716833071837129 ) ) ;
#22681 = ORIENTED_EDGE ( 'NONE', *, *, #3632, .F. ) ;
#22682 = LINE ( 'NONE', #15574, #28126 ) ;
#22683 = CARTESIAN_POINT ( 'NONE',  ( 141.7825277784304205, -213.5000000000000000, 10.00000000000000178 ) ) ;
#22684 = ORIENTED_EDGE ( 'NONE', *, *, #385, .T. ) ;
#22685 = DIRECTION ( 'NONE',  ( -0.000000000000000000, 1.000000000000000000, -0.000000000000000000 ) ) ;
#22686 = ADVANCED_FACE ( 'NONE', ( #47405 ), #11385, .T. ) ;
#22687 = CARTESIAN_POINT ( 'NONE',  ( -48.64924157374594671, -175.3837268820161057, 124.9998842437354227 ) ) ;
#22688 = DIRECTION ( 'NONE',  ( 1.000000000000000000, 0.000000000000000000, 0.000000000000000000 ) ) ;
#22689 = EDGE_CURVE ( 'NONE', #38924, #13962, #27935, .T. ) ;
#22690 = VERTEX_POINT ( 'NONE', #48183 ) ;
#22691 = CIRCLE ( 'NONE', #16845, 60.00000000000000000 ) ;
#22692 = PLANE ( 'NONE',  #40501 ) ;
#22693 = DIRECTION ( 'NONE',  ( -0.5085311186492154079, 0.000000000000000000, -0.8610436117673585521 ) ) ;
#22694 = DIRECTION ( 'NONE',  ( -1.000000000000000000, -0.000000000000000000, -0.000000000000000000 ) ) ;
#22696 = ORIENTED_EDGE ( 'NONE', *, *, #15396, .F. ) ;
#22695 = FACE_OUTER_BOUND ( 'NONE', #25747, .T. ) ;
#22697 = VERTEX_POINT ( 'NONE', #3505 ) ;
#22698 = LINE ( 'NONE', #2717, #2273 ) ;
#22699 = ADVANCED_FACE ( 'NONE', ( #3763 ), #11658, .T. ) ;
#22700 = EDGE_CURVE ( 'NONE', #17498, #12667, #40012, .T. ) ;
#22701 = CARTESIAN_POINT ( 'NONE',  ( -48.47912675150885065, -177.1207230881787780, 6.938893903907228378E-15 ) ) ;
#22702 = ORIENTED_EDGE ( 'NONE', *, *, #43042, .F. ) ;
#22703 = EDGE_CURVE ( 'NONE', #29336, #51798, #12675, .T. ) ;
#22704 = VECTOR ( 'NONE', #41955, 1000.000000000000000 ) ;
#22705 = DIRECTION ( 'NONE',  ( 0.000000000000000000, -0.4647231720437755564, -0.8854560256532062468 ) ) ;
#22706 = ORIENTED_EDGE ( 'NONE', *, *, #24677, .T. ) ;
#22707 = DIRECTION ( 'NONE',  ( -0.000000000000000000, 0.2393156642875685636, 0.9709418174260492362 ) ) ;
#22708 = LINE ( 'NONE', #46632, #19970 ) ;
#22709 = EDGE_CURVE ( 'NONE', #44232, #27933, #48703, .T. ) ;
#22710 = DIRECTION ( 'NONE',  ( 0.000000000000000000, -1.000000000000000000, 0.000000000000000000 ) ) ;
#22711 = DIRECTION ( 'NONE',  ( 0.000000000000000000, 0.000000000000000000, -1.000000000000000000 ) ) ;
#22712 = ORIENTED_EDGE ( 'NONE', *, *, #32867, .T. ) ;
#22713 = ORIENTED_EDGE ( 'NONE', *, *, #24495, .T. ) ;
#22714 = VERTEX_POINT ( 'NONE', #24775 ) ;
#22715 = LINE ( 'NONE', #7202, #23289 ) ;
#22716 = CARTESIAN_POINT ( 'NONE',  ( -127.0132498732366457, -183.6283474603465606, 97.24912084693259828 ) ) ;
#22717 = DIRECTION ( 'NONE',  ( 0.000000000000000000, 0.000000000000000000, -1.000000000000000000 ) ) ;
#22718 = LINE ( 'NONE', #18007, #7933 ) ;
#22719 = ORIENTED_EDGE ( 'NONE', *, *, #19703, .F. ) ;
#22720 = AXIS2_PLACEMENT_3D ( 'NONE', #44785, #36637, #44270 ) ;
#22721 = UNCERTAINTY_MEASURE_WITH_UNIT (LENGTH_MEASURE( 1.000000000000000082E-05 ), #29615, 'distance_accuracy_value', 'NONE');
#22722 = CYLINDRICAL_SURFACE ( 'NONE', #24828, 9.999999999999994671 ) ;
#22723 = CARTESIAN_POINT ( 'NONE',  ( 73.87536152799695799, -175.3837268820161057, -25.58083653558413317 ) ) ;
#22724 = CIRCLE ( 'NONE', #29422, 125.0000000000000000 ) ;
#22725 = AXIS2_PLACEMENT_3D ( 'NONE', #27328, #3671, #35464 ) ;
#22726 = EDGE_LOOP ( 'NONE', ( #51446, #1725, #5536, #33067 ) ) ;
#22727 = ORIENTED_EDGE ( 'NONE', *, *, #32365, .T. ) ;
#22728 = FACE_OUTER_BOUND ( 'NONE', #48908, .T. ) ;
#22729 = FACE_OUTER_BOUND ( 'NONE', #7876, .T. ) ;
#22730 = CARTESIAN_POINT ( 'NONE',  ( -47.51449116960048968, -177.1207230881787780, 0.2635871660690785045 ) ) ;
#22731 = LINE ( 'NONE', #14080, #26661 ) ;
#22732 = CARTESIAN_POINT ( 'NONE',  ( 72.35619569422321717, -177.1207230881787780, 27.83926365844748574 ) ) ;
#22733 = CARTESIAN_POINT ( 'NONE',  ( -180.0000000000000568, -115.7896721143442278, 18.45401972188388839 ) ) ;
#22734 = VERTEX_POINT ( 'NONE', #16653 ) ;
#22735 = CARTESIAN_POINT ( 'NONE',  ( -48.71401279728982558, -183.6283474603465606, -0.9720229140804069745 ) ) ;
#22736 = ADVANCED_FACE ( 'NONE', ( #28698 ), #20570, .F. ) ;
#22737 = VERTEX_POINT ( 'NONE', #2283 ) ;
#22738 = LINE ( 'NONE', #18792, #22901 ) ;
#22739 = VECTOR ( 'NONE', #6498, 1000.000000000000000 ) ;
#22740 = CARTESIAN_POINT ( 'NONE',  ( -332.3517673607765914, -114.7679482383557144, 58.37307289257701370 ) ) ;
#22741 = EDGE_LOOP ( 'NONE', ( #38498, #26910, #897, #8417 ) ) ;
#22742 = EDGE_CURVE ( 'NONE', #25920, #33208, #18814, .T. ) ;
#22743 = DIRECTION ( 'NONE',  ( 0.000000000000000000, -1.000000000000000000, 0.000000000000000000 ) ) ;
#22744 = ADVANCED_FACE ( 'NONE', ( #14119 ), #18319, .T. ) ;
#22745 = DIRECTION ( 'NONE',  ( -0.000000000000000000, -1.000000000000000000, -0.000000000000000000 ) ) ;
#22746 = DIRECTION ( 'NONE',  ( 0.000000000000000000, 0.000000000000000000, 1.000000000000000000 ) ) ;
#22747 = EDGE_CURVE ( 'NONE', #5970, #19616, #31160, .T. ) ;
#22748 = LINE ( 'NONE', #6210, #16487 ) ;
#22749 = EDGE_CURVE ( 'NONE', #4422, #16821, #42206, .T. ) ;
#22750 = DIRECTION ( 'NONE',  ( -0.000000000000000000, 1.000000000000000000, -0.000000000000000000 ) ) ;
#22751 = ORIENTED_EDGE ( 'NONE', *, *, #34535, .F. ) ;
#22752 = ADVANCED_FACE ( 'NONE', ( #35107 ), #47212, .T. ) ;
#22753 = CARTESIAN_POINT ( 'NONE',  ( -168.4003408533108086, -193.5000000000000000, -35.26900067126609173 ) ) ;
#22755 = ORIENTED_EDGE ( 'NONE', *, *, #15359, .F. ) ;
#22754 = LINE ( 'NONE', #45710, #43882 ) ;
#22756 = AXIS2_PLACEMENT_3D ( 'NONE', #41034, #40503, #48677 ) ;
#22757 = ORIENTED_EDGE ( 'NONE', *, *, #17296, .F. ) ;
#22758 = PLANE ( 'NONE',  #6174 ) ;
#22759 = ADVANCED_FACE ( 'NONE', ( #42742 ), #38265, .F. ) ;
#22760 = VERTEX_POINT ( 'NONE', #51167 ) ;
#22761 = ADVANCED_FACE ( 'NONE', ( #14365 ), #34073, .T. ) ;
#22762 = AXIS2_PLACEMENT_3D ( 'NONE', #38960, #2969, #35037 ) ;
#22763 = LINE ( 'NONE', #39547, #45308 ) ;
#22764 = ORIENTED_EDGE ( 'NONE', *, *, #38871, .F. ) ;
#22765 = ADVANCED_FACE ( 'NONE', ( #34578 ), #30911, .F. ) ;
#22766 = CARTESIAN_POINT ( 'NONE',  ( 46.00000000000000711, 35.00000000000000000, -46.00000000000000000 ) ) ;
#22767 = CARTESIAN_POINT ( 'NONE',  ( 40.30419662299490113, -183.6283474603465606, -87.99159897727903967 ) ) ;
#22768 = ORIENTED_EDGE ( 'NONE', *, *, #41552, .T. ) ;
#22769 = LINE ( 'NONE', #10935, #29124 ) ;
#22770 = EDGE_CURVE ( 'NONE', #14709, #24601, #50894, .T. ) ;
#22771 = FACE_OUTER_BOUND ( 'NONE', #34566, .T. ) ;
#22772 = LINE ( 'NONE', #38781, #24087 ) ;
#22773 = VERTEX_POINT ( 'NONE', #3045 ) ;
#22774 = ORIENTED_EDGE ( 'NONE', *, *, #48828, .F. ) ;
#22775 = EDGE_CURVE ( 'NONE', #29888, #18768, #51802, .T. ) ;
#22776 = VERTEX_POINT ( 'NONE', #26708 ) ;
#22777 = DIRECTION ( 'NONE',  ( 0.000000000000000000, -1.000000000000000000, 0.000000000000000000 ) ) ;
#22778 = LINE ( 'NONE', #2793, #14254 ) ;
#22779 = AXIS2_PLACEMENT_3D ( 'NONE', #46065, #21622, #45289 ) ;
#22780 = DIRECTION ( 'NONE',  ( -0.000000000000000000, 0.9350162426854107256, -0.3546048870425463906 ) ) ;
#22781 = DIRECTION ( 'NONE',  ( 0.000000000000000000, 0.000000000000000000, 1.000000000000000000 ) ) ;
#22782 = PLANE ( 'NONE',  #43166 ) ;
#22783 = ORIENTED_EDGE ( 'NONE', *, *, #11179, .F. ) ;
#22784 = ADVANCED_FACE ( 'NONE', ( #10412 ), #23295, .T. ) ;
#22785 = CARTESIAN_POINT ( 'NONE',  ( -48.13092511607445800, -193.5000000000000000, 0.9374196611341301111 ) ) ;
#22786 = ORIENTED_EDGE ( 'NONE', *, *, #18307, .F. ) ;
#22788 = EDGE_LOOP ( 'NONE', ( #44496, #3963, #34931, #36031 ) ) ;
#22787 = DIRECTION ( 'NONE',  ( -0.000000000000000000, 1.000000000000000000, -0.000000000000000000 ) ) ;
#22789 = VERTEX_POINT ( 'NONE', #22521 ) ;
#22790 = CARTESIAN_POINT ( 'NONE',  ( -48.77118352214583297, -175.3837268820161057, 0.9564009842765270886 ) ) ;
#22791 = DIRECTION ( 'NONE',  ( 0.9960498426152171181, 0.000000000000000000, -0.08879589532293157006 ) ) ;
#22792 = CIRCLE ( 'NONE', #12683, 125.0000000000000000 ) ;
#22793 = DIRECTION ( 'NONE',  ( 0.2348860457809775482, 0.000000000000000000, 0.9720229140804121926 ) ) ;
#22794 = FACE_OUTER_BOUND ( 'NONE', #41944, .T. ) ;
#22795 = ORIENTED_EDGE ( 'NONE', *, *, #37697, .F. ) ;
#22796 = CARTESIAN_POINT ( 'NONE',  ( 0.000000000000000000, -102.5783116644905562, -55.16595831843955722 ) ) ;
#22797 = VECTOR ( 'NONE', #21448, 1000.000000000000000 ) ;
#22798 = ORIENTED_EDGE ( 'NONE', *, *, #37705, .F. ) ;
#22799 = AXIS2_PLACEMENT_3D ( 'NONE', #44733, #37095, #41293 ) ;
#22800 = VERTEX_POINT ( 'NONE', #38538 ) ;
#22801 = CARTESIAN_POINT ( 'NONE',  ( -130.0559183202350084, -189.7472609257535510, -93.38753978496592367 ) ) ;
#22802 = CARTESIAN_POINT ( 'NONE',  ( -339.1964088526558498, -150.4759391377552618, 52.47426709956155122 ) ) ;
#22803 = CARTESIAN_POINT ( 'NONE',  ( 0.000000000000000000, -64.50000000000000000, 0.000000000000000000 ) ) ;
#22804 = VERTEX_POINT ( 'NONE', #39034 ) ;
#22805 = DIRECTION ( 'NONE',  ( -0.3758275821142357809, 0.000000000000000000, -0.9266896074318343723 ) ) ;
#22806 = CARTESIAN_POINT ( 'NONE',  ( -52.47502265695602119, -193.5000000000000000, -124.9361149384469485 ) ) ;
#22807 = EDGE_CURVE ( 'NONE', #27872, #48164, #619, .T. ) ;
#22808 = EDGE_CURVE ( 'NONE', #44107, #47366, #22769, .T. ) ;
#22809 = CARTESIAN_POINT ( 'NONE',  ( -339.1964088526558498, -84.75001853787875916, -44.49369547121548862 ) ) ;
#22810 = DIRECTION ( 'NONE',  ( -0.000000000000000000, 1.000000000000000000, -0.000000000000000000 ) ) ;
#22811 = ORIENTED_EDGE ( 'NONE', *, *, #14816, .T. ) ;
#22812 = DIRECTION ( 'NONE',  ( -0.000000000000000000, 0.8229838658936494689, -0.5680647467311658039 ) ) ;
#22813 = DIRECTION ( 'NONE',  ( -0.000000000000000000, 1.000000000000000000, -0.000000000000000000 ) ) ;
#22814 = AXIS2_PLACEMENT_3D ( 'NONE', #16431, #8522, #12719 ) ;
#22815 = EDGE_CURVE ( 'NONE', #32799, #39057, #38779, .T. ) ;
#22816 = EDGE_CURVE ( 'NONE', #25410, #3029, #14900, .T. ) ;
#22817 = FACE_BOUND ( 'NONE', #45239, .T. ) ;
#22818 = ORIENTED_EDGE ( 'NONE', *, *, #19038, .F. ) ;
#22819 = AXIS2_PLACEMENT_3D ( 'NONE', #27350, #11060, #2423 ) ;
#22820 = DIRECTION ( 'NONE',  ( 0.000000000000000000, 1.000000000000000000, -0.000000000000000000 ) ) ;
#22821 = CARTESIAN_POINT ( 'NONE',  ( 70.98542830588607444, -183.6283474603465606, -36.78613984829962646 ) ) ;
#22822 = VERTEX_POINT ( 'NONE', #43764 ) ;
#22823 = DIRECTION ( 'NONE',  ( 0.000000000000000000, 0.000000000000000000, 1.000000000000000000 ) ) ;
#22824 = VERTEX_POINT ( 'NONE', #3562 ) ;
#22825 = DIRECTION ( 'NONE',  ( 0.000000000000000000, 1.000000000000000000, -0.000000000000000000 ) ) ;
#22826 = ADVANCED_FACE ( 'NONE', ( #24318 ), #35358, .T. ) ;
#22827 = FACE_OUTER_BOUND ( 'NONE', #6656, .T. ) ;
#22828 = LINE ( 'NONE', #14433, #27931 ) ;
#22829 = VECTOR ( 'NONE', #46025, 1000.000000000000000 ) ;
#22830 = AXIS2_PLACEMENT_3D ( 'NONE', #34500, #14287, #5636 ) ;
#22831 = CARTESIAN_POINT ( 'NONE',  ( -51.89154260666836649, -193.5000000000000000, 124.9534129907280828 ) ) ;
#22832 = VERTEX_POINT ( 'NONE', #19853 ) ;
#22833 = EDGE_CURVE ( 'NONE', #3183, #42659, #35062, .T. ) ;
#22834 = VECTOR ( 'NONE', #29220, 1000.000000000000000 ) ;
#22835 = ORIENTED_EDGE ( 'NONE', *, *, #10288, .T. ) ;
#22836 = DIRECTION ( 'NONE',  ( 0.000000000000000000, 0.000000000000000000, -1.000000000000000000 ) ) ;
#22837 = VERTEX_POINT ( 'NONE', #19592 ) ;
#22838 = CARTESIAN_POINT ( 'NONE',  ( -332.3517673607765914, -123.5000000000000284, 0.000000000000000000 ) ) ;
#22839 = VECTOR ( 'NONE', #12921, 1000.000000000000000 ) ;
#22840 = FACE_OUTER_BOUND ( 'NONE', #48924, .T. ) ;
#22841 = DIRECTION ( 'NONE',  ( 0.000000000000000000, 1.000000000000000000, 0.000000000000000000 ) ) ;
#22842 = ORIENTED_EDGE ( 'NONE', *, *, #49242, .T. ) ;
#22845 = ORIENTED_EDGE ( 'NONE', *, *, #8944, .T. ) ;
#22844 = LINE ( 'NONE', #35967, #12155 ) ;
#22843 = CARTESIAN_POINT ( 'NONE',  ( -332.3517673607765914, -152.3639871485048900, -51.48334306143194539 ) ) ;
#22846 = AXIS2_PLACEMENT_3D ( 'NONE', #9519, #42342, #10045 ) ;
#22847 = AXIS2_PLACEMENT_3D ( 'NONE', #8481, #40534, #24781 ) ;
#22848 = FACE_OUTER_BOUND ( 'NONE', #47129, .T. ) ;
#22849 = ORIENTED_EDGE ( 'NONE', *, *, #2816, .F. ) ;
#22850 = CARTESIAN_POINT ( 'NONE',  ( -11.80936624585915418, -193.5000000000000000, -119.5003291395395735 ) ) ;
#22851 = ORIENTED_EDGE ( 'NONE', *, *, #49983, .T. ) ;
#22852 = EDGE_CURVE ( 'NONE', #41498, #26525, #32460, .T. ) ;
#22853 = CARTESIAN_POINT ( 'NONE',  ( -8.169009709621407822, -177.1207230881787780, 118.3219948448695504 ) ) ;
#22854 = ORIENTED_EDGE ( 'NONE', *, *, #29793, .T. ) ;
#22857 = EDGE_LOOP ( 'NONE', ( #5955, #39108, #6665, #36875 ) ) ;
#22856 = CARTESIAN_POINT ( 'NONE',  ( 11.66870402553033337, -177.1207230881787780, 108.4360005853211248 ) ) ;
#22855 = LINE ( 'NONE', #34926, #8138 ) ;
#22858 = ORIENTED_EDGE ( 'NONE', *, *, #20147, .F. ) ;
#22859 = CARTESIAN_POINT ( 'NONE',  ( -102.9981419485577590, -183.6283474603465606, -111.3726929437936377 ) ) ;
#22860 = VERTEX_POINT ( 'NONE', #39552 ) ;
#22861 = CARTESIAN_POINT ( 'NONE',  ( 0.000000000000000000, -182.0698235717852924, -7.111664135063673342 ) ) ;
#22862 = LINE ( 'NONE', #31002, #24846 ) ;
#22863 = ORIENTED_EDGE ( 'NONE', *, *, #16291, .T. ) ;
#22864 = DIRECTION ( 'NONE',  ( -1.000000000000000000, 0.000000000000000000, 0.000000000000000000 ) ) ;
#22865 = PLANE ( 'NONE',  #22352 ) ;
#22866 = DIRECTION ( 'NONE',  ( 0.000000000000000000, 0.000000000000000000, 1.000000000000000000 ) ) ;
#22867 = DIRECTION ( 'NONE',  ( -0.7765238627180349740, 0.000000000000000000, -0.6300878435817203194 ) ) ;
#22868 = ORIENTED_EDGE ( 'NONE', *, *, #34821, .F. ) ;
#22869 = EDGE_CURVE ( 'NONE', #24091, #49425, #133, .T. ) ;
#22870 = EDGE_CURVE ( 'NONE', #8427, #39351, #12391, .T. ) ;
#22871 = FACE_OUTER_BOUND ( 'NONE', #15634, .T. ) ;
#22872 = DIRECTION ( 'NONE',  ( 0.000000000000000000, -1.000000000000000000, 0.000000000000000000 ) ) ;
#22873 = VECTOR ( 'NONE', #1881, 999.9999999999998863 ) ;
#22874 = CARTESIAN_POINT ( 'NONE',  ( 46.40005841627164074, -193.5000000000000000, 81.38144888055276738 ) ) ;
#22875 = ORIENTED_EDGE ( 'NONE', *, *, #5580, .T. ) ;
#22876 = DIRECTION ( 'NONE',  ( 0.000000000000000000, -1.000000000000000000, 0.000000000000000000 ) ) ;
#22877 = CARTESIAN_POINT ( 'NONE',  ( -332.3517673607765914, -113.7752393642576720, 58.25253621232167944 ) ) ;
#22878 = CARTESIAN_POINT ( 'NONE',  ( -339.1964088526558498, -180.6659093959934523, -14.60509510167853264 ) ) ;
#22879 = DIRECTION ( 'NONE',  ( 0.9890401873221633666, 0.000000000000000000, 0.1476465640024850756 ) ) ;
#22880 = DIRECTION ( 'NONE',  ( 0.000000000000000000, 0.7071067811865479058, 0.7071067811865472397 ) ) ;
#22881 = VERTEX_POINT ( 'NONE', #35886 ) ;
#22882 = CIRCLE ( 'NONE', #203, 125.0000000000000000 ) ;
#22883 = VECTOR ( 'NONE', #44778, 1000.000000000000000 ) ;
#22884 = AXIS2_PLACEMENT_3D ( 'NONE', #15713, #31458, #39346 ) ;
#22885 = DIRECTION ( 'NONE',  ( 0.000000000000000000, 1.000000000000000000, -0.000000000000000000 ) ) ;
#22886 = AXIS2_PLACEMENT_3D ( 'NONE', #5904, #45836, #38705 ) ;
#22887 = PLANE ( 'NONE',  #11433 ) ;
#22888 = CARTESIAN_POINT ( 'NONE',  ( -173.1763543514842070, -177.1207230881787780, 8.694908215728892387 ) ) ;
#22889 = ADVANCED_FACE ( 'NONE', ( #51668 ), #15410, .F. ) ;
#22890 = DIRECTION ( 'NONE',  ( 0.000000000000000000, 0.000000000000000000, -1.000000000000000000 ) ) ;
#22891 = DIRECTION ( 'NONE',  ( 0.000000000000000000, -1.000000000000000000, 0.000000000000000000 ) ) ;
#22892 = EDGE_LOOP ( 'NONE', ( #24867, #20346, #37245, #5466 ) ) ;
#22893 = VECTOR ( 'NONE', #12009, 1000.000000000000000 ) ;
#22894 = LINE ( 'NONE', #47333, #41119 ) ;
#22895 = EDGE_CURVE ( 'NONE', #34569, #49741, #36391, .T. ) ;
#22896 = CARTESIAN_POINT ( 'NONE',  ( -4.794493649713349015, -175.3837268820161057, -117.1181148702518726 ) ) ;
#22897 = EDGE_LOOP ( 'NONE', ( #39908, #7767, #7400, #34392 ) ) ;
#22898 = ORIENTED_EDGE ( 'NONE', *, *, #5434, .F. ) ;
#22899 = ORIENTED_EDGE ( 'NONE', *, *, #493, .F. ) ;
#22900 = LINE ( 'NONE', #46828, #43495 ) ;
#22901 = VECTOR ( 'NONE', #34803, 1000.000000000000000 ) ;
#22902 = EDGE_CURVE ( 'NONE', #18461, #49438, #22471, .T. ) ;
#22903 = CARTESIAN_POINT ( 'NONE',  ( -48.71401279728982558, -175.3837268820161057, -0.9720229140804069745 ) ) ;
#22904 = CARTESIAN_POINT ( 'NONE',  ( -18.95304271317703382, -175.3837268820161057, -121.4627941443854837 ) ) ;
#22905 = EDGE_LOOP ( 'NONE', ( #39440, #14276, #22560, #32048 ) ) ;
#22906 = VECTOR ( 'NONE', #9579, 1000.000000000000000 ) ;
#22907 = FACE_OUTER_BOUND ( 'NONE', #19936, .T. ) ;
#22908 = DIRECTION ( 'NONE',  ( 0.5586467658036415873, 0.000000000000000000, 0.8294056854502090959 ) ) ;
#22911 = ORIENTED_EDGE ( 'NONE', *, *, #12673, .T. ) ;
#22910 = CARTESIAN_POINT ( 'NONE',  ( 76.09804998693969935, -193.5000000000000000, 10.27263529369908746 ) ) ;
#22909 = CARTESIAN_POINT ( 'NONE',  ( 43.18784210722336070, -175.3837268820161057, -84.98333260264753619 ) ) ;
#22912 = CARTESIAN_POINT ( 'NONE',  ( 33.25242634436026634, -175.3837268820161057, -94.57776286494161866 ) ) ;
#22913 = EDGE_LOOP ( 'NONE', ( #16779, #7677, #7663, #19098 ) ) ;
#22914 = DIRECTION ( 'NONE',  ( 0.000000000000000000, 0.000000000000000000, 1.000000000000000000 ) ) ;
#22915 = EDGE_LOOP ( 'NONE', ( #5282, #29537, #49357, #11510 ) ) ;
#22916 = DIRECTION ( 'NONE',  ( 0.000000000000000000, 0.000000000000000000, 1.000000000000000000 ) ) ;
#22917 = CARTESIAN_POINT ( 'NONE',  ( -106.4764934152196645, -213.5000000000000000, 110.7307791902283043 ) ) ;
#22918 = CARTESIAN_POINT ( 'NONE',  ( -48.77118352214581876, -193.5000000000000000, -0.9564009842765195391 ) ) ;
#22919 = VECTOR ( 'NONE', #43618, 1000.000000000000000 ) ;
#22920 = VECTOR ( 'NONE', #2349, 1000.000000000000000 ) ;
#22921 = VERTEX_POINT ( 'NONE', #36135 ) ;
#22922 = EDGE_CURVE ( 'NONE', #24499, #47079, #23538, .T. ) ;
#22923 = ORIENTED_EDGE ( 'NONE', *, *, #7529, .F. ) ;
#22924 = VECTOR ( 'NONE', #40507, 1000.000000000000000 ) ;
#22925 = CARTESIAN_POINT ( 'NONE',  ( -77.43961373357964817, -193.5000000000000000, -120.5706864261535145 ) ) ;
#22926 = CARTESIAN_POINT ( 'NONE',  ( -84.53143451966468547, -193.5000000000000000, -118.6432945265036949 ) ) ;
#22927 = ORIENTED_EDGE ( 'NONE', *, *, #6628, .F. ) ;
#22928 = CARTESIAN_POINT ( 'NONE',  ( 44.30815888362531041, -189.7472609257535510, 83.75869879877568280 ) ) ;
#22929 = PLANE ( 'NONE',  #11403 ) ;
#22930 = ORIENTED_EDGE ( 'NONE', *, *, #5264, .F. ) ;
#22931 = EDGE_CURVE ( 'NONE', #39919, #45092, #48510, .T. ) ;
#22932 = CARTESIAN_POINT ( 'NONE',  ( -47.60339180931321579, -189.7472609257535510, 0.4827922027307559594 ) ) ;
#22933 = CIRCLE ( 'NONE', #8670, 11.92076361695220932 ) ;
#22934 = EDGE_CURVE ( 'NONE', #29247, #39853, #49329, .T. ) ;
#22935 = LINE ( 'NONE', #2449, #32324 ) ;
#22936 = ORIENTED_EDGE ( 'NONE', *, *, #16645, .F. ) ;
#22937 = CARTESIAN_POINT ( 'NONE',  ( 73.32083127613157103, -193.5000000000000000, 28.10285082451656535 ) ) ;
#22938 = ORIENTED_EDGE ( 'NONE', *, *, #16836, .T. ) ;
#22939 = EDGE_CURVE ( 'NONE', #39920, #8260, #16180, .T. ) ;
#22940 = LINE ( 'NONE', #10590, #23973 ) ;
#22941 = PLANE ( 'NONE',  #8485 ) ;
#22942 = ORIENTED_EDGE ( 'NONE', *, *, #13136, .T. ) ;
#22943 = AXIS2_PLACEMENT_3D ( 'NONE', #10026, #44268, #45506 ) ;
#22944 = DIRECTION ( 'NONE',  ( 0.000000000000000000, 1.000000000000000000, 0.000000000000000000 ) ) ;
#22945 = ADVANCED_FACE ( 'NONE', ( #44548 ), #48240, .T. ) ;
#22946 = PLANE ( 'NONE',  #14656 ) ;
#22947 = CARTESIAN_POINT ( 'NONE',  ( -49.32472275501068282, -189.7472609257535510, 0.5338233779647895139 ) ) ;
#22948 = VECTOR ( 'NONE', #37636, 1000.000000000000000 ) ;
#22949 = EDGE_LOOP ( 'NONE', ( #33070, #3984, #38151, #15155 ) ) ;
#22950 = LINE ( 'NONE', #19006, #35510 ) ;
#22951 = PLANE ( 'NONE',  #51318 ) ;
#22952 = EDGE_CURVE ( 'NONE', #3411, #32153, #37580, .T. ) ;
#22953 = LINE ( 'NONE', #46360, #28520 ) ;
#22955 = ORIENTED_EDGE ( 'NONE', *, *, #37685, .F. ) ;
#22954 = PLANE ( 'NONE',  #37923 ) ;
#22956 = VERTEX_POINT ( 'NONE', #8025 ) ;
#22957 = CARTESIAN_POINT ( 'NONE',  ( -97.70585564814139445, -189.7472609257535510, 113.8100815915419162 ) ) ;
#22958 = VECTOR ( 'NONE', #7421, 1000.000000000000000 ) ;
#22959 = DIRECTION ( 'NONE',  ( 1.000000000000000000, -0.000000000000000000, -0.000000000000000000 ) ) ;
#22960 = ORIENTED_EDGE ( 'NONE', *, *, #3514, .T. ) ;
#22961 = AXIS2_PLACEMENT_3D ( 'NONE', #33839, #38804, #10185 ) ;
#22962 = ORIENTED_EDGE ( 'NONE', *, *, #9365, .F. ) ;
#22963 = CARTESIAN_POINT ( 'NONE',  ( -88.23625491228469286, -193.5000000000000000, 118.5089480183148254 ) ) ;
#22964 = ORIENTED_EDGE ( 'NONE', *, *, #3234, .T. ) ;
#22965 = CARTESIAN_POINT ( 'NONE',  ( -180.0000000000000568, -115.7896721143442278, -18.45401972188387418 ) ) ;
#22966 = CARTESIAN_POINT ( 'NONE',  ( -51.89154260666841623, -183.6283474603465606, 124.9534129907280970 ) ) ;
#22967 = LINE ( 'NONE', #19028, #36187 ) ;
#22968 = CARTESIAN_POINT ( 'NONE',  ( -172.9701362814535912, -175.3837268820161057, -11.26891947860193000 ) ) ;
#22969 = ORIENTED_EDGE ( 'NONE', *, *, #5838, .T. ) ;
#22970 = ORIENTED_EDGE ( 'NONE', *, *, #29996, .F. ) ;
#22971 = VERTEX_POINT ( 'NONE', #24064 ) ;
#22972 = LINE ( 'NONE', #2994, #45097 ) ;
#22973 = CARTESIAN_POINT ( 'NONE',  ( -164.0008810331606526, -193.5000000000000000, 47.74645837849825369 ) ) ;
#22974 = PLANE ( 'NONE',  #35800 ) ;
#22975 = DIRECTION ( 'NONE',  ( 0.000000000000000000, -1.000000000000000000, 0.000000000000000000 ) ) ;
#22976 = DIRECTION ( 'NONE',  ( 0.000000000000000000, 1.000000000000000000, 0.000000000000000000 ) ) ;
#22977 = AXIS2_PLACEMENT_3D ( 'NONE', #30427, #34878, #2055 ) ;
#22978 = VERTEX_POINT ( 'NONE', #12218 ) ;
#22979 = EDGE_CURVE ( 'NONE', #19952, #5285, #40079, .T. ) ;
#22980 = EDGE_CURVE ( 'NONE', #2758, #23170, #39310, .T. ) ;
#22981 = DIRECTION ( 'NONE',  ( 0.000000000000000000, -1.000000000000000000, 0.000000000000000000 ) ) ;
#22982 = DIRECTION ( 'NONE',  ( 0.000000000000000000, 0.000000000000000000, -1.000000000000000000 ) ) ;
#22983 = AXIS2_PLACEMENT_3D ( 'NONE', #33856, #41994, #5770 ) ;
#22984 = ORIENTED_EDGE ( 'NONE', *, *, #50593, .T. ) ;
#22985 = ORIENTED_EDGE ( 'NONE', *, *, #30757, .F. ) ;
#22986 = LINE ( 'NONE', #6133, #2988 ) ;
#22987 = CARTESIAN_POINT ( 'NONE',  ( -48.47912675150883643, -193.5000000000000000, -125.0000000000000000 ) ) ;
#22988 = DIRECTION ( 'NONE',  ( -1.000000000000000000, 8.589602288500872567E-15, 5.928974370888848022E-15 ) ) ;
#22989 = LINE ( 'NONE', #10902, #3056 ) ;
#22990 = FACE_OUTER_BOUND ( 'NONE', #35770, .T. ) ;
#22991 = CARTESIAN_POINT ( 'NONE',  ( -48.47912675150885065, -175.3837268820161057, 6.938893903907228378E-15 ) ) ;
#22992 = ORIENTED_EDGE ( 'NONE', *, *, #42562, .T. ) ;
#22993 = EDGE_CURVE ( 'NONE', #27852, #20294, #45087, .T. ) ;
#22994 = DIRECTION ( 'NONE',  ( 1.000000000000000000, -0.000000000000000000, -0.000000000000000000 ) ) ;
#22995 = AXIS2_PLACEMENT_3D ( 'NONE', #43830, #41446, #25684 ) ;
#22996 = EDGE_CURVE ( 'NONE', #23360, #50065, #5393, .T. ) ;
#22997 = EDGE_LOOP ( 'NONE', ( #27254, #8497, #49997, #44719 ) ) ;
#22998 = DIRECTION ( 'NONE',  ( 0.000000000000000000, 0.000000000000000000, -1.000000000000000000 ) ) ;
#22999 = EDGE_CURVE ( 'NONE', #25253, #13145, #4602, .T. ) ;
#23000 = CARTESIAN_POINT ( 'NONE',  ( -339.1964088526558498, -84.00150778970767362, -43.83057281297470098 ) ) ;
#23001 = EDGE_LOOP ( 'NONE', ( #38692, #47232, #49020, #29470 ) ) ;
#23002 = PLANE ( 'NONE',  #48349 ) ;
#23003 = DIRECTION ( 'NONE',  ( 0.000000000000000000, 1.000000000000000000, 0.000000000000000000 ) ) ;
#23004 = CARTESIAN_POINT ( 'NONE',  ( -339.1964088526558498, -124.0000000000002700, -59.00000000000002132 ) ) ;
#23005 = CARTESIAN_POINT ( 'NONE',  ( -156.6671849566220089, -175.3837268820161057, 60.59166255800404599 ) ) ;
#23006 = DIRECTION ( 'NONE',  ( 0.000000000000000000, 0.000000000000000000, 1.000000000000000000 ) ) ;
#23007 = ORIENTED_EDGE ( 'NONE', *, *, #50236, .T. ) ;
#23008 = DIRECTION ( 'NONE',  ( -0.000000000000000000, -1.000000000000000000, 0.000000000000000000 ) ) ;
#23010 = ORIENTED_EDGE ( 'NONE', *, *, #36343, .F. ) ;
#23009 = CARTESIAN_POINT ( 'NONE',  ( -336.3521761649654422, -73.44864141332200802, 31.34948880313848107 ) ) ;
#23011 = AXIS2_PLACEMENT_3D ( 'NONE', #49058, #41160, #29332 ) ;
#23012 = CIRCLE ( 'NONE', #43150, 125.0000000000000000 ) ;
#23013 = ORIENTED_EDGE ( 'NONE', *, *, #46798, .F. ) ;
#23014 = CARTESIAN_POINT ( 'NONE',  ( -128.2395503755045638, -183.6283474603465606, -96.24590808611419845 ) ) ;
#23015 = ORIENTED_EDGE ( 'NONE', *, *, #24239, .F. ) ;
#23016 = LINE ( 'NONE', #6992, #49514 ) ;
#23017 = ORIENTED_EDGE ( 'NONE', *, *, #44106, .F. ) ;
#23018 = CARTESIAN_POINT ( 'NONE',  ( 12.12533326292403935, -193.5000000000000000, 109.3256576763158847 ) ) ;
#23019 = DIRECTION ( 'NONE',  ( 0.000000000000000000, 1.000000000000000000, -0.000000000000000000 ) ) ;
#23020 = ORIENTED_EDGE ( 'NONE', *, *, #48165, .T. ) ;
#23021 = DIRECTION ( 'NONE',  ( 0.000000000000000000, 1.000000000000000000, 0.000000000000000000 ) ) ;
#23023 = AXIS2_PLACEMENT_3D ( 'NONE', #22536, #26189, #31175 ) ;
#23022 = CARTESIAN_POINT ( 'NONE',  ( -332.3517673607765914, -92.15051119686104641, -50.05135858667769355 ) ) ;
#23024 = CARTESIAN_POINT ( 'NONE',  ( -48.53836737940255119, -183.6283474603465606, -0.9982437317643153563 ) ) ;
#23025 = EDGE_LOOP ( 'NONE', ( #49902, #643, #23070, #19959 ) ) ;
#23026 = EDGE_LOOP ( 'NONE', ( #28009, #10107, #12543, #27995 ) ) ;
#23027 = VERTEX_POINT ( 'NONE', #13274 ) ;
#23028 = LINE ( 'NONE', #50637, #46070 ) ;
#23029 = DIRECTION ( 'NONE',  ( -0.000000000000000000, 1.000000000000000000, -0.000000000000000000 ) ) ;
#23030 = DIRECTION ( 'NONE',  ( -0.8294056854502090959, 0.000000000000000000, 0.5586467658036415873 ) ) ;
#23031 = CARTESIAN_POINT ( 'NONE',  ( -37.08895481556041318, -177.1207230881787780, 124.4799742258550310 ) ) ;
#23032 = CARTESIAN_POINT ( 'NONE',  ( -339.1964088526558498, -115.7716958700746233, 59.50019592636127896 ) ) ;
#23033 = ORIENTED_EDGE ( 'NONE', *, *, #33529, .T. ) ;
#23034 = EDGE_CURVE ( 'NONE', #29760, #17894, #25832, .T. ) ;
#23035 = ADVANCED_FACE ( 'NONE', ( #17740 ), #1701, .F. ) ;
#23036 = ADVANCED_FACE ( 'NONE', ( #41122 ), #45854, .F. ) ;
#23037 = ADVANCED_FACE ( 'NONE', ( #9333 ), #33754, .F. ) ;
#23038 = CARTESIAN_POINT ( 'NONE',  ( -305.0000000000000568, -161.2787550547969033, 46.61293454085098631 ) ) ;
#23039 = EDGE_LOOP ( 'NONE', ( #7359, #495, #12612, #45105 ) ) ;
#23041 = ORIENTED_EDGE ( 'NONE', *, *, #15887, .F. ) ;
#23040 = CARTESIAN_POINT ( 'NONE',  ( -108.5723883981723930, -193.5000000000000000, 109.6074810615846360 ) ) ;
#23042 = ORIENTED_EDGE ( 'NONE', *, *, #9952, .F. ) ;
#23043 = EDGE_CURVE ( 'NONE', #12949, #37838, #33384, .T. ) ;
#23044 = CARTESIAN_POINT ( 'NONE',  ( 69.99104047056320610, -175.3837268820161057, -39.87254040532513955 ) ) ;
#23045 = ADVANCED_FACE ( 'NONE', ( #37702 ), #37178, .T. ) ;
#23046 = FACE_OUTER_BOUND ( 'NONE', #3248, .T. ) ;
#23047 = VECTOR ( 'NONE', #50716, 1000.000000000000000 ) ;
#23048 = VECTOR ( 'NONE', #28426, 1000.000000000000000 ) ;
#23049 = CARTESIAN_POINT ( 'NONE',  ( -48.18706998087188254, -177.1207230881787780, 0.9564009842765313074 ) ) ;
#23050 = DIRECTION ( 'NONE',  ( -0.000000000000000000, 1.000000000000000000, -0.000000000000000000 ) ) ;
#23051 = VERTEX_POINT ( 'NONE', #36924 ) ;
#23052 = EDGE_CURVE ( 'NONE', #28153, #10381, #39259, .T. ) ;
#23053 = DIRECTION ( 'NONE',  ( 0.000000000000000000, 0.000000000000000000, -1.000000000000000000 ) ) ;
#23054 = EDGE_LOOP ( 'NONE', ( #40384, #1157, #30421, #17899 ) ) ;
#23055 = CIRCLE ( 'NONE', #49885, 14.36509618646847386 ) ;
#23056 = ADVANCED_FACE ( 'NONE', ( #21680 ), #25354, .T. ) ;
#23057 = EDGE_CURVE ( 'NONE', #30483, #16943, #28757, .T. ) ;
#23058 = VERTEX_POINT ( 'NONE', #29295 ) ;
#23059 = CARTESIAN_POINT ( 'NONE',  ( -330.4913330509368166, -179.7763290203209579, -20.80804632820165168 ) ) ;
#23060 = FACE_OUTER_BOUND ( 'NONE', #44490, .T. ) ;
#23061 = ADVANCED_FACE ( 'NONE', ( #20629 ), #36664, .F. ) ;
#23062 = DIRECTION ( 'NONE',  ( -0.000000000000000000, 1.000000000000000000, -0.000000000000000000 ) ) ;
#23063 = FACE_OUTER_BOUND ( 'NONE', #16528, .T. ) ;
#23064 = ORIENTED_EDGE ( 'NONE', *, *, #15775, .F. ) ;
#23065 = DIRECTION ( 'NONE',  ( -0.9266896074318343723, 0.000000000000000000, 0.3758275821142357809 ) ) ;
#23066 = CARTESIAN_POINT ( 'NONE',  ( -28.74596282265200387, -177.1207230881787780, 123.4325817657431372 ) ) ;
#23067 = EDGE_CURVE ( 'NONE', #26646, #27341, #24833, .T. ) ;
#23068 = DIRECTION ( 'NONE',  ( -0.9374196611341206742, 0.000000000000000000, -0.3482016354343996367 ) ) ;
#23069 = CARTESIAN_POINT ( 'NONE',  ( -48.47912675150885065, -183.6283474603465606, 6.938893903907228378E-15 ) ) ;
#23070 = ORIENTED_EDGE ( 'NONE', *, *, #29523, .F. ) ;
#23071 = VECTOR ( 'NONE', #26663, 1000.000000000000000 ) ;
#23072 = LINE ( 'NONE', #42518, #42280 ) ;
#23073 = FACE_OUTER_BOUND ( 'NONE', #4764, .T. ) ;
#23074 = CARTESIAN_POINT ( 'NONE',  ( -330.4913330509368166, -71.49045607248250178, -27.86139516340898581 ) ) ;
#23075 = VERTEX_POINT ( 'NONE', #32718 ) ;
#23076 = FACE_OUTER_BOUND ( 'NONE', #40163, .T. ) ;
#23077 = LINE ( 'NONE', #47517, #5996 ) ;
#23078 = EDGE_LOOP ( 'NONE', ( #22245, #238, #10137, #36465 ) ) ;
#23079 = DIRECTION ( 'NONE',  ( -1.000000000000000000, 0.000000000000000000, 0.000000000000000000 ) ) ;
#23080 = VERTEX_POINT ( 'NONE', #12992 ) ;
#23081 = EDGE_CURVE ( 'NONE', #47556, #32799, #44295, .T. ) ;
#23082 = LINE ( 'NONE', #31215, #25119 ) ;
#23083 = VECTOR ( 'NONE', #32557, 1000.000000000000000 ) ;
#23084 = FACE_BOUND ( 'NONE', #16481, .T. ) ;
#23085 = CARTESIAN_POINT ( 'NONE',  ( -147.6585554144535024, -193.5000000000000000, 76.08180419845385245 ) ) ;
#23086 = AXIS2_PLACEMENT_3D ( 'NONE', #24398, #16258, #32270 ) ;
#23087 = VECTOR ( 'NONE', #26996, 1000.000000000000000 ) ;
#23088 = DIRECTION ( 'NONE',  ( 0.000000000000000000, 0.4647231720437631775, -0.8854560256532126861 ) ) ;
#23089 = EDGE_LOOP ( 'NONE', ( #46563, #2016, #40497, #33254 ) ) ;
#23090 = CIRCLE ( 'NONE', #38159, 125.0000000000000000 ) ;
#23091 = ORIENTED_EDGE ( 'NONE', *, *, #3683, .T. ) ;
#23092 = EDGE_CURVE ( 'NONE', #47750, #3706, #30862, .T. ) ;
#23093 = LINE ( 'NONE', #19401, #46042 ) ;
#23094 = ORIENTED_EDGE ( 'NONE', *, *, #19190, .F. ) ;
#23095 = MECHANICAL_DESIGN_GEOMETRIC_PRESENTATION_REPRESENTATION (  '', ( #2078 ), #28099 ) ;
#23096 = CARTESIAN_POINT ( 'NONE',  ( 50.70030191143631271, -177.1207230881787780, -76.08180419845318454 ) ) ;
#23097 = AXIS2_PLACEMENT_3D ( 'NONE', #35882, #34829, #35103 ) ;
#23098 = EDGE_CURVE ( 'NONE', #467, #1035, #50568, .T. ) ;
#23099 = EDGE_CURVE ( 'NONE', #8637, #29121, #18762, .T. ) ;
#23100 = EDGE_CURVE ( 'NONE', #12871, #49461, #25872, .T. ) ;
#23101 = AXIS2_PLACEMENT_3D ( 'NONE', #38357, #18400, #34417 ) ;
#23102 = EDGE_CURVE ( 'NONE', #32388, #39056, #30074, .T. ) ;
#23103 = VECTOR ( 'NONE', #33048, 1000.000000000000000 ) ;
#23104 = DIRECTION ( 'NONE',  ( 0.000000000000000000, -0.000000000000000000, 1.000000000000000000 ) ) ;
#23105 = CARTESIAN_POINT ( 'NONE',  ( 32.99469856375238663, -175.3837268820161057, 94.79987230212020677 ) ) ;
#23106 = ORIENTED_EDGE ( 'NONE', *, *, #33025, .F. ) ;
#23109 = VERTEX_POINT ( 'NONE', #34007 ) ;
#23108 = DIRECTION ( 'NONE',  ( -0.000000000000000000, 1.000000000000000000, -0.000000000000000000 ) ) ;
#23107 = LINE ( 'NONE', #38351, #25030 ) ;
#23110 = EDGE_CURVE ( 'NONE', #22832, #27333, #17994, .T. ) ;
#23111 = LINE ( 'NONE', #39887, #430 ) ;
#23112 = ORIENTED_EDGE ( 'NONE', *, *, #24146, .F. ) ;
#23113 = DIRECTION ( 'NONE',  ( -0.000000000000000000, 1.000000000000000000, -0.000000000000000000 ) ) ;
#23114 = ORIENTED_EDGE ( 'NONE', *, *, #11307, .F. ) ;
#23115 = DIRECTION ( 'NONE',  ( -0.000000000000000000, -0.8854560256532062468, 0.4647231720437755564 ) ) ;
#23116 = VERTEX_POINT ( 'NONE', #6687 ) ;
#23117 = EDGE_CURVE ( 'NONE', #36354, #21929, #18257, .T. ) ;
#23119 = LINE ( 'NONE', #11268, #5696 ) ;
#23118 = PLANE ( 'NONE',  #49266 ) ;
#23120 = ORIENTED_EDGE ( 'NONE', *, *, #45039, .T. ) ;
#23121 = LINE ( 'NONE', #15235, #21540 ) ;
#23122 = ORIENTED_EDGE ( 'NONE', *, *, #48967, .T. ) ;
#23123 = DIRECTION ( 'NONE',  ( 0.000000000000000000, -1.000000000000000000, -0.000000000000000000 ) ) ;
#23124 = VECTOR ( 'NONE', #9044, 1000.000000000000000 ) ;
#23125 = CARTESIAN_POINT ( 'NONE',  ( -172.9701362814535912, -189.7472609257535510, -11.26891947860197440 ) ) ;
#23126 = EDGE_CURVE ( 'NONE', #20990, #672, #50199, .T. ) ;
#23127 = ORIENTED_EDGE ( 'NONE', *, *, #6983, .F. ) ;
#23128 = LINE ( 'NONE', #14997, #28888 ) ;
#23129 = DIRECTION ( 'NONE',  ( 0.000000000000000000, -1.000000000000000000, 0.000000000000000000 ) ) ;
#23130 = DIRECTION ( 'NONE',  ( 0.000000000000000000, 0.9350162426854146114, -0.3546048870425363986 ) ) ;
#23131 = AXIS2_PLACEMENT_3D ( 'NONE', #621, #43728, #7731 ) ;
#23132 = LINE ( 'NONE', #11278, #24887 ) ;
#23133 = VECTOR ( 'NONE', #22428, 1000.000000000000114 ) ;
#23134 = EDGE_CURVE ( 'NONE', #28728, #39637, #4876, .T. ) ;
#23135 = ORIENTED_EDGE ( 'NONE', *, *, #23676, .F. ) ;
#23136 = SHAPE_REPRESENTATION_RELATIONSHIP ( 'NONE' , 'NONE' ,  #40181, #12969 ) ;
#23137 = FACE_OUTER_BOUND ( 'NONE', #29158, .T. ) ;
#23138 = CARTESIAN_POINT ( 'NONE',  ( 62.86098202833237281, -183.6283474603465606, 56.81883646197908888 ) ) ;
#23139 = EDGE_CURVE ( 'NONE', #37538, #37621, #5916, .T. ) ;
#23140 = CARTESIAN_POINT ( 'NONE',  ( 47.04848625005566021, -183.6283474603465606, 80.61932246194658092 ) ) ;
#23141 = ORIENTED_EDGE ( 'NONE', *, *, #8409, .T. ) ;
#23142 = CARTESIAN_POINT ( 'NONE',  ( -330.4913330509368166, -178.4886558749180949, 21.38919645685269444 ) ) ;
#23143 = CARTESIAN_POINT ( 'NONE',  ( -47.70260288879081401, -177.1207230881787780, 0.6300878435817218737 ) ) ;
#23144 = CIRCLE ( 'NONE', #43230, 15.00000000000000000 ) ;
#23145 = AXIS2_PLACEMENT_3D ( 'NONE', #45896, #951, #13310 ) ;
#23146 = DIRECTION ( 'NONE',  ( 0.000000000000000000, 0.000000000000000000, -1.000000000000000000 ) ) ;
#23147 = DIRECTION ( 'NONE',  ( -0.000000000000000000, 1.000000000000000000, -0.000000000000000000 ) ) ;
#23148 = LINE ( 'NONE', #34700, #2307 ) ;
#23149 = ORIENTED_EDGE ( 'NONE', *, *, #15408, .F. ) ;
#23150 = VECTOR ( 'NONE', #34918, 1000.000000000000000 ) ;
#23151 = EDGE_CURVE ( 'NONE', #9685, #7739, #26381, .T. ) ;
#23152 = CIRCLE ( 'NONE', #30666, 125.0000000000000000 ) ;
#23153 = DIRECTION ( 'NONE',  ( 0.9646355819083556327, 0.000000000000000000, 0.2635871660690782825 ) ) ;
#23154 = DIRECTION ( 'NONE',  ( 0.000000000000000000, -0.000000000000000000, -1.000000000000000000 ) ) ;
#23155 = CARTESIAN_POINT ( 'NONE',  ( -152.8876895714563773, -175.3837268820161057, 66.89437584437912676 ) ) ;
#23156 = CYLINDRICAL_SURFACE ( 'NONE', #38793, 125.0000000000000000 ) ;
#23157 = DIRECTION ( 'NONE',  ( 1.043714542225393697E-14, -0.5680647467311569221, -0.8229838658936556861 ) ) ;
#23158 = ORIENTED_EDGE ( 'NONE', *, *, #6961, .T. ) ;
#23159 = DIRECTION ( 'NONE',  ( 0.000000000000000000, 0.000000000000000000, 1.000000000000000000 ) ) ;
#23160 = VERTEX_POINT ( 'NONE', #22187 ) ;
#23161 = ORIENTED_EDGE ( 'NONE', *, *, #43583, .T. ) ;
#23162 = VECTOR ( 'NONE', #9963, 1000.000000000000000 ) ;
#23163 = VERTEX_POINT ( 'NONE', #46631 ) ;
#23164 = DIRECTION ( 'NONE',  ( -0.000000000000000000, 1.000000000000000000, -0.000000000000000000 ) ) ;
#23165 = VECTOR ( 'NONE', #51501, 1000.000000000000000 ) ;
#23166 = AXIS2_PLACEMENT_3D ( 'NONE', #50537, #35264, #14537 ) ;
#23167 = EDGE_CURVE ( 'NONE', #6669, #48376, #37953, .T. ) ;
#23168 = EDGE_CURVE ( 'NONE', #6473, #39339, #34519, .T. ) ;
#23169 = DIRECTION ( 'NONE',  ( 0.000000000000000000, 0.9709418174260511236, -0.2393156642875615969 ) ) ;
#23170 = VERTEX_POINT ( 'NONE', #14310 ) ;
#23171 = DIRECTION ( 'NONE',  ( 0.000000000000000000, -0.2393156642875685636, -0.9709418174260492362 ) ) ;
#23172 = DIRECTION ( 'NONE',  ( 0.000000000000000000, 0.000000000000000000, 1.000000000000000000 ) ) ;
#23175 = ORIENTED_EDGE ( 'NONE', *, *, #6799, .F. ) ;
#23174 = CARTESIAN_POINT ( 'NONE',  ( -332.3517673607765914, -182.5000000000000568, 2.632288850093980503 ) ) ;
#23173 = PLANE ( 'NONE',  #33357 ) ;
#23176 = VECTOR ( 'NONE', #30087, 1000.000000000000227 ) ;
#23177 = AXIS2_PLACEMENT_3D ( 'NONE', #8771, #21385, #44789 ) ;
#23178 = DIRECTION ( 'NONE',  ( 0.000000000000000000, -4.093947403305264743E-14, -1.000000000000000000 ) ) ;
#23179 = ORIENTED_EDGE ( 'NONE', *, *, #13500, .T. ) ;
#23180 = CARTESIAN_POINT ( 'NONE',  ( 72.95485052494852596, -177.1207230881787780, -29.64437826672757836 ) ) ;
#23181 = ORIENTED_EDGE ( 'NONE', *, *, #5649, .F. ) ;
#23182 = DIRECTION ( 'NONE',  ( -0.9027978299657446470, 0.000000000000000000, 0.4300652022765183435 ) ) ;
#23183 = AXIS2_PLACEMENT_3D ( 'NONE', #41956, #38541, #46180 ) ;
#23184 = DIRECTION ( 'NONE',  ( -0.000000000000000000, 0.3546048870425331789, -0.9350162426854158326 ) ) ;
#23186 = CARTESIAN_POINT ( 'NONE',  ( 61.69163308845453031, -183.6283474603465606, -56.90809649257491998 ) ) ;
#23185 = DIRECTION ( 'NONE',  ( 0.000000000000000000, -1.000000000000000000, 0.000000000000000000 ) ) ;
#23187 = ORIENTED_EDGE ( 'NONE', *, *, #39174, .F. ) ;
#23188 = VECTOR ( 'NONE', #13354, 1000.000000000000114 ) ;
#23189 = CARTESIAN_POINT ( 'NONE',  ( 1.806149300554621862, 28.00000000000000355, -48.96369439584437799 ) ) ;
#23190 = ORIENTED_EDGE ( 'NONE', *, *, #14612, .T. ) ;
#23191 = DIRECTION ( 'NONE',  ( -0.000000000000000000, 1.000000000000000000, -0.000000000000000000 ) ) ;
#23192 = DIRECTION ( 'NONE',  ( 0.000000000000000000, 0.000000000000000000, 1.000000000000000000 ) ) ;
#23193 = ORIENTED_EDGE ( 'NONE', *, *, #30601, .T. ) ;
#23194 = EDGE_CURVE ( 'NONE', #28946, #44188, #21641, .T. ) ;
#23195 = LINE ( 'NONE', #39212, #7307 ) ;
#23196 = CARTESIAN_POINT ( 'NONE',  ( -18.31235070009513421, -193.5000000000000000, 121.3052580173829966 ) ) ;
#23197 = EDGE_LOOP ( 'NONE', ( #31818, #17707, #22329, #38300 ) ) ;
#23198 = CYLINDRICAL_SURFACE ( 'NONE', #724, 60.00000000000000000 ) ;
#23199 = FACE_OUTER_BOUND ( 'NONE', #32823, .T. ) ;
#23200 = EDGE_CURVE ( 'NONE', #25116, #16167, #10357, .T. ) ;
#23201 = ORIENTED_EDGE ( 'NONE', *, *, #39827, .T. ) ;
#23202 = DIRECTION ( 'NONE',  ( -0.5085311186492216251, 0.000000000000000000, 0.8610436117673548884 ) ) ;
#23203 = VERTEX_POINT ( 'NONE', #2983 ) ;
#23204 = AXIS2_PLACEMENT_3D ( 'NONE', #41417, #5438, #21457 ) ;
#23205 = VECTOR ( 'NONE', #4136, 1000.000000000000000 ) ;
#23206 = CARTESIAN_POINT ( 'NONE',  ( -173.0563034899574859, -193.5000000000000000, -10.27263529369817618 ) ) ;
#23207 = CARTESIAN_POINT ( 'NONE',  ( -73.94077438226446475, -183.6283474603465606, 122.3793467049372481 ) ) ;
#23208 = ORIENTED_EDGE ( 'NONE', *, *, #17404, .F. ) ;
#23209 = VECTOR ( 'NONE', #29201, 1000.000000000000000 ) ;
#23210 = DIRECTION ( 'NONE',  ( -0.000000000000000000, 0.4647231720437789981, 0.8854560256532044704 ) ) ;
#23211 = DIRECTION ( 'NONE',  ( 0.000000000000000000, 0.000000000000000000, 1.000000000000000000 ) ) ;
#23212 = PLANE ( 'NONE',  #32456 ) ;
#23213 = DIRECTION ( 'NONE',  ( 0.000000000000000000, 0.000000000000000000, 1.000000000000000000 ) ) ;
#23214 = AXIS2_PLACEMENT_3D ( 'NONE', #6139, #33971, #50021 ) ;
#23215 = VECTOR ( 'NONE', #16705, 1000.000000000000227 ) ;
#23216 = DIRECTION ( 'NONE',  ( 0.000000000000000000, -1.942890293094023946E-14, -1.000000000000000000 ) ) ;
#23217 = CARTESIAN_POINT ( 'NONE',  ( -134.2540868116286674, -193.5000000000000000, 89.54698061029657197 ) ) ;
#23219 = ORIENTED_EDGE ( 'NONE', *, *, #36269, .F. ) ;
#23218 = CARTESIAN_POINT ( 'NONE',  ( -160.0000000000000284, -123.5000000000000284, -45.63467731922664683 ) ) ;
#23220 = VECTOR ( 'NONE', #10729, 1000.000000000000000 ) ;
#23221 = VECTOR ( 'NONE', #44266, 999.9999999999998863 ) ;
#23222 = ORIENTED_EDGE ( 'NONE', *, *, #50526, .T. ) ;
#23223 = DIRECTION ( 'NONE',  ( -0.9960498426152158968, 0.000000000000000000, -0.08879589532294571153 ) ) ;
#23224 = AXIS2_PLACEMENT_3D ( 'NONE', #44813, #5141, #37436 ) ;
#23225 = AXIS2_PLACEMENT_3D ( 'NONE', #51301, #7422, #39447 ) ;
#23226 = CARTESIAN_POINT ( 'NONE',  ( -101.9736325116273576, -183.6283474603465606, 112.9749434763330527 ) ) ;
#23227 = ORIENTED_EDGE ( 'NONE', *, *, #47820, .T. ) ;
#23228 = ORIENTED_EDGE ( 'NONE', *, *, #36862, .F. ) ;
#23229 = DIRECTION ( 'NONE',  ( -0.9960498426152177842, 0.000000000000000000, 0.08879589532292482545 ) ) ;
#23230 = ORIENTED_EDGE ( 'NONE', *, *, #26113, .T. ) ;
#23231 = LINE ( 'NONE', #36074, #46853 ) ;
#23232 = CARTESIAN_POINT ( 'NONE',  ( -339.1964088526558498, -171.7720157143604069, -33.92731199008472487 ) ) ;
#23233 = EDGE_CURVE ( 'NONE', #28841, #51547, #15097, .T. ) ;
#23234 = LINE ( 'NONE', #19527, #10988 ) ;
#23235 = LINE ( 'NONE', #19295, #32479 ) ;
#23236 = VERTEX_POINT ( 'NONE', #50831 ) ;
#23237 = EDGE_LOOP ( 'NONE', ( #31422, #45016, #22598, #28283 ) ) ;
#23238 = ORIENTED_EDGE ( 'NONE', *, *, #47832, .F. ) ;
#23239 = CARTESIAN_POINT ( 'NONE',  ( -330.4913330509368166, -167.9936954712156023, -38.74998146212117689 ) ) ;
#23240 = LINE ( 'NONE', #51879, #47861 ) ;
#23241 = AXIS2_PLACEMENT_3D ( 'NONE', #41885, #26813, #21664 ) ;
#23242 = PLANE ( 'NONE',  #29082 ) ;
#23243 = VECTOR ( 'NONE', #30830, 1000.000000000000000 ) ;
#23244 = CARTESIAN_POINT ( 'NONE',  ( -168.9345475356665531, -177.1207230881787780, 29.43839964798725362 ) ) ;
#23245 = DIRECTION ( 'NONE',  ( -1.000000000000000000, 0.000000000000000000, 0.000000000000000000 ) ) ;
#23246 = ORIENTED_EDGE ( 'NONE', *, *, #41378, .T. ) ;
#23247 = VECTOR ( 'NONE', #22448, 999.9999999999998863 ) ;
#23248 = ADVANCED_FACE ( 'NONE', ( #14837 ), #46897, .T. ) ;
#23249 = CARTESIAN_POINT ( 'NONE',  ( -122.3978016498073202, -177.1207230881787780, -100.8019320314827212 ) ) ;
#23250 = DIRECTION ( 'NONE',  ( 0.000000000000000000, -1.000000000000000000, 0.000000000000000000 ) ) ;
#23251 = ORIENTED_EDGE ( 'NONE', *, *, #15398, .F. ) ;
#23252 = EDGE_LOOP ( 'NONE', ( #42732, #5012, #15117, #13602 ) ) ;
#23253 = VECTOR ( 'NONE', #9086, 1000.000000000000114 ) ;
#23254 = FACE_OUTER_BOUND ( 'NONE', #10465, .T. ) ;
#23255 = CARTESIAN_POINT ( 'NONE',  ( -305.0000000000000568, -65.36517161715264024, 14.84391218300897464 ) ) ;
#23256 = AXIS2_PLACEMENT_3D ( 'NONE', #7368, #19187, #14221 ) ;
#23257 = VERTEX_POINT ( 'NONE', #38972 ) ;
#23258 = ADVANCED_FACE ( 'NONE', ( #9848 ), #21930, .F. ) ;
#23259 = DIRECTION ( 'NONE',  ( -0.000000000000000000, 0.6631226582407937498, -0.7485107481711024136 ) ) ;
#23260 = VECTOR ( 'NONE', #6127, 1000.000000000000000 ) ;
#23261 = AXIS2_PLACEMENT_3D ( 'NONE', #27121, #19754, #3469 ) ;
#23262 = CARTESIAN_POINT ( 'NONE',  ( -330.4913330509368166, -179.4217241332781612, 21.74306257088775141 ) ) ;
#23263 = FACE_OUTER_BOUND ( 'NONE', #16675, .T. ) ;
#23264 = ORIENTED_EDGE ( 'NONE', *, *, #16090, .F. ) ;
#23265 = FACE_OUTER_BOUND ( 'NONE', #40295, .T. ) ;
#23266 = VECTOR ( 'NONE', #35552, 1000.000000000000000 ) ;
#23267 = AXIS2_PLACEMENT_3D ( 'NONE', #5821, #33646, #9739 ) ;
#23268 = VERTEX_POINT ( 'NONE', #32129 ) ;
#23269 = FACE_OUTER_BOUND ( 'NONE', #2132, .T. ) ;
#23270 = FACE_OUTER_BOUND ( 'NONE', #18151, .T. ) ;
#23271 = ORIENTED_EDGE ( 'NONE', *, *, #21553, .T. ) ;
#23272 = CARTESIAN_POINT ( 'NONE',  ( -169.0855799822425922, -193.5000000000000000, -28.81338593823970839 ) ) ;
#23273 = CARTESIAN_POINT ( 'NONE',  ( -48.47912675150885065, -193.5000000000000000, 6.938893903907228378E-15 ) ) ;
#23274 = LINE ( 'NONE', #31393, #14792 ) ;
#23275 = LINE ( 'NONE', #31917, #16524 ) ;
#23276 = LINE ( 'NONE', #27715, #29491 ) ;
#23277 = ORIENTED_EDGE ( 'NONE', *, *, #1105, .T. ) ;
#23278 = ORIENTED_EDGE ( 'NONE', *, *, #35411, .T. ) ;
#23279 = AXIS2_PLACEMENT_3D ( 'NONE', #32857, #2029, #4759 ) ;
#23280 = VECTOR ( 'NONE', #17915, 1000.000000000000000 ) ;
#23281 = CARTESIAN_POINT ( 'NONE',  ( 72.82672500347334221, -193.5000000000000000, 25.70779184431858155 ) ) ;
#23283 = VERTEX_POINT ( 'NONE', #47667 ) ;
#23282 = CARTESIAN_POINT ( 'NONE',  ( -336.3521761649653854, -71.15086438280971493, -29.31839013542551342 ) ) ;
#23284 = CIRCLE ( 'NONE', #25792, 60.00000000000000000 ) ;
#23285 = EDGE_CURVE ( 'NONE', #47681, #50353, #35817, .T. ) ;
#23286 = ORIENTED_EDGE ( 'NONE', *, *, #16996, .F. ) ;
#23287 = EDGE_CURVE ( 'NONE', #3372, #41076, #27410, .T. ) ;
#23288 = CARTESIAN_POINT ( 'NONE',  ( -40.96347969518280507, -193.5000000000000000, -123.7720294769268889 ) ) ;
#23289 = VECTOR ( 'NONE', #31107, 1000.000000000000000 ) ;
#23290 = VERTEX_POINT ( 'NONE', #11122 ) ;
#23291 = LINE ( 'NONE', #7252, #1255 ) ;
#23292 = CIRCLE ( 'NONE', #21607, 125.0000000000000000 ) ;
#23293 = CARTESIAN_POINT ( 'NONE',  ( -339.1964088526558498, -102.1108035431470427, 54.98865587491797413 ) ) ;
#23294 = ORIENTED_EDGE ( 'NONE', *, *, #40633, .T. ) ;
#23295 = PLANE ( 'NONE',  #15757 ) ;
#23296 = CIRCLE ( 'NONE', #628, 125.0000000000000000 ) ;
#23297 = EDGE_CURVE ( 'NONE', #32383, #50178, #15339, .T. ) ;
#23298 = AXIS2_PLACEMENT_3D ( 'NONE', #41811, #13690, #37611 ) ;
#23299 = DIRECTION ( 'NONE',  ( 0.000000000000000000, 0.000000000000000000, 1.000000000000000000 ) ) ;
#23300 = DIRECTION ( 'NONE',  ( -0.000000000000000000, 1.000000000000000000, -0.000000000000000000 ) ) ;
#23301 = ORIENTED_EDGE ( 'NONE', *, *, #38525, .T. ) ;
#23302 = ORIENTED_EDGE ( 'NONE', *, *, #27187, .F. ) ;
#23303 = EDGE_CURVE ( 'NONE', #9591, #28684, #26696, .T. ) ;
#23304 = VERTEX_POINT ( 'NONE', #27149 ) ;
#23305 = VECTOR ( 'NONE', #14517, 1000.000000000000000 ) ;
#23306 = LINE ( 'NONE', #51174, #9980 ) ;
#23307 = PLANE ( 'NONE',  #13424 ) ;
#23308 = ADVANCED_FACE ( 'NONE', ( #39735 ), #23484, .T. ) ;
#23309 = DIRECTION ( 'NONE',  ( 0.000000000000000000, 1.000000000000000000, 0.000000000000000000 ) ) ;
#23310 = DIRECTION ( 'NONE',  ( -0.9646355819083594074, 0.000000000000000000, 0.2635871660690647933 ) ) ;
#23311 = CARTESIAN_POINT ( 'NONE',  ( 73.66680038934278230, -189.7472609257535510, -26.55884942729568721 ) ) ;
#23312 = EDGE_LOOP ( 'NONE', ( #42769, #36671, #11972, #223 ) ) ;
#23313 = FACE_OUTER_BOUND ( 'NONE', #40274, .T. ) ;
#23314 = ORIENTED_EDGE ( 'NONE', *, *, #3190, .T. ) ;
#23315 =( REPRESENTATION_RELATIONSHIP ('NONE','NONE', #4578, #15639 ) REPRESENTATION_RELATIONSHIP_WITH_TRANSFORMATION ( #10452 )SHAPE_REPRESENTATION_RELATIONSHIP( ) );
#23317 = ORIENTED_EDGE ( 'NONE', *, *, #25665, .F. ) ;
#23316 = DIRECTION ( 'NONE',  ( 0.4566292373937140270, 0.000000000000000000, -0.8896570909947467687 ) ) ;
#23318 = VECTOR ( 'NONE', #1720, 1000.000000000000000 ) ;
#23319 = ORIENTED_EDGE ( 'NONE', *, *, #50424, .F. ) ;
#23320 = VECTOR ( 'NONE', #18080, 1000.000000000000000 ) ;
#23321 = LINE ( 'NONE', #18837, #44237 ) ;
#23322 = EDGE_CURVE ( 'NONE', #17812, #28521, #1524, .T. ) ;
#23323 = CARTESIAN_POINT ( 'NONE',  ( 52.59568867645218404, -189.7472609257535510, -73.54509967498589162 ) ) ;
#23324 = VECTOR ( 'NONE', #22457, 1000.000000000000000 ) ;
#23325 = LINE ( 'NONE', #44051, #48131 ) ;
#23326 = DIRECTION ( 'NONE',  ( -0.000000000000000000, 1.000000000000000000, -0.000000000000000000 ) ) ;
#23327 = VERTEX_POINT ( 'NONE', #11649 ) ;
#23328 = DIRECTION ( 'NONE',  ( -0.000000000000000000, 1.000000000000000000, -0.000000000000000000 ) ) ;
#23329 = VERTEX_POINT ( 'NONE', #43181 ) ;
#23330 = EDGE_LOOP ( 'NONE', ( #2957, #30384, #10622, #14427 ) ) ;
#23331 = CARTESIAN_POINT ( 'NONE',  ( -330.4913330509368166, -182.0095552316575152, 7.608018572113473432 ) ) ;
#23332 = AXIS2_PLACEMENT_3D ( 'NONE', #8534, #3829, #31935 ) ;
#23333 = CARTESIAN_POINT ( 'NONE',  ( -173.0003472773501301, -193.5000000000000000, 10.93003379476953363 ) ) ;
#23334 = CARTESIAN_POINT ( 'NONE',  ( -330.4913330509368166, -71.02573290043878274, -26.97593913775585150 ) ) ;
#23335 = CARTESIAN_POINT ( 'NONE',  ( -124.4642912599203726, -175.3837268820161057, 99.25348746834863789 ) ) ;
#23336 = DIRECTION ( 'NONE',  ( 0.2920567706369764371, 0.000000000000000000, -0.9564009842765223146 ) ) ;
#23337 = PLANE ( 'NONE',  #22884 ) ;
#23338 = VERTEX_POINT ( 'NONE', #47395 ) ;
#23339 = LINE ( 'NONE', #51455, #12912 ) ;
#23340 = CARTESIAN_POINT ( 'NONE',  ( 17.15229921100055321, -183.6283474603465606, -106.3838142112212779 ) ) ;
#23341 = VECTOR ( 'NONE', #15484, 1000.000000000000000 ) ;
#23342 = DIRECTION ( 'NONE',  ( 0.000000000000000000, 0.000000000000000000, 1.000000000000000000 ) ) ;
#23343 = ORIENTED_EDGE ( 'NONE', *, *, #14094, .F. ) ;
#23344 = DIRECTION ( 'NONE',  ( -0.000000000000000000, 1.000000000000000000, -0.000000000000000000 ) ) ;
#23345 = EDGE_CURVE ( 'NONE', #16540, #50918, #12874, .T. ) ;
#23346 = ORIENTED_EDGE ( 'NONE', *, *, #33016, .F. ) ;
#23347 = ADVANCED_FACE ( 'NONE', ( #3750 ), #28895, .F. ) ;
#23348 = DIRECTION ( 'NONE',  ( -0.6965510290630033685, 0.000000000000000000, 0.7175072570443249420 ) ) ;
#23349 = EDGE_LOOP ( 'NONE', ( #32644, #16406, #6469, #8779 ) ) ;
#23350 = CIRCLE ( 'NONE', #9920, 125.0000000000000000 ) ;
#23351 = PLANE ( 'NONE',  #51133 ) ;
#23352 = CIRCLE ( 'NONE', #48535, 125.0000000000000000 ) ;
#23353 = FACE_BOUND ( 'NONE', #18550, .T. ) ;
#23354 = DIRECTION ( 'NONE',  ( 0.000000000000000000, 0.000000000000000000, 1.000000000000000000 ) ) ;
#23355 = CIRCLE ( 'NONE', #30066, 125.0000000000000000 ) ;
#23356 = EDGE_CURVE ( 'NONE', #20241, #4422, #19781, .T. ) ;
#23357 = CARTESIAN_POINT ( 'NONE',  ( -53.47502265695602119, -193.5000000000000000, -123.9001241957025883 ) ) ;
#23358 = ORIENTED_EDGE ( 'NONE', *, *, #50358, .T. ) ;
#23359 = EDGE_CURVE ( 'NONE', #21393, #11641, #23362, .T. ) ;
#23360 = VERTEX_POINT ( 'NONE', #8941 ) ;
#23361 = DIRECTION ( 'NONE',  ( 0.000000000000000000, 1.000000000000000000, 0.000000000000000000 ) ) ;
#23362 = CIRCLE ( 'NONE', #14968, 125.0000000000000000 ) ;
#23363 = EDGE_CURVE ( 'NONE', #8278, #14662, #5744, .T. ) ;
#23364 = EDGE_LOOP ( 'NONE', ( #23475, #8146, #6196, #33935 ) ) ;
#23365 = FACE_OUTER_BOUND ( 'NONE', #33760, .T. ) ;
#23366 = EDGE_CURVE ( 'NONE', #9485, #3068, #23231, .T. ) ;
#23367 = AXIS2_PLACEMENT_3D ( 'NONE', #50214, #46781, #17638 ) ;
#23368 = CYLINDRICAL_SURFACE ( 'NONE', #43239, 15.00000000000000000 ) ;
#23369 = ORIENTED_EDGE ( 'NONE', *, *, #38870, .F. ) ;
#23372 = VERTEX_POINT ( 'NONE', #7705 ) ;
#23371 = LINE ( 'NONE', #47027, #15525 ) ;
#23370 = CARTESIAN_POINT ( 'NONE',  ( -336.3521761649654422, -128.9912765084839066, 58.76657425099337928 ) ) ;
#23373 = CARTESIAN_POINT ( 'NONE',  ( -330.4913330509368166, -151.3613951634091848, -52.00954392751743427 ) ) ;
#23374 = ORIENTED_EDGE ( 'NONE', *, *, #28548, .F. ) ;
#23375 = CARTESIAN_POINT ( 'NONE',  ( -171.9838957966129840, -175.3837268820161057, 19.27620354518724355 ) ) ;
#23376 = VERTEX_POINT ( 'NONE', #71 ) ;
#23377 = DIRECTION ( 'NONE',  ( -1.000000000000000000, -0.000000000000000000, 0.000000000000000000 ) ) ;
#23378 = ORIENTED_EDGE ( 'NONE', *, *, #7066, .T. ) ;
#23380 = CARTESIAN_POINT ( 'NONE',  ( -48.47912675150885065, -189.7472609257535510, 6.938893903907228378E-15 ) ) ;
#23379 = CARTESIAN_POINT ( 'NONE',  ( -332.3517673607765914, -123.5000000000000284, 0.000000000000000000 ) ) ;
#23381 = VERTEX_POINT ( 'NONE', #3494 ) ;
#23382 = LINE ( 'NONE', #19425, #10611 ) ;
#23383 = CARTESIAN_POINT ( 'NONE',  ( 0.000000000000000000, 0.000000000000000000, 0.000000000000000000 ) ) ;
#23384 = ORIENTED_EDGE ( 'NONE', *, *, #5789, .T. ) ;
#23385 = DIRECTION ( 'NONE',  ( -0.000000000000000000, 1.000000000000000000, 0.000000000000000000 ) ) ;
#23386 = AXIS2_PLACEMENT_3D ( 'NONE', #30294, #50539, #14539 ) ;
#23387 = LINE ( 'NONE', #28077, #20641 ) ;
#23388 = LINE ( 'NONE', #20211, #34743 ) ;
#23389 = DIRECTION ( 'NONE',  ( 0.000000000000000000, 0.4647231720437631775, -0.8854560256532126861 ) ) ;
#23390 = DIRECTION ( 'NONE',  ( -0.000000000000000000, 1.000000000000000000, -0.000000000000000000 ) ) ;
#23391 = PLANE ( 'NONE',  #38152 ) ;
#23392 = VERTEX_POINT ( 'NONE', #24979 ) ;
#23393 = CARTESIAN_POINT ( 'NONE',  ( 31.86508519151254148, 4.999999999999997335, 53.84468928687354605 ) ) ;
#23394 = DIRECTION ( 'NONE',  ( -0.000000000000000000, 1.000000000000000000, -0.000000000000000000 ) ) ;
#23395 = CARTESIAN_POINT ( 'NONE',  ( -339.1964088526558498, -123.5000000000000142, 60.00000000000000000 ) ) ;
#23396 = ADVANCED_FACE ( 'NONE', ( #40993 ), #19522, .T. ) ;
#23397 = DIRECTION ( 'NONE',  ( -0.000000000000000000, 1.000000000000000000, -0.000000000000000000 ) ) ;
#23398 = VERTEX_POINT ( 'NONE', #51593 ) ;
#23399 = VECTOR ( 'NONE', #27215, 1000.000000000000000 ) ;
#23400 = PLANE ( 'NONE',  #37448 ) ;
#23401 = DIRECTION ( 'NONE',  ( 0.000000000000000000, -0.000000000000000000, -1.000000000000000000 ) ) ;
#23402 = EDGE_CURVE ( 'NONE', #33538, #45739, #31614, .T. ) ;
#23403 = CYLINDRICAL_SURFACE ( 'NONE', #19385, 124.9999999999999858 ) ;
#23405 = EDGE_LOOP ( 'NONE', ( #7289, #6122, #51080, #24498 ) ) ;
#23404 = CARTESIAN_POINT ( 'NONE',  ( 74.13662511985246795, -175.3837268820161057, 18.47640724094593168 ) ) ;
#23406 = EDGE_CURVE ( 'NONE', #22228, #18767, #25230, .T. ) ;
#23407 = ADVANCED_FACE ( 'NONE', ( #5270 ), #13142, .T. ) ;
#23408 = ORIENTED_EDGE ( 'NONE', *, *, #14324, .F. ) ;
#23409 = ORIENTED_EDGE ( 'NONE', *, *, #28211, .F. ) ;
#23410 = EDGE_CURVE ( 'NONE', #48020, #38286, #12426, .T. ) ;
#23411 = LINE ( 'NONE', #19451, #21202 ) ;
#23412 = ADVANCED_FACE ( 'NONE', ( #9460 ), #33629, .T. ) ;
#23413 = CARTESIAN_POINT ( 'NONE',  ( 72.05536924052414349, -193.5000000000000000, 33.11246405730899056 ) ) ;
#23414 = CARTESIAN_POINT ( 'NONE',  ( -336.3521761649654422, -66.84438072661991725, -16.67542351306652648 ) ) ;
#23415 = DIRECTION ( 'NONE',  ( 0.000000000000000000, 1.000000000000000000, 0.000000000000000000 ) ) ;
#23416 = VERTEX_POINT ( 'NONE', #38341 ) ;
#23417 = EDGE_CURVE ( 'NONE', #787, #32651, #47716, .T. ) ;
#23418 = CARTESIAN_POINT ( 'NONE',  ( 0.2934699642939896380, 58.14470866581339692, -16.45750525699327937 ) ) ;
#23419 = EDGE_CURVE ( 'NONE', #17366, #34920, #41821, .T. ) ;
#23420 = ORIENTED_EDGE ( 'NONE', *, *, #16533, .T. ) ;
#23421 = ORIENTED_EDGE ( 'NONE', *, *, #39424, .T. ) ;
#23422 = ADVANCED_FACE ( 'NONE', ( #49668 ), #13923, .F. ) ;
#23423 = VECTOR ( 'NONE', #34138, 1000.000000000000000 ) ;
#23424 = ORIENTED_EDGE ( 'NONE', *, *, #41368, .T. ) ;
#23425 = DIRECTION ( 'NONE',  ( 0.000000000000000000, 0.000000000000000000, -1.000000000000000000 ) ) ;
#23426 = AXIS2_PLACEMENT_3D ( 'NONE', #20917, #36937, #927 ) ;
#23427 = EDGE_CURVE ( 'NONE', #18925, #11600, #49426, .T. ) ;
#23428 = DIRECTION ( 'NONE',  ( 1.000000000000000000, 0.000000000000000000, 0.000000000000000000 ) ) ;
#23429 = EDGE_LOOP ( 'NONE', ( #16782, #21955, #19449, #24516 ) ) ;
#23430 = ADVANCED_FACE ( 'NONE', ( #29941 ), #26001, .T. ) ;
#23431 = CARTESIAN_POINT ( 'NONE',  ( -48.47912675150885065, -183.6283474603465606, 6.938893903907228378E-15 ) ) ;
#23432 = FACE_OUTER_BOUND ( 'NONE', #39578, .T. ) ;
#23433 = VECTOR ( 'NONE', #50120, 1000.000000000000000 ) ;
#23436 = ORIENTED_EDGE ( 'NONE', *, *, #1460, .T. ) ;
#23435 = DIRECTION ( 'NONE',  ( 0.000000000000000000, 0.000000000000000000, 1.000000000000000000 ) ) ;
#23434 = CARTESIAN_POINT ( 'NONE',  ( -339.1964088526558498, -109.8658467157473666, -57.40522506028092664 ) ) ;
#23437 = CARTESIAN_POINT ( 'NONE',  ( -330.4913330509368166, -123.5000000000000284, 0.000000000000000000 ) ) ;
#23438 = VERTEX_POINT ( 'NONE', #1825 ) ;
#23439 = PLANE ( 'NONE',  #13826 ) ;
#23440 = ORIENTED_EDGE ( 'NONE', *, *, #7048, .T. ) ;
#23441 = CARTESIAN_POINT ( 'NONE',  ( 20.66186849114819069, -189.7472609257535510, -104.1370384486464928 ) ) ;
#23442 = DIRECTION ( 'NONE',  ( -0.5586467658036415873, 0.000000000000000000, -0.8294056854502090959 ) ) ;
#23444 = FACE_OUTER_BOUND ( 'NONE', #16017, .T. ) ;
#23443 = CARTESIAN_POINT ( 'NONE',  ( -336.3521761649654422, -133.2247606357419443, -58.25253621232173629 ) ) ;
#23445 = ADVANCED_FACE ( 'NONE', ( #41782 ), #5533, .T. ) ;
#23446 = EDGE_LOOP ( 'NONE', ( #26356, #19714, #24759, #16834 ) ) ;
#23447 = AXIS2_PLACEMENT_3D ( 'NONE', #29199, #40035, #45501 ) ;
#23448 = EDGE_CURVE ( 'NONE', #24719, #43748, #37579, .T. ) ;
#23449 = FACE_OUTER_BOUND ( 'NONE', #33751, .T. ) ;
#23450 = DIRECTION ( 'NONE',  ( -0.000000000000000000, 1.000000000000000000, -0.000000000000000000 ) ) ;
#23451 = VERTEX_POINT ( 'NONE', #21812 ) ;
#23452 = PLANE ( 'NONE',  #8994 ) ;
#23453 = DIRECTION ( 'NONE',  ( -0.000000000000000000, 1.000000000000000000, -0.000000000000000000 ) ) ;
#23454 = ORIENTED_EDGE ( 'NONE', *, *, #41047, .T. ) ;
#23455 = FACE_OUTER_BOUND ( 'NONE', #43589, .T. ) ;
#23456 = PLANE ( 'NONE',  #2138 ) ;
#23457 = ORIENTED_EDGE ( 'NONE', *, *, #31260, .T. ) ;
#23458 = CARTESIAN_POINT ( 'NONE',  ( -91.84482189527193441, -175.3837268820161057, -117.2365833888816695 ) ) ;
#23459 = VERTEX_POINT ( 'NONE', #29678 ) ;
#23460 = VECTOR ( 'NONE', #49342, 1000.000000000000227 ) ;
#23461 = DIRECTION ( 'NONE',  ( -0.6068001458186002006, 0.000000000000000000, 0.7948544414133481562 ) ) ;
#23462 = CARTESIAN_POINT ( 'NONE',  ( -40.90423906728908321, -193.5000000000000000, -124.7702732086912221 ) ) ;
#23463 = VECTOR ( 'NONE', #32073, 1000.000000000000000 ) ;
#23464 = EDGE_CURVE ( 'NONE', #24906, #41605, #45726, .T. ) ;
#23465 = CARTESIAN_POINT ( 'NONE',  ( -332.3517673607765914, -94.63601285149479736, 51.48334306143172512 ) ) ;
#23466 = CARTESIAN_POINT ( 'NONE',  ( -151.5051191635538146, -183.6283474603465606, -69.00559874123518966 ) ) ;
#23467 = LINE ( 'NONE', #15080, #23243 ) ;
#23468 = EDGE_CURVE ( 'NONE', #3230, #48106, #17864, .T. ) ;
#23469 = EDGE_CURVE ( 'NONE', #20782, #15531, #14194, .T. ) ;
#23470 = LINE ( 'NONE', #15319, #12863 ) ;
#23471 = ADVANCED_FACE ( 'NONE', ( #33107 ), #30209, .T. ) ;
#23472 = DIRECTION ( 'NONE',  ( -0.9995608365087944591, 0.000000000000000000, 0.02963332782255633305 ) ) ;
#23473 = DIRECTION ( 'NONE',  ( -0.000000000000000000, 1.000000000000000000, -0.000000000000000000 ) ) ;
#23475 = ORIENTED_EDGE ( 'NONE', *, *, #2209, .F. ) ;
#23474 = DIRECTION ( 'NONE',  ( 0.000000000000000000, -0.3546048870425463906, -0.9350162426854107256 ) ) ;
#23476 = ORIENTED_EDGE ( 'NONE', *, *, #11280, .F. ) ;
#23477 = LINE ( 'NONE', #43450, #28291 ) ;
#23478 = VECTOR ( 'NONE', #21746, 999.9999999999998863 ) ;
#23479 = CARTESIAN_POINT ( 'NONE',  ( 8.448131207122532516, -193.5000000000000000, 111.2847127925100352 ) ) ;
#23480 = ORIENTED_EDGE ( 'NONE', *, *, #28276, .F. ) ;
#23481 = ORIENTED_EDGE ( 'NONE', *, *, #50884, .T. ) ;
#23482 = FACE_OUTER_BOUND ( 'NONE', #17083, .T. ) ;
#23483 = EDGE_LOOP ( 'NONE', ( #36228, #11293, #4462, #38281 ) ) ;
#23484 = CYLINDRICAL_SURFACE ( 'NONE', #21676, 125.0000000000000000 ) ;
#23485 = CARTESIAN_POINT ( 'NONE',  ( -339.1964088526558498, -182.1300919119129560, -6.615309698014600670 ) ) ;
#23486 = CARTESIAN_POINT ( 'NONE',  ( 13.86276369408137477, -189.7472609257535510, -107.1890582354654526 ) ) ;
#23487 = LINE ( 'NONE', #7709, #16554 ) ;
#23488 = ORIENTED_EDGE ( 'NONE', *, *, #18487, .T. ) ;
#23489 = VERTEX_POINT ( 'NONE', #46250 ) ;
#23490 = EDGE_CURVE ( 'NONE', #51365, #39858, #10229, .T. ) ;
#23491 = EDGE_LOOP ( 'NONE', ( #3205, #23703, #23436, #24760 ) ) ;
#23492 = DIRECTION ( 'NONE',  ( -0.7765238627180482966, 0.000000000000000000, 0.6300878435817038881 ) ) ;
#23493 = DIRECTION ( 'NONE',  ( 0.000000000000000000, -0.000000000000000000, -1.000000000000000000 ) ) ;
#23494 = CARTESIAN_POINT ( 'NONE',  ( -148.0127667507368585, -193.5000000000000000, -75.61781872352626976 ) ) ;
#23495 = AXIS2_PLACEMENT_3D ( 'NONE', #1574, #42273, #6289 ) ;
#23496 = DIRECTION ( 'NONE',  ( -0.000000000000000000, -0.9709418174260502354, 0.2393156642875652051 ) ) ;
#23497 = LINE ( 'NONE', #32144, #44906 ) ;
#23498 = ORIENTED_EDGE ( 'NONE', *, *, #7275, .F. ) ;
#23499 = CARTESIAN_POINT ( 'NONE',  ( 58.95724912996274725, -177.1207230881787780, 61.91627321685103169 ) ) ;
#23500 = CARTESIAN_POINT ( 'NONE',  ( 33.75048693540709621, -175.3837268820161057, 94.14505102712816154 ) ) ;
#23501 = VERTEX_POINT ( 'NONE', #51224 ) ;
#23502 = ORIENTED_EDGE ( 'NONE', *, *, #311, .T. ) ;
#23503 = VERTEX_POINT ( 'NONE', #10480 ) ;
#23504 = CARTESIAN_POINT ( 'NONE',  ( -336.3521761649654422, -123.5000000000000284, 0.000000000000000000 ) ) ;
#23505 = CARTESIAN_POINT ( 'NONE',  ( -138.3705904895685421, -183.6283474603465606, -86.85922373029301014 ) ) ;
#23506 = EDGE_LOOP ( 'NONE', ( #709, #15444, #91, #28185 ) ) ;
#23507 = DIRECTION ( 'NONE',  ( 1.000000000000000000, -0.000000000000000000, -0.000000000000000000 ) ) ;
#23508 = CARTESIAN_POINT ( 'NONE',  ( -336.3521761649654422, -87.81784868886214213, 47.06073758877343494 ) ) ;
#23509 = DIRECTION ( 'NONE',  ( 0.000000000000000000, 0.000000000000000000, -1.000000000000000000 ) ) ;
#23510 = ORIENTED_EDGE ( 'NONE', *, *, #11587, .F. ) ;
#23511 = LINE ( 'NONE', #34304, #41840 ) ;
#23512 = CIRCLE ( 'NONE', #41959, 125.0000000000000000 ) ;
#23513 = VECTOR ( 'NONE', #16701, 1000.000000000000000 ) ;
#23514 = VERTEX_POINT ( 'NONE', #10748 ) ;
#23515 = DIRECTION ( 'NONE',  ( -0.000000000000000000, 1.000000000000000000, -0.000000000000000000 ) ) ;
#23516 = FACE_OUTER_BOUND ( 'NONE', #45433, .T. ) ;
#23517 = VERTEX_POINT ( 'NONE', #34652 ) ;
#23518 = DIRECTION ( 'NONE',  ( 0.3758275821142422202, 0.000000000000000000, -0.9266896074318318188 ) ) ;
#23519 = LINE ( 'NONE', #27970, #46550 ) ;
#23520 = LINE ( 'NONE', #15383, #30707 ) ;
#23521 = ADVANCED_FACE ( 'NONE', ( #26774 ), #50698, .T. ) ;
#23522 = DIRECTION ( 'NONE',  ( -0.6068001458186002006, 0.000000000000000000, 0.7948544414133481562 ) ) ;
#23523 = DIRECTION ( 'NONE',  ( -8.718379230999704661E-17, -0.8229838658936613482, -0.5680647467311485954 ) ) ;
#23524 = ORIENTED_EDGE ( 'NONE', *, *, #12642, .F. ) ;
#23525 = ORIENTED_EDGE ( 'NONE', *, *, #23092, .T. ) ;
#23526 = AXIS2_PLACEMENT_3D ( 'NONE', #10992, #7576, #23596 ) ;
#23527 = DIRECTION ( 'NONE',  ( 0.000000000000000000, 0.6631226582407964143, 0.7485107481710999711 ) ) ;
#23529 = EDGE_LOOP ( 'NONE', ( #47535, #45619, #23112, #41440 ) ) ;
#23528 = DIRECTION ( 'NONE',  ( 0.6528221181905174975, 0.000000000000000000, 0.7575112421616236880 ) ) ;
#23530 = ORIENTED_EDGE ( 'NONE', *, *, #19255, .T. ) ;
#23531 = CARTESIAN_POINT ( 'NONE',  ( -26.53529504715430676, -175.3837268820161057, 123.0587999703026867 ) ) ;
#23532 = DIRECTION ( 'NONE',  ( 0.000000000000000000, 0.000000000000000000, -1.000000000000000000 ) ) ;
#23533 = EDGE_LOOP ( 'NONE', ( #6964, #23010, #2826, #41303 ) ) ;
#23534 = FACE_BOUND ( 'NONE', #14456, .T. ) ;
#23535 = CARTESIAN_POINT ( 'NONE',  ( 46.00000000000000711, 20.00000000000000000, -56.99999999999999289 ) ) ;
#23536 = EDGE_CURVE ( 'NONE', #34048, #19724, #31484, .T. ) ;
#23537 = ORIENTED_EDGE ( 'NONE', *, *, #32654, .F. ) ;
#23538 = LINE ( 'NONE', #32195, #17450 ) ;
#23539 = DIRECTION ( 'NONE',  ( 1.000000000000000000, 0.000000000000000000, -0.000000000000000000 ) ) ;
#23540 = DIRECTION ( 'NONE',  ( -0.9027978299657477557, 0.000000000000000000, 0.4300652022765115712 ) ) ;
#23541 = CARTESIAN_POINT ( 'NONE',  ( -85.77912150413021664, -175.3837268820161057, -119.3051146910911768 ) ) ;
#23542 = VERTEX_POINT ( 'NONE', #14443 ) ;
#23543 = ORIENTED_EDGE ( 'NONE', *, *, #49768, .T. ) ;
#23544 = AXIS2_PLACEMENT_3D ( 'NONE', #21036, #49433, #20249 ) ;
#23546 = ORIENTED_EDGE ( 'NONE', *, *, #18905, .T. ) ;
#23545 = CIRCLE ( 'NONE', #20, 4.000000000000003553 ) ;
#23547 = DIRECTION ( 'NONE',  ( 0.000000000000000000, -1.000000000000000000, -0.000000000000000000 ) ) ;
#23548 = DIRECTION ( 'NONE',  ( -0.000000000000000000, 0.000000000000000000, 1.000000000000000000 ) ) ;
#23549 = FACE_OUTER_BOUND ( 'NONE', #33192, .T. ) ;
#23550 = CARTESIAN_POINT ( 'NONE',  ( -330.4913330509368166, -68.15673923803930734, -20.45418021416698551 ) ) ;
#23551 = DIRECTION ( 'NONE',  ( 1.000000000000000000, -0.000000000000000000, -0.000000000000000000 ) ) ;
#23552 = EDGE_LOOP ( 'NONE', ( #1362, #30044, #30307, #33053 ) ) ;
#23553 = EDGE_CURVE ( 'NONE', #31469, #44223, #31755, .T. ) ;
#23554 = CARTESIAN_POINT ( 'NONE',  ( -170.7635349987907034, -189.7472609257535510, -25.91377046305883169 ) ) ;
#23555 = EDGE_LOOP ( 'NONE', ( #18902, #27415, #20199, #51250 ) ) ;
#23557 = ORIENTED_EDGE ( 'NONE', *, *, #23812, .F. ) ;
#23556 = FACE_OUTER_BOUND ( 'NONE', #20904, .T. ) ;
#23558 = VERTEX_POINT ( 'NONE', #43062 ) ;
#23559 = VECTOR ( 'NONE', #28507, 1000.000000000000000 ) ;
#23560 = EDGE_CURVE ( 'NONE', #47778, #27224, #26510, .T. ) ;
#23561 = DIRECTION ( 'NONE',  ( -0.2059786187410953262, 0.000000000000000000, -0.9785564922995046988 ) ) ;
#23562 = DIRECTION ( 'NONE',  ( 1.043714542225393381E-14, -1.000000000000000000, 3.491481338843133355E-15 ) ) ;
#23563 = DIRECTION ( 'NONE',  ( -0.000000000000000000, 1.000000000000000000, -0.000000000000000000 ) ) ;
#23564 = LINE ( 'NONE', #27756, #3266 ) ;
#23565 = VERTEX_POINT ( 'NONE', #43582 ) ;
#23566 = DIRECTION ( 'NONE',  ( 0.000000000000000000, 0.000000000000000000, -1.000000000000000000 ) ) ;
#23567 = ORIENTED_EDGE ( 'NONE', *, *, #26227, .F. ) ;
#23568 = ADVANCED_FACE ( 'NONE', ( #30973 ), #27548, .F. ) ;
#23569 = ORIENTED_EDGE ( 'NONE', *, *, #6685, .T. ) ;
#23570 = CARTESIAN_POINT ( 'NONE',  ( -91.22542124915045747, -193.5000000000000000, 117.4638425504669783 ) ) ;
#23571 = CARTESIAN_POINT ( 'NONE',  ( -332.3517673607765914, -123.5000000000000284, 0.000000000000000000 ) ) ;
#23572 = DIRECTION ( 'NONE',  ( -0.000000000000000000, -0.6631226582407885317, 0.7485107481711069655 ) ) ;
#23573 = CIRCLE ( 'NONE', #22756, 60.00000000000000000 ) ;
#23574 = DIRECTION ( 'NONE',  ( 0.000000000000000000, 0.000000000000000000, 1.000000000000000000 ) ) ;
#23575 = DIRECTION ( 'NONE',  ( 1.000000000000000000, -0.000000000000000000, -0.000000000000000000 ) ) ;
#23576 = EDGE_CURVE ( 'NONE', #6394, #33644, #6565, .T. ) ;
#23577 = ORIENTED_EDGE ( 'NONE', *, *, #14163, .F. ) ;
#23578 = CARTESIAN_POINT ( 'NONE',  ( -305.0000000000000568, -147.2170408776451609, -55.11353710303946940 ) ) ;
#23579 = FACE_OUTER_BOUND ( 'NONE', #51758, .T. ) ;
#23580 = EDGE_CURVE ( 'NONE', #40297, #47963, #30708, .T. ) ;
#23581 = AXIS2_PLACEMENT_3D ( 'NONE', #50435, #1804, #17847 ) ;
#23582 = CARTESIAN_POINT ( 'NONE',  ( -166.6807411098556031, -177.1207230881787780, 37.47770156625504256 ) ) ;
#23583 = ORIENTED_EDGE ( 'NONE', *, *, #49530, .F. ) ;
#23584 = EDGE_CURVE ( 'NONE', #23845, #38723, #3216, .T. ) ;
#23585 = DIRECTION ( 'NONE',  ( 0.9785564922995032555, 0.000000000000000000, 0.2059786187411021818 ) ) ;
#23586 = CARTESIAN_POINT ( 'NONE',  ( -95.72791768350688812, -193.5000000000000000, -115.7261930397105232 ) ) ;
#23587 = EDGE_LOOP ( 'NONE', ( #49536, #11693, #16139, #19416 ) ) ;
#23588 = LINE ( 'NONE', #44861, #32969 ) ;
#23589 = ORIENTED_EDGE ( 'NONE', *, *, #14695, .T. ) ;
#23590 = DIRECTION ( 'NONE',  ( -0.000000000000000000, 1.000000000000000000, -0.000000000000000000 ) ) ;
#23591 = VECTOR ( 'NONE', #1107, 1000.000000000000000 ) ;
#23592 = FACE_BOUND ( 'NONE', #17563, .T. ) ;
#23594 = ORIENTED_EDGE ( 'NONE', *, *, #36455, .T. ) ;
#23593 = DIRECTION ( 'NONE',  ( -1.000000000000000000, 0.000000000000000000, -0.000000000000000000 ) ) ;
#23595 = EDGE_CURVE ( 'NONE', #13008, #47040, #47017, .T. ) ;
#23596 = DIRECTION ( 'NONE',  ( 0.000000000000000000, 0.000000000000000000, 1.000000000000000000 ) ) ;
#23597 = EDGE_CURVE ( 'NONE', #33930, #46522, #32579, .T. ) ;
#23598 = ORIENTED_EDGE ( 'NONE', *, *, #5927, .T. ) ;
#23599 = ORIENTED_EDGE ( 'NONE', *, *, #23410, .T. ) ;
#23600 = CARTESIAN_POINT ( 'NONE',  ( -47.63353074800703268, -189.7472609257535510, 0.5338233779648018373 ) ) ;
#23601 = ORIENTED_EDGE ( 'NONE', *, *, #5033, .F. ) ;
#23602 = CARTESIAN_POINT ( 'NONE',  ( -48.02249751411514467, -177.1207230881787780, 0.8896570909947569827 ) ) ;
#23603 = AXIS2_PLACEMENT_3D ( 'NONE', #34321, #44277, #51922 ) ;
#23604 = CARTESIAN_POINT ( 'NONE',  ( 64.01121016852529522, -175.3837268820161057, -54.50618404930953176 ) ) ;
#23605 = DIRECTION ( 'NONE',  ( -0.000000000000000000, 1.000000000000000000, -0.000000000000000000 ) ) ;
#23606 = ORIENTED_EDGE ( 'NONE', *, *, #2922, .F. ) ;
#23608 = VERTEX_POINT ( 'NONE', #10995 ) ;
#23607 = DIRECTION ( 'NONE',  ( 0.8124868780056783146, 0.000000000000000000, 0.5829794791144762289 ) ) ;
#23609 = VERTEX_POINT ( 'NONE', #27021 ) ;
#23610 = DIRECTION ( 'NONE',  ( -0.2059786187410953262, 0.000000000000000000, -0.9785564922995046988 ) ) ;
#23611 = ORIENTED_EDGE ( 'NONE', *, *, #10235, .F. ) ;
#23612 = PLANE ( 'NONE',  #31476 ) ;
#23613 = ORIENTED_EDGE ( 'NONE', *, *, #43974, .F. ) ;
#23614 = EDGE_CURVE ( 'NONE', #44188, #28946, #30896, .T. ) ;
#23615 = EDGE_CURVE ( 'NONE', #21465, #31069, #23093, .T. ) ;
#23616 = CYLINDRICAL_SURFACE ( 'NONE', #31764, 125.0000000000000000 ) ;
#23617 = EDGE_LOOP ( 'NONE', ( #14269, #35984, #43533, #17603 ) ) ;
#23619 = DIRECTION ( 'NONE',  ( -1.000000000000000000, 0.000000000000000000, 0.000000000000000000 ) ) ;
#23618 = CARTESIAN_POINT ( 'NONE',  ( 29.90148147319962035, -193.5000000000000000, 96.08646119224012239 ) ) ;
#23620 = ORIENTED_EDGE ( 'NONE', *, *, #19214, .F. ) ;
#23621 = AXIS2_PLACEMENT_3D ( 'NONE', #1805, #29926, #9975 ) ;
#23622 = DIRECTION ( 'NONE',  ( 0.000000000000000000, 7.170190367370802131E-15, 1.000000000000000000 ) ) ;
#23623 = ORIENTED_EDGE ( 'NONE', *, *, #17666, .F. ) ;
#23624 = CARTESIAN_POINT ( 'NONE',  ( -124.3803110981236273, -175.3837268820161057, -98.05618656931940791 ) ) ;
#23626 = AXIS2_PLACEMENT_3D ( 'NONE', #15536, #12559, #36458 ) ;
#23625 = DIRECTION ( 'NONE',  ( -0.000000000000000000, 1.000000000000000000, -1.047444401652940007E-14 ) ) ;
#23627 = DIRECTION ( 'NONE',  ( 0.7765238627180482966, 0.000000000000000000, -0.6300878435817038881 ) ) ;
#23628 = LINE ( 'NONE', #34434, #51731 ) ;
#23629 = DIRECTION ( 'NONE',  ( 0.000000000000000000, 1.000000000000000000, 0.000000000000000000 ) ) ;
#23630 = DIRECTION ( 'NONE',  ( -0.000000000000000000, 0.5680647467311625842, 0.8229838658936516893 ) ) ;
#23631 = ORIENTED_EDGE ( 'NONE', *, *, #29692, .T. ) ;
#23632 = DIRECTION ( 'NONE',  ( 1.000000000000000000, 0.000000000000000000, 0.000000000000000000 ) ) ;
#23633 = ADVANCED_FACE ( 'NONE', ( #34905 ), #31226, .F. ) ;
#23634 = DIRECTION ( 'NONE',  ( 0.1476465640024710868, 0.000000000000000000, 0.9890401873221654760 ) ) ;
#23635 = CARTESIAN_POINT ( 'NONE',  ( -48.24424070572787571, -193.5000000000000000, 0.9720229140804191870 ) ) ;
#23636 = EDGE_CURVE ( 'NONE', #25951, #38237, #15212, .T. ) ;
#23637 = CARTESIAN_POINT ( 'NONE',  ( -49.40581635894069024, -175.3837268820161057, 0.3758275821142362250 ) ) ;
#23638 = ORIENTED_EDGE ( 'NONE', *, *, #44973, .F. ) ;
#23639 = EDGE_CURVE ( 'NONE', #32593, #2592, #50451, .T. ) ;
#23640 = DIRECTION ( 'NONE',  ( 0.000000000000000000, 0.9709418174260526779, 0.2393156642875547968 ) ) ;
#23641 = AXIS2_PLACEMENT_3D ( 'NONE', #5827, #13686, #36827 ) ;
#23642 = EDGE_CURVE ( 'NONE', #34175, #8967, #4913, .T. ) ;
#23643 = CARTESIAN_POINT ( 'NONE',  ( 30.50828161901820224, -177.1207230881787780, 96.88131563365348597 ) ) ;
#23645 = EDGE_LOOP ( 'NONE', ( #37978, #34907, #40318, #36223 ) ) ;
#23644 = DIRECTION ( 'NONE',  ( 0.000000000000000000, 0.000000000000000000, 1.000000000000000000 ) ) ;
#23646 = VERTEX_POINT ( 'NONE', #31998 ) ;
#23647 = VECTOR ( 'NONE', #48008, 1000.000000000000000 ) ;
#23648 = ORIENTED_EDGE ( 'NONE', *, *, #48139, .F. ) ;
#23649 = AXIS2_PLACEMENT_3D ( 'NONE', #31279, #27602, #11299 ) ;
#23650 = DIRECTION ( 'NONE',  ( 1.000000000000000000, 0.000000000000000000, -0.000000000000000000 ) ) ;
#23651 = DIRECTION ( 'NONE',  ( -0.4566292373937077542, 0.000000000000000000, -0.8896570909947499883 ) ) ;
#23652 = CARTESIAN_POINT ( 'NONE',  ( -49.30901192927175458, -175.3837268820161057, -124.9972451320097093 ) ) ;
#23653 = DIRECTION ( 'NONE',  ( 1.000000000000000000, -0.000000000000000000, -0.000000000000000000 ) ) ;
#23654 = ORIENTED_EDGE ( 'NONE', *, *, #31519, .F. ) ;
#23655 = FACE_OUTER_BOUND ( 'NONE', #4027, .T. ) ;
#23656 = VECTOR ( 'NONE', #16885, 1000.000000000000000 ) ;
#23657 = ORIENTED_EDGE ( 'NONE', *, *, #34498, .F. ) ;
#23658 = VECTOR ( 'NONE', #23794, 1000.000000000000000 ) ;
#23659 = ORIENTED_EDGE ( 'NONE', *, *, #24362, .T. ) ;
#23660 = VECTOR ( 'NONE', #45613, 999.9999999999998863 ) ;
#23661 = ORIENTED_EDGE ( 'NONE', *, *, #17963, .F. ) ;
#23662 = PLANE ( 'NONE',  #36783 ) ;
#23663 = VERTEX_POINT ( 'NONE', #32255 ) ;
#23664 = DIRECTION ( 'NONE',  ( 0.000000000000000000, 0.8854560256532110207, 0.4647231720437664526 ) ) ;
#23665 = DIRECTION ( 'NONE',  ( 0.2920567706369694982, 0.000000000000000000, 0.9564009842765243130 ) ) ;
#23668 = VERTEX_POINT ( 'NONE', #36453 ) ;
#23667 = LINE ( 'NONE', #31042, #14896 ) ;
#23666 = DIRECTION ( 'NONE',  ( -0.000000000000000000, 1.000000000000000000, -0.000000000000000000 ) ) ;
#23669 = EDGE_CURVE ( 'NONE', #18052, #34792, #49410, .T. ) ;
#23670 = CARTESIAN_POINT ( 'NONE',  ( -38.66762320617017679, -193.5000000000000000, -124.6143426664033740 ) ) ;
#23671 = ORIENTED_EDGE ( 'NONE', *, *, #51586, .F. ) ;
#23672 = FACE_OUTER_BOUND ( 'NONE', #46120, .T. ) ;
#23673 = AXIS2_PLACEMENT_3D ( 'NONE', #39899, #24167, #36480 ) ;
#23674 = ORIENTED_EDGE ( 'NONE', *, *, #42679, .T. ) ;
#23675 = EDGE_CURVE ( 'NONE', #17110, #33465, #27792, .T. ) ;
#23676 = EDGE_CURVE ( 'NONE', #32651, #46212, #19924, .T. ) ;
#23677 = EDGE_CURVE ( 'NONE', #41991, #43010, #24910, .T. ) ;
#23678 = DIRECTION ( 'NONE',  ( 0.000000000000000000, 1.000000000000000000, 1.346129392433909288E-16 ) ) ;
#23679 = DIRECTION ( 'NONE',  ( 0.000000000000000000, 0.000000000000000000, 1.000000000000000000 ) ) ;
#23681 = LINE ( 'NONE', #43663, #13070 ) ;
#23680 = CARTESIAN_POINT ( 'NONE',  ( -170.7635349987907603, -175.3837268820161057, -25.91377046305877130 ) ) ;
#23682 = VERTEX_POINT ( 'NONE', #48041 ) ;
#23683 = ADVANCED_FACE ( 'NONE', ( #44091 ), #51739, .F. ) ;
#23684 = AXIS2_PLACEMENT_3D ( 'NONE', #33872, #30201, #30439 ) ;
#23685 = DIRECTION ( 'NONE',  ( 0.000000000000000000, 0.000000000000000000, 1.000000000000000000 ) ) ;
#23686 = CARTESIAN_POINT ( 'NONE',  ( -172.5669052183642407, -177.1207230881787780, 15.07392567185553744 ) ) ;
#23687 = CARTESIAN_POINT ( 'NONE',  ( -339.1964088526558498, -182.5000000000000568, -0.4999999999999543698 ) ) ;
#23688 = ORIENTED_EDGE ( 'NONE', *, *, #20786, .T. ) ;
#23689 = EDGE_CURVE ( 'NONE', #34695, #48626, #42673, .T. ) ;
#23690 = CARTESIAN_POINT ( 'NONE',  ( -336.3521761649654422, -66.60506506233235768, -15.70448169564047092 ) ) ;
#23691 = DIRECTION ( 'NONE',  ( 0.000000000000000000, -1.811051308919786607E-13, 1.000000000000000000 ) ) ;
#23692 = EDGE_CURVE ( 'NONE', #21919, #38136, #12021, .T. ) ;
#23693 = CARTESIAN_POINT ( 'NONE',  ( 73.80528149577284580, -189.7472609257535510, 25.91377046305970211 ) ) ;
#23694 = VERTEX_POINT ( 'NONE', #35957 ) ;
#23695 = DIRECTION ( 'NONE',  ( 0.000000000000000000, 0.000000000000000000, 1.000000000000000000 ) ) ;
#23696 = EDGE_CURVE ( 'NONE', #1758, #2274, #39871, .T. ) ;
#23697 = VECTOR ( 'NONE', #51276, 999.9999999999998863 ) ;
#23699 = AXIS2_PLACEMENT_3D ( 'NONE', #9040, #16678, #20077 ) ;
#23698 = DIRECTION ( 'NONE',  ( 0.000000000000000000, -1.000000000000000000, 0.000000000000000000 ) ) ;
#23700 = EDGE_CURVE ( 'NONE', #34751, #37802, #12287, .T. ) ;
#23701 = ORIENTED_EDGE ( 'NONE', *, *, #12492, .F. ) ;
#23702 = DIRECTION ( 'NONE',  ( 1.000000000000000000, 0.000000000000000000, 0.000000000000000000 ) ) ;
#23703 = ORIENTED_EDGE ( 'NONE', *, *, #13331, .F. ) ;
#23704 = VECTOR ( 'NONE', #23575, 1000.000000000000000 ) ;
#23705 = AXIS2_PLACEMENT_3D ( 'NONE', #17191, #45058, #21909 ) ;
#23706 = EDGE_CURVE ( 'NONE', #5333, #42630, #44370, .T. ) ;
#23707 = LINE ( 'NONE', #27901, #34850 ) ;
#23708 = DIRECTION ( 'NONE',  ( 0.000000000000000000, -1.000000000000000000, 0.000000000000000000 ) ) ;
#23709 = EDGE_CURVE ( 'NONE', #4036, #13526, #3254, .T. ) ;
#23710 = CARTESIAN_POINT ( 'NONE',  ( -170.0000000000000284, -113.5000000000000142, -60.00000000000001421 ) ) ;
#23711 = LINE ( 'NONE', #19760, #7958 ) ;
#23712 = CARTESIAN_POINT ( 'NONE',  ( 45.36094686508022988, -183.6283474603465606, -82.57748230379236531 ) ) ;
#23713 = EDGE_CURVE ( 'NONE', #46918, #48966, #15991, .T. ) ;
#23714 = CARTESIAN_POINT ( 'NONE',  ( -50.89116676070551648, -193.5000000000000000, 124.9767260852757147 ) ) ;
#23715 = DIRECTION ( 'NONE',  ( -0.000000000000000000, 1.000000000000000000, -0.000000000000000000 ) ) ;
#23716 = CARTESIAN_POINT ( 'NONE',  ( -127.0132498732366457, -183.6283474603465606, 97.24912084693259828 ) ) ;
#23718 = ORIENTED_EDGE ( 'NONE', *, *, #14346, .F. ) ;
#23717 = CARTESIAN_POINT ( 'NONE',  ( -48.98765787015808115, -193.5000000000000000, 0.8610436117673582190 ) ) ;
#23719 = CIRCLE ( 'NONE', #5287, 60.00000000000000000 ) ;
#23720 = EDGE_LOOP ( 'NONE', ( #2041, #1654, #29418, #46674 ) ) ;
#23721 = FACE_OUTER_BOUND ( 'NONE', #8627, .T. ) ;
#23722 = ADVANCED_FACE ( 'NONE', ( #8098 ), #8360, .T. ) ;
#23723 = VECTOR ( 'NONE', #16295, 1000.000000000000000 ) ;
#23724 = FACE_OUTER_BOUND ( 'NONE', #23078, .T. ) ;
#23725 = ORIENTED_EDGE ( 'NONE', *, *, #15648, .T. ) ;
#23726 = VERTEX_POINT ( 'NONE', #40648 ) ;
#23727 = PLANE ( 'NONE',  #8833 ) ;
#23728 = EDGE_LOOP ( 'NONE', ( #36581, #51443, #4250, #20720 ) ) ;
#23729 = DIRECTION ( 'NONE',  ( -0.000000000000000000, 1.000000000000000000, 0.000000000000000000 ) ) ;
#23730 = FACE_OUTER_BOUND ( 'NONE', #21619, .T. ) ;
#23731 = CARTESIAN_POINT ( 'NONE',  ( -111.8989814360438828, -175.3837268820161057, -107.7168604805787027 ) ) ;
#23732 = CARTESIAN_POINT ( 'NONE',  ( -124.4642912599203726, -193.5000000000000000, 99.25348746834863789 ) ) ;
#23734 = VERTEX_POINT ( 'NONE', #4410 ) ;
#23733 = AXIS2_PLACEMENT_3D ( 'NONE', #41540, #25519, #1865 ) ;
#23735 = AXIS2_PLACEMENT_3D ( 'NONE', #15982, #36448, #44609 ) ;
#23736 = VERTEX_POINT ( 'NONE', #16510 ) ;
#23737 = VERTEX_POINT ( 'NONE', #8603 ) ;
#23738 = ADVANCED_FACE ( 'NONE', ( #32526 ), #48578, .T. ) ;
#23739 = CARTESIAN_POINT ( 'NONE',  ( 0.000000000000000000, -137.6196241929653752, 57.28556722813723212 ) ) ;
#23740 = CARTESIAN_POINT ( 'NONE',  ( -332.3517673607765914, -179.5993808087905279, -18.46045550523168899 ) ) ;
#23741 = AXIS2_PLACEMENT_3D ( 'NONE', #46945, #39021, #39791 ) ;
#23742 = CARTESIAN_POINT ( 'NONE',  ( -336.3521761649654422, -85.59754891220836726, -45.24454186338619621 ) ) ;
#23743 = AXIS2_PLACEMENT_3D ( 'NONE', #6347, #2404, #22367 ) ;
#23744 = CARTESIAN_POINT ( 'NONE',  ( 76.09804998693969935, -189.7472609257535510, 10.27263529369908746 ) ) ;
#23745 = FACE_OUTER_BOUND ( 'NONE', #51053, .T. ) ;
#23746 = EDGE_LOOP ( 'NONE', ( #10254, #24876, #28851, #11007 ) ) ;
#23747 = PLANE ( 'NONE',  #23831 ) ;
#23748 = EDGE_CURVE ( 'NONE', #32802, #16247, #4671, .T. ) ;
#23749 = EDGE_CURVE ( 'NONE', #7602, #11338, #12803, .T. ) ;
#23750 = EDGE_CURVE ( 'NONE', #33090, #41579, #28402, .T. ) ;
#23751 = VECTOR ( 'NONE', #29147, 1000.000000000000000 ) ;
#23752 = DIRECTION ( 'NONE',  ( 0.000000000000000000, 1.000000000000000000, -0.000000000000000000 ) ) ;
#23753 = FACE_OUTER_BOUND ( 'NONE', #24334, .T. ) ;
#23754 = EDGE_CURVE ( 'NONE', #21574, #21379, #25424, .T. ) ;
#23755 = ORIENTED_EDGE ( 'NONE', *, *, #5807, .T. ) ;
#23756 = ORIENTED_EDGE ( 'NONE', *, *, #18392, .T. ) ;
#23757 = EDGE_LOOP ( 'NONE', ( #25516, #26616, #45976, #48564 ) ) ;
#23758 = CARTESIAN_POINT ( 'NONE',  ( -115.4536696835167930, -183.6283474603465606, -105.5434062319793895 ) ) ;
#23759 = DIRECTION ( 'NONE',  ( 0.4031234292879665171, 0.000000000000000000, 0.9151456172430210145 ) ) ;
#23760 = ORIENTED_EDGE ( 'NONE', *, *, #45533, .F. ) ;
#23761 = CARTESIAN_POINT ( 'NONE',  ( -155.0851258170080484, -193.5000000000000000, 63.33473559879990233 ) ) ;
#23762 = VECTOR ( 'NONE', #51261, 1000.000000000000000 ) ;
#23763 = FACE_OUTER_BOUND ( 'NONE', #46784, .T. ) ;
#23764 = FACE_OUTER_BOUND ( 'NONE', #8214, .T. ) ;
#23765 = VERTEX_POINT ( 'NONE', #45157 ) ;
#23766 = DIRECTION ( 'NONE',  ( -0.000000000000000000, 1.000000000000000000, -0.000000000000000000 ) ) ;
#23767 = AXIS2_PLACEMENT_3D ( 'NONE', #11885, #28434, #16637 ) ;
#23768 = VERTEX_POINT ( 'NONE', #5726 ) ;
#23769 = DIRECTION ( 'NONE',  ( -1.000000000000000000, 0.000000000000000000, 0.000000000000000000 ) ) ;
#23770 = FACE_BOUND ( 'NONE', #22542, .T. ) ;
#23771 = EDGE_CURVE ( 'NONE', #30123, #14634, #17556, .T. ) ;
#23772 = LINE ( 'NONE', #19819, #42107 ) ;
#23773 = ORIENTED_EDGE ( 'NONE', *, *, #29380, .F. ) ;
#23774 = EDGE_CURVE ( 'NONE', #25657, #39370, #36000, .T. ) ;
#23775 = LINE ( 'NONE', #44002, #49185 ) ;
#23776 = FACE_OUTER_BOUND ( 'NONE', #4997, .T. ) ;
#23777 = DIRECTION ( 'NONE',  ( -0.05924062789370748011, 0.000000000000000000, -0.9982437317643217956 ) ) ;
#23778 = VECTOR ( 'NONE', #38431, 1000.000000000000000 ) ;
#23779 = CARTESIAN_POINT ( 'NONE',  ( -305.0000000000000568, -183.0001959263614424, -7.728304129924262078 ) ) ;
#23780 = EDGE_CURVE ( 'NONE', #30279, #27547, #29612, .T. ) ;
#23781 = ORIENTED_EDGE ( 'NONE', *, *, #30508, .F. ) ;
#23782 = DIRECTION ( 'NONE',  ( 0.000000000000000000, -0.9350162426854107256, 0.3546048870425463906 ) ) ;
#23783 = ORIENTED_EDGE ( 'NONE', *, *, #2739, .T. ) ;
#23784 = ORIENTED_EDGE ( 'NONE', *, *, #36933, .F. ) ;
#23785 = AXIS2_PLACEMENT_3D ( 'NONE', #35284, #47124, #51578 ) ;
#23787 = VERTEX_POINT ( 'NONE', #36988 ) ;
#23786 = DIRECTION ( 'NONE',  ( 0.000000000000000000, -1.000000000000000000, 0.000000000000000000 ) ) ;
#23788 = ORIENTED_EDGE ( 'NONE', *, *, #46082, .F. ) ;
#23789 = LINE ( 'NONE', #39796, #14005 ) ;
#23790 = AXIS2_PLACEMENT_3D ( 'NONE', #45913, #21978, #25659 ) ;
#23791 = LINE ( 'NONE', #382, #21813 ) ;
#23792 = ORIENTED_EDGE ( 'NONE', *, *, #24215, .F. ) ;
#23793 = CARTESIAN_POINT ( 'NONE',  ( -1.771278280434274155, -183.6283474603465606, -115.9455772817710226 ) ) ;
#23794 = DIRECTION ( 'NONE',  ( 0.000000000000000000, -1.000000000000000000, 1.541976423090494894E-16 ) ) ;
#23795 = ORIENTED_EDGE ( 'NONE', *, *, #47074, .F. ) ;
#23796 = DIRECTION ( 'NONE',  ( -0.000000000000000000, 1.000000000000000000, -0.000000000000000000 ) ) ;
#23797 = DIRECTION ( 'NONE',  ( 0.000000000000000000, 0.000000000000000000, -1.000000000000000000 ) ) ;
#23798 = VECTOR ( 'NONE', #11490, 1000.000000000000114 ) ;
#23799 = DIRECTION ( 'NONE',  ( -0.000000000000000000, 1.000000000000000000, -0.000000000000000000 ) ) ;
#23800 = CARTESIAN_POINT ( 'NONE',  ( -48.47912675150885065, -189.7472609257535510, 6.938893903907228378E-15 ) ) ;
#23801 = ORIENTED_EDGE ( 'NONE', *, *, #11751, .T. ) ;
#23802 = ORIENTED_EDGE ( 'NONE', *, *, #12406, .T. ) ;
#23803 = CIRCLE ( 'NONE', #32202, 125.0000000000000000 ) ;
#23804 = ORIENTED_EDGE ( 'NONE', *, *, #12799, .T. ) ;
#23805 = CARTESIAN_POINT ( 'NONE',  ( 64.01121016852529522, -175.3837268820161057, -54.50618404930953176 ) ) ;
#23806 = CARTESIAN_POINT ( 'NONE',  ( -135.4258661347518853, -193.5000000000000000, -89.80681772907007598 ) ) ;
#23807 = CARTESIAN_POINT ( 'NONE',  ( -23.99795575808071035, -183.6283474603465606, -122.5792489240757703 ) ) ;
#23808 = LINE ( 'NONE', #11199, #13580 ) ;
#23809 = FACE_OUTER_BOUND ( 'NONE', #7082, .T. ) ;
#23810 = VERTEX_POINT ( 'NONE', #33819 ) ;
#23811 = ADVANCED_FACE ( 'NONE', ( #41961 ), #1761, .T. ) ;
#23812 = EDGE_CURVE ( 'NONE', #38465, #2804, #25096, .T. ) ;
#23813 = AXIS2_PLACEMENT_3D ( 'NONE', #9352, #36687, #5415 ) ;
#23814 = LINE ( 'NONE', #11461, #14889 ) ;
#23815 = ORIENTED_EDGE ( 'NONE', *, *, #20182, .F. ) ;
#23817 = EDGE_LOOP ( 'NONE', ( #1180, #25735, #43379, #38615 ) ) ;
#23816 = DIRECTION ( 'NONE',  ( -0.000000000000000000, 1.000000000000000000, -0.000000000000000000 ) ) ;
#23818 = ORIENTED_EDGE ( 'NONE', *, *, #22420, .T. ) ;
#23819 = DIRECTION ( 'NONE',  ( 0.000000000000000000, -1.000000000000000000, 0.000000000000000000 ) ) ;
#23820 = DIRECTION ( 'NONE',  ( 1.000000000000000000, 1.043714542225393381E-14, 0.000000000000000000 ) ) ;
#23821 = DIRECTION ( 'NONE',  ( 0.7378332790417285736, 0.000000000000000000, -0.6749830015182091136 ) ) ;
#23822 = CARTESIAN_POINT ( 'NONE',  ( 74.68865188374466868, -183.6283474603465606, 14.34663989163627740 ) ) ;
#23823 = EDGE_LOOP ( 'NONE', ( #46511, #34342, #40843, #19291 ) ) ;
#23824 = DIRECTION ( 'NONE',  ( 0.000000000000000000, 0.000000000000000000, -1.000000000000000000 ) ) ;
#23825 = ORIENTED_EDGE ( 'NONE', *, *, #24240, .T. ) ;
#23826 = ORIENTED_EDGE ( 'NONE', *, *, #20141, .T. ) ;
#23827 = DIRECTION ( 'NONE',  ( -0.000000000000000000, 1.000000000000000000, -0.000000000000000000 ) ) ;
#23828 = ADVANCED_FACE ( 'NONE', ( #21481, #33041, #49352 ), #41181, .T. ) ;
#23829 = FACE_OUTER_BOUND ( 'NONE', #48465, .T. ) ;
#23830 = DIRECTION ( 'NONE',  ( 0.000000000000000000, 0.000000000000000000, 1.000000000000000000 ) ) ;
#23831 = AXIS2_PLACEMENT_3D ( 'NONE', #7970, #20313, #31628 ) ;
#23832 = DIRECTION ( 'NONE',  ( -1.000000000000000000, -0.000000000000000000, -0.000000000000000000 ) ) ;
#23833 = AXIS2_PLACEMENT_3D ( 'NONE', #2107, #34433, #46281 ) ;
#23834 = CARTESIAN_POINT ( 'NONE',  ( -47.57632892154310866, -193.5000000000000000, -0.4300652022765113491 ) ) ;
#23835 = CARTESIAN_POINT ( 'NONE',  ( -153.7332855749581881, -175.3837268820161057, 67.42819922234392038 ) ) ;
#23836 = ORIENTED_EDGE ( 'NONE', *, *, #37247, .T. ) ;
#23837 = CARTESIAN_POINT ( 'NONE',  ( -336.3521761649654422, -168.7445418633863596, -37.90245108779149064 ) ) ;
#23838 = DIRECTION ( 'NONE',  ( -0.000000000000000000, 1.000000000000000000, -0.000000000000000000 ) ) ;
#23839 = AXIS2_PLACEMENT_3D ( 'NONE', #13829, #5176, #25397 ) ;
#23840 = EDGE_CURVE ( 'NONE', #1636, #33208, #8274, .T. ) ;
#23841 = FACE_BOUND ( 'NONE', #35041, .T. ) ;
#23842 = EDGE_LOOP ( 'NONE', ( #18118, #51336, #41735, #48002 ) ) ;
#23843 = DIRECTION ( 'NONE',  ( 0.000000000000000000, -0.000000000000000000, 1.000000000000000000 ) ) ;
#23844 = CARTESIAN_POINT ( 'NONE',  ( -49.47517659412406488, -193.5000000000000000, -0.08879589532293878651 ) ) ;
#23845 = VERTEX_POINT ( 'NONE', #29094 ) ;
#23846 = CARTESIAN_POINT ( 'NONE',  ( -148.0127667507368585, -183.6283474603465606, -75.61781872352626976 ) ) ;
#23847 = AXIS2_PLACEMENT_3D ( 'NONE', #14377, #46190, #35120 ) ;
#23848 = ORIENTED_EDGE ( 'NONE', *, *, #4359, .T. ) ;
#23849 = CARTESIAN_POINT ( 'NONE',  ( -46.06708674231130374, -177.1207230881787780, -124.9767260852756863 ) ) ;
#23850 = FACE_BOUND ( 'NONE', #22037, .T. ) ;
#23851 = FACE_OUTER_BOUND ( 'NONE', #45912, .T. ) ;
#23852 = LINE ( 'NONE', #19398, #50397 ) ;
#23853 = EDGE_LOOP ( 'NONE', ( #23855, #32607, #40968, #4425 ) ) ;
#23854 = EDGE_CURVE ( 'NONE', #15236, #46340, #13856, .T. ) ;
#23855 = ORIENTED_EDGE ( 'NONE', *, *, #33675, .F. ) ;
#23856 = DIRECTION ( 'NONE',  ( 0.000000000000000000, 0.000000000000000000, 1.000000000000000000 ) ) ;
#23857 = ORIENTED_EDGE ( 'NONE', *, *, #51350, .F. ) ;
#23858 = CARTESIAN_POINT ( 'NONE',  ( -132.6364218684650211, -193.5000000000000000, 92.42591454022807795 ) ) ;
#23859 = FACE_OUTER_BOUND ( 'NONE', #46867, .T. ) ;
#23860 = AXIS2_PLACEMENT_3D ( 'NONE', #18669, #11022, #18919 ) ;
#23861 = EDGE_CURVE ( 'NONE', #14309, #3034, #37650, .T. ) ;
#23862 = VECTOR ( 'NONE', #37412, 1000.000000000000000 ) ;
#23863 = CARTESIAN_POINT ( 'NONE',  ( 41.00573479224733120, -177.1207230881787780, -87.27805883780175122 ) ) ;
#23864 = CARTESIAN_POINT ( 'NONE',  ( -336.3521761649654422, -181.4155151828941825, -11.56382487286496463 ) ) ;
#23865 = ORIENTED_EDGE ( 'NONE', *, *, #40338, .F. ) ;
#23868 = ORIENTED_EDGE ( 'NONE', *, *, #23233, .T. ) ;
#23867 = CARTESIAN_POINT ( 'NONE',  ( -332.3517673607765914, -123.5000000000000284, 0.000000000000000000 ) ) ;
#23866 = CYLINDRICAL_SURFACE ( 'NONE', #26702, 16.00000000000000000 ) ;
#23869 = ADVANCED_FACE ( 'NONE', ( #17287 ), #10164, .F. ) ;
#23870 = ORIENTED_EDGE ( 'NONE', *, *, #52008, .F. ) ;
#23871 = DIRECTION ( 'NONE',  ( -0.000000000000000000, 0.1205366802553199113, -0.9927088740980544168 ) ) ;
#23872 = VERTEX_POINT ( 'NONE', #20969 ) ;
#23873 = CARTESIAN_POINT ( 'NONE',  ( -167.9436818089035057, -193.5000000000000000, 36.78613984830044359 ) ) ;
#23874 = VERTEX_POINT ( 'NONE', #29356 ) ;
#23875 = CARTESIAN_POINT ( 'NONE',  ( -56.05401443572774411, -175.3837268820161057, 124.7702732086912931 ) ) ;
#23876 = ORIENTED_EDGE ( 'NONE', *, *, #35175, .T. ) ;
#23878 = CARTESIAN_POINT ( 'NONE',  ( -140.1460956102404509, -189.7472609257535510, 84.98333260264821831 ) ) ;
#23877 = DIRECTION ( 'NONE',  ( -8.718379230999705894E-17, -0.8854560256532044704, 0.4647231720437789981 ) ) ;
#23879 = AXIS2_PLACEMENT_3D ( 'NONE', #50139, #6236, #6760 ) ;
#23880 = VERTEX_POINT ( 'NONE', #45407 ) ;
#23881 = CYLINDRICAL_SURFACE ( 'NONE', #50914, 10.99999999999999645 ) ;
#23882 = EDGE_LOOP ( 'NONE', ( #48686, #7055, #51724, #49667 ) ) ;
#23883 = DIRECTION ( 'NONE',  ( 0.05924062789370006937, 0.000000000000000000, 0.9982437317643222396 ) ) ;
#23884 = DIRECTION ( 'NONE',  ( 0.8294056854502049880, 0.000000000000000000, -0.5586467658036476935 ) ) ;
#23885 = EDGE_CURVE ( 'NONE', #5747, #25612, #45246, .T. ) ;
#23886 = PLANE ( 'NONE',  #11253 ) ;
#23887 = PLANE ( 'NONE',  #16586 ) ;
#23888 = CARTESIAN_POINT ( 'NONE',  ( 5.015379008610418410, -177.1207230881787780, -112.9749434763326690 ) ) ;
#23889 = CARTESIAN_POINT ( 'NONE',  ( 17.15229921100054611, -183.6283474603465606, -106.3838142112212921 ) ) ;
#23890 = ORIENTED_EDGE ( 'NONE', *, *, #48225, .T. ) ;
#23891 = DIRECTION ( 'NONE',  ( -0.000000000000000000, 0.8854560256532110207, 0.4647231720437664526 ) ) ;
#23892 = LINE ( 'NONE', #24422, #13933 ) ;
#23893 = DIRECTION ( 'NONE',  ( 0.2348860457809911206, 0.000000000000000000, -0.9720229140804089729 ) ) ;
#23894 = VERTEX_POINT ( 'NONE', #14127 ) ;
#23895 = VECTOR ( 'NONE', #40423, 1000.000000000000000 ) ;
#23896 = CARTESIAN_POINT ( 'NONE',  ( -46.00000000000000711, 20.00000000000000000, -41.00000000000000000 ) ) ;
#23897 = VECTOR ( 'NONE', #15547, 1000.000000000000000 ) ;
#23898 = VECTOR ( 'NONE', #47384, 1000.000000000000000 ) ;
#23899 = DIRECTION ( 'NONE',  ( -1.000000000000000000, -0.000000000000000000, -0.000000000000000000 ) ) ;
#23900 = CARTESIAN_POINT ( 'NONE',  ( -336.3521761649654422, -65.82380048139334860, 12.53476669029061519 ) ) ;
#23901 = ORIENTED_EDGE ( 'NONE', *, *, #10082, .F. ) ;
#23902 = ORIENTED_EDGE ( 'NONE', *, *, #47853, .T. ) ;
#23903 = ORIENTED_EDGE ( 'NONE', *, *, #50961, .T. ) ;
#23904 = AXIS2_PLACEMENT_3D ( 'NONE', #40765, #38061, #20818 ) ;
#23905 = CARTESIAN_POINT ( 'NONE',  ( -332.3517673607765914, -181.4155151828941825, -11.56382487286496463 ) ) ;
#23906 = DIRECTION ( 'NONE',  ( 0.000000000000000000, 0.000000000000000000, -1.000000000000000000 ) ) ;
#23907 = CIRCLE ( 'NONE', #20538, 125.0000000000000000 ) ;
#23908 = LINE ( 'NONE', #11819, #17852 ) ;
#23909 = CARTESIAN_POINT ( 'NONE',  ( -170.0000000000000284, -93.50000000000001421, -51.54700538379269403 ) ) ;
#23910 = VECTOR ( 'NONE', #17214, 1000.000000000000000 ) ;
#23911 = VERTEX_POINT ( 'NONE', #38015 ) ;
#23912 = EDGE_CURVE ( 'NONE', #20769, #11672, #32617, .T. ) ;
#23913 = AXIS2_PLACEMENT_3D ( 'NONE', #8742, #24783, #17161 ) ;
#23914 = CARTESIAN_POINT ( 'NONE',  ( 3.555982085019433914, 56.50744240459307832, -17.15800186250228876 ) ) ;
#23915 = EDGE_CURVE ( 'NONE', #42173, #18306, #34083, .T. ) ;
#23916 = ORIENTED_EDGE ( 'NONE', *, *, #48458, .F. ) ;
#23917 = AXIS2_PLACEMENT_3D ( 'NONE', #11256, #47803, #3908 ) ;
#23918 = ORIENTED_EDGE ( 'NONE', *, *, #41487, .F. ) ;
#23919 = EDGE_LOOP ( 'NONE', ( #11573, #24301, #20172, #1369 ) ) ;
#23920 = FACE_OUTER_BOUND ( 'NONE', #39689, .T. ) ;
#23921 = EDGE_CURVE ( 'NONE', #6882, #12420, #4947, .T. ) ;
#23922 = ORIENTED_EDGE ( 'NONE', *, *, #18309, .T. ) ;
#23923 = ADVANCED_FACE ( 'NONE', ( #18572 ), #3054, .T. ) ;
#23924 = EDGE_CURVE ( 'NONE', #39444, #1712, #34346, .T. ) ;
#23925 = CARTESIAN_POINT ( 'NONE',  ( 58.12687231399075927, -193.5000000000000000, -63.33473559879914916 ) ) ;
#23926 = LINE ( 'NONE', #42871, #51247 ) ;
#23929 = ORIENTED_EDGE ( 'NONE', *, *, #48870, .T. ) ;
#23928 = DIRECTION ( 'NONE',  ( -0.000000000000000000, 0.000000000000000000, 1.000000000000000000 ) ) ;
#23927 = DIRECTION ( 'NONE',  ( -1.000000000000000000, 0.000000000000000000, 0.000000000000000000 ) ) ;
#23930 = ADVANCED_FACE ( 'NONE', ( #26964 ), #35113, .T. ) ;
#23931 = AXIS2_PLACEMENT_3D ( 'NONE', #13440, #8708, #37081 ) ;
#23932 = EDGE_CURVE ( 'NONE', #31839, #34695, #43000, .T. ) ;
#23933 = CARTESIAN_POINT ( 'NONE',  ( -150.5215542367829471, -193.5000000000000000, -72.19655804061974891 ) ) ;
#23934 = AXIS2_PLACEMENT_3D ( 'NONE', #52024, #8113, #8375 ) ;
#23935 = ORIENTED_EDGE ( 'NONE', *, *, #14484, .F. ) ;
#23936 = CARTESIAN_POINT ( 'NONE',  ( -38.78589637709156790, -177.1207230881787780, -123.6213615703898654 ) ) ;
#23937 = ORIENTED_EDGE ( 'NONE', *, *, #32344, .T. ) ;
#23938 = VECTOR ( 'NONE', #25973, 1000.000000000000000 ) ;
#23939 = CARTESIAN_POINT ( 'NONE',  ( -91.81555821786918159, -189.7472609257535510, 116.1806952091180563 ) ) ;
#23940 = DIRECTION ( 'NONE',  ( 0.000000000000000000, -0.4647231720437724478, -0.8854560256532078011 ) ) ;
#23942 = DIRECTION ( 'NONE',  ( -0.9646355819083576311, 0.000000000000000000, -0.2635871660690715101 ) ) ;
#23941 = DIRECTION ( 'NONE',  ( 1.000000000000000000, 0.000000000000000000, -0.000000000000000000 ) ) ;
#23943 = VECTOR ( 'NONE', #180, 1000.000000000000000 ) ;
#23944 = VERTEX_POINT ( 'NONE', #50386 ) ;
#23945 = CARTESIAN_POINT ( 'NONE',  ( -138.3705904895685990, -177.1207230881787780, -86.85922373029299592 ) ) ;
#23946 = PLANE ( 'NONE',  #28692 ) ;
#23947 = SHAPE_REPRESENTATION_RELATIONSHIP ( 'NONE' , 'NONE' ,  #33116, #7414 ) ;
#23948 = ORIENTED_EDGE ( 'NONE', *, *, #16880, .F. ) ;
#23949 = CARTESIAN_POINT ( 'NONE',  ( -47.51449116960048968, -177.1207230881787780, -0.2635871660690578544 ) ) ;
#23950 = CARTESIAN_POINT ( 'NONE',  ( -109.9568094315246327, -183.6283474603465606, -108.8370090194290611 ) ) ;
#23951 = VECTOR ( 'NONE', #13562, 1000.000000000000114 ) ;
#23952 = LINE ( 'NONE', #39705, #27387 ) ;
#23953 = ORIENTED_EDGE ( 'NONE', *, *, #25077, .F. ) ;
#23954 = PLANE ( 'NONE',  #37675 ) ;
#23955 = AXIS2_PLACEMENT_3D ( 'NONE', #37322, #49165, #8688 ) ;
#23956 = CARTESIAN_POINT ( 'NONE',  ( -336.3521761649654422, -82.40546666720629787, 42.41660376256258047 ) ) ;
#23957 = VECTOR ( 'NONE', #47412, 1000.000000000000000 ) ;
#23958 = ORIENTED_EDGE ( 'NONE', *, *, #38240, .F. ) ;
#23959 = CARTESIAN_POINT ( 'NONE',  ( -48.47912675150885065, -175.3837268820161057, 6.938893903907228378E-15 ) ) ;
#23960 = ORIENTED_EDGE ( 'NONE', *, *, #20183, .T. ) ;
#23961 = CARTESIAN_POINT ( 'NONE',  ( -166.6265240196292439, -175.3837268820161057, 40.81902153125349741 ) ) ;
#23962 = LINE ( 'NONE', #27385, #51312 ) ;
#23963 = CARTESIAN_POINT ( 'NONE',  ( -48.47912675150885065, -175.3837268820161057, 6.938893903907228378E-15 ) ) ;
#23964 = CARTESIAN_POINT ( 'NONE',  ( -121.8391548840036762, -193.5000000000000000, -99.97252634603249533 ) ) ;
#23965 = LINE ( 'NONE', #40766, #2270 ) ;
#23966 = DIRECTION ( 'NONE',  ( 0.3482016354343995812, 0.000000000000000000, -0.9374196611341205632 ) ) ;
#23967 = AXIS2_PLACEMENT_3D ( 'NONE', #51009, #15005, #39152 ) ;
#23968 = DIRECTION ( 'NONE',  ( -0.9785564922995017012, 0.000000000000000000, -0.2059786187411094538 ) ) ;
#23969 = DIRECTION ( 'NONE',  ( 0.9051968626821054187, -0.4249925173346862373, 0.000000000000000000 ) ) ;
#23971 = ORIENTED_EDGE ( 'NONE', *, *, #18374, .F. ) ;
#23970 = FACE_OUTER_BOUND ( 'NONE', #2920, .T. ) ;
#23972 = VECTOR ( 'NONE', #38680, 1000.000000000000000 ) ;
#23973 = VECTOR ( 'NONE', #26621, 1000.000000000000000 ) ;
#23974 = EDGE_CURVE ( 'NONE', #36669, #9672, #26714, .T. ) ;
#23975 = ORIENTED_EDGE ( 'NONE', *, *, #21815, .F. ) ;
#23976 = EDGE_CURVE ( 'NONE', #21496, #28486, #10792, .T. ) ;
#23977 = EDGE_CURVE ( 'NONE', #36397, #17068, #46964, .T. ) ;
#23978 = DIRECTION ( 'NONE',  ( 0.000000000000000000, -1.000000000000000000, 0.000000000000000000 ) ) ;
#23979 = CARTESIAN_POINT ( 'NONE',  ( -48.47912675150885065, -189.7472609257535510, 6.938893903907228378E-15 ) ) ;
#23980 = ORIENTED_EDGE ( 'NONE', *, *, #30472, .F. ) ;
#23981 = ORIENTED_EDGE ( 'NONE', *, *, #9296, .T. ) ;
#23982 = VECTOR ( 'NONE', #41013, 1000.000000000000114 ) ;
#23983 = EDGE_LOOP ( 'NONE', ( #34476, #25931, #47724, #42773 ) ) ;
#23984 = DIRECTION ( 'NONE',  ( 0.000000000000000000, 0.000000000000000000, -1.000000000000000000 ) ) ;
#23985 = CARTESIAN_POINT ( 'NONE',  ( -167.1580984288390823, -175.3837268820161057, -39.24667733211878584 ) ) ;
#23986 = EDGE_CURVE ( 'NONE', #49319, #15063, #34841, .T. ) ;
#23987 = CIRCLE ( 'NONE', #30700, 4.000000000000003553 ) ;
#23988 = EDGE_CURVE ( 'NONE', #2175, #5608, #35365, .T. ) ;
#23990 = CIRCLE ( 'NONE', #1344, 60.00000000000000000 ) ;
#23989 = DIRECTION ( 'NONE',  ( -0.000000000000000000, 1.000000000000000000, -0.000000000000000000 ) ) ;
#23991 = DIRECTION ( 'NONE',  ( -0.000000000000000000, -0.4647231720437724478, -0.8854560256532078011 ) ) ;
#23992 = ORIENTED_EDGE ( 'NONE', *, *, #14535, .F. ) ;
#23993 = ORIENTED_EDGE ( 'NONE', *, *, #4710, .T. ) ;
#23994 = EDGE_CURVE ( 'NONE', #20319, #12264, #23306, .T. ) ;
#23995 = EDGE_LOOP ( 'NONE', ( #10005, #30559, #14042, #7627 ) ) ;
#23996 = CIRCLE ( 'NONE', #50877, 4.999999999999997335 ) ;
#23997 = DIRECTION ( 'NONE',  ( 0.000000000000000000, -0.9709418174260544543, -0.2393156642875482465 ) ) ;
#23998 = CARTESIAN_POINT ( 'NONE',  ( 76.09804998693969935, -193.5000000000000000, 10.27263529369908746 ) ) ;
#23999 = DIRECTION ( 'NONE',  ( -0.000000000000000000, 1.000000000000000000, -0.000000000000000000 ) ) ;
#24000 = EDGE_CURVE ( 'NONE', #3155, #50821, #39330, .T. ) ;
#24001 = DIRECTION ( 'NONE',  ( 0.000000000000000000, 0.6631226582407911962, -0.7485107481711046340 ) ) ;
#24002 = CARTESIAN_POINT ( 'NONE',  ( -339.1964088526558498, -115.8919814278862503, 58.50955523165745831 ) ) ;
#24003 = ORIENTED_EDGE ( 'NONE', *, *, #22979, .F. ) ;
#24004 = CARTESIAN_POINT ( 'NONE',  ( -332.3517673607765914, -140.1754235130667610, -56.65561927338005432 ) ) ;
#24005 = EDGE_CURVE ( 'NONE', #1407, #2868, #23028, .T. ) ;
#24006 = CARTESIAN_POINT ( 'NONE',  ( -5.113431607746569796, -189.7472609257535510, 117.2365833888819537 ) ) ;
#24007 = CARTESIAN_POINT ( 'NONE',  ( 49.88781503343063406, -183.6283474603465606, -75.49882471933871386 ) ) ;
#24008 = CARTESIAN_POINT ( 'NONE',  ( 57.12946453413545100, -189.7472609257535510, 66.87170886601998632 ) ) ;
#24009 = ORIENTED_EDGE ( 'NONE', *, *, #5037, .T. ) ;
#24010 = ORIENTED_EDGE ( 'NONE', *, *, #788, .T. ) ;
#24011 = AXIS2_PLACEMENT_3D ( 'NONE', #7808, #16222, #15454 ) ;
#24012 = ORIENTED_EDGE ( 'NONE', *, *, #37476, .F. ) ;
#24013 = DIRECTION ( 'NONE',  ( -0.8455960035018311727, 0.000000000000000000, 0.5338233779647826305 ) ) ;
#24014 = VECTOR ( 'NONE', #31278, 1000.000000000000227 ) ;
#24015 = DIRECTION ( 'NONE',  ( 0.000000000000000000, -0.1205366802553199113, 0.9927088740980544168 ) ) ;
#24016 = ORIENTED_EDGE ( 'NONE', *, *, #19872, .F. ) ;
#24017 = CARTESIAN_POINT ( 'NONE',  ( 33.09766481721658238, -175.3837268820161057, 93.38753978496653474 ) ) ;
#24018 = CIRCLE ( 'NONE', #12229, 60.00000000000000000 ) ;
#24019 = AXIS2_PLACEMENT_3D ( 'NONE', #28663, #40490, #36045 ) ;
#24020 = CARTESIAN_POINT ( 'NONE',  ( -55.05561436132770581, -193.5000000000000000, 124.8268793598474105 ) ) ;
#24021 = DIRECTION ( 'NONE',  ( 1.000000000000000000, -0.000000000000000000, -0.000000000000000000 ) ) ;
#24022 = ORIENTED_EDGE ( 'NONE', *, *, #47554, .F. ) ;
#24023 = CARTESIAN_POINT ( 'NONE',  ( -336.3521761649654422, -65.24746378767824240, -9.724760635741734660 ) ) ;
#24024 = EDGE_CURVE ( 'NONE', #775, #10747, #14371, .T. ) ;
#24025 = EDGE_LOOP ( 'NONE', ( #52019, #42608, #39810, #33640 ) ) ;
#24026 = FACE_OUTER_BOUND ( 'NONE', #17357, .T. ) ;
#24027 = VERTEX_POINT ( 'NONE', #22247 ) ;
#24028 = CARTESIAN_POINT ( 'NONE',  ( -75.48985759771373694, -183.6283474603465606, -122.0467960216648606 ) ) ;
#24029 = VECTOR ( 'NONE', #41083, 1000.000000000000114 ) ;
#24030 = COLOUR_RGB ( '', 0.66274510, 0.83137255, 0.94901961) ;
#24031 = DIRECTION ( 'NONE',  ( 0.000000000000000000, 0.000000000000000000, 1.000000000000000000 ) ) ;
#24032 = ORIENTED_EDGE ( 'NONE', *, *, #29380, .T. ) ;
#24033 = AXIS2_PLACEMENT_3D ( 'NONE', #49647, #13635, #6011 ) ;
#24034 = VECTOR ( 'NONE', #49521, 1000.000000000000227 ) ;
#24035 = DIRECTION ( 'NONE',  ( 0.000000000000000000, 0.000000000000000000, 1.000000000000000000 ) ) ;
#24036 = CARTESIAN_POINT ( 'NONE',  ( -48.65601702663143868, -193.5000000000000000, 0.9842305779476024918 ) ) ;
#24037 = LINE ( 'NONE', #40050, #5578 ) ;
#24038 = VECTOR ( 'NONE', #10415, 1000.000000000000000 ) ;
#24039 = DIRECTION ( 'NONE',  ( 1.000000000000000000, -0.000000000000000000, -0.000000000000000000 ) ) ;
#24040 = ORIENTED_EDGE ( 'NONE', *, *, #1576, .T. ) ;
#24042 = VECTOR ( 'NONE', #25063, 1000.000000000000000 ) ;
#24041 = PLANE ( 'NONE',  #37038 ) ;
#24043 = ORIENTED_EDGE ( 'NONE', *, *, #33662, .F. ) ;
#24044 = EDGE_CURVE ( 'NONE', #13064, #2622, #26443, .T. ) ;
#24045 = ORIENTED_EDGE ( 'NONE', *, *, #12598, .F. ) ;
#24046 = LINE ( 'NONE', #19838, #42793 ) ;
#24048 = EDGE_LOOP ( 'NONE', ( #1644, #14545, #43794, #37294 ) ) ;
#24047 = DIRECTION ( 'NONE',  ( 0.000000000000000000, 0.000000000000000000, 1.000000000000000000 ) ) ;
#24049 = ADVANCED_FACE ( 'NONE', ( #38545 ), #31170, .F. ) ;
#24050 = EDGE_CURVE ( 'NONE', #11314, #34044, #50267, .T. ) ;
#24051 = ORIENTED_EDGE ( 'NONE', *, *, #7054, .F. ) ;
#24052 = ADVANCED_FACE ( 'NONE', ( #3320 ), #19354, .T. ) ;
#24053 = DIRECTION ( 'NONE',  ( -0.000000000000000000, 0.000000000000000000, -1.000000000000000000 ) ) ;
#24054 = EDGE_CURVE ( 'NONE', #42459, #35361, #14635, .T. ) ;
#24055 = EDGE_CURVE ( 'NONE', #49368, #19699, #640, .T. ) ;
#24056 = CARTESIAN_POINT ( 'NONE',  ( -336.3521761649654422, -159.1821513111375452, -47.06073758877369073 ) ) ;
#24057 = AXIS2_PLACEMENT_3D ( 'NONE', #3026, #43499, #16160 ) ;
#24058 = AXIS2_PLACEMENT_3D ( 'NONE', #25090, #27971, #12709 ) ;
#24059 = ORIENTED_EDGE ( 'NONE', *, *, #39204, .T. ) ;
#24060 = CARTESIAN_POINT ( 'NONE',  ( -38.78589637709156790, -183.6283474603465606, -123.6213615703898654 ) ) ;
#24061 = EDGE_CURVE ( 'NONE', #28636, #48811, #40299, .T. ) ;
#24062 = CARTESIAN_POINT ( 'NONE',  ( 11.66870402553031560, -183.6283474603465606, 108.4360005853211391 ) ) ;
#24063 = EDGE_LOOP ( 'NONE', ( #43592, #48621, #6279, #21301 ) ) ;
#24064 = CARTESIAN_POINT ( 'NONE',  ( 67.42090074966655777, -175.3837268820161057, -46.82076062204441769 ) ) ;
#24065 = DIRECTION ( 'NONE',  ( 1.000000000000000000, -0.000000000000000000, -0.000000000000000000 ) ) ;
#24066 = CIRCLE ( 'NONE', #48369, 125.0000000000000000 ) ;
#24067 = ADVANCED_FACE ( 'NONE', ( #886, #20877, #44269, #40821, #16928, #48990, #28988, #4315, #45056, #32169, #4067, #106, #20335, #8255, #36368, #361, #16414, #32427, #48484, #47428, #43738, #51629, #23770, #3793, #15902, #10989, #8087, #7821, #15467, #2847, #18871, #15737, #27536, #19916, #31473, #44082, #19396, #30967, #47272, #39364, #51467, #47524, #3109, #31216, #11243, #19150, #7061, #31990, #38845, #15206, #43309, #23592, #51727, #7574, #34893, #35675, #35164, #47011, #27271, #50962, #51997, #23084, #14959, #23850, #11507, #27013, #43054, #39094, #3619, #51218, #7319, #23353, #3367, #35414, #43819, #48033, #43573, #39605, #31746, #19648, #35950, #47783, #39861, #3890, #11759, #27786, #15981, #12013, #28041, #49343, #13333, #20690, #44608, #444, #40141, #36447, #4398, #24897, #20424, #24625, #48293, #45150, #726, #4158, #20168, #17024 ), #36188, .T. ) ;
#24068 = DIRECTION ( 'NONE',  ( 0.000000000000000000, 1.850371707708594366E-15, 1.000000000000000000 ) ) ;
#24069 = DIRECTION ( 'NONE',  ( 0.000000000000000000, 1.000000000000000000, -0.000000000000000000 ) ) ;
#24070 = ORIENTED_EDGE ( 'NONE', *, *, #25077, .T. ) ;
#24071 = ORIENTED_EDGE ( 'NONE', *, *, #16342, .T. ) ;
#24072 = EDGE_CURVE ( 'NONE', #29379, #26067, #33032, .T. ) ;
#24073 = VERTEX_POINT ( 'NONE', #32248 ) ;
#24074 = LINE ( 'NONE', #35625, #3928 ) ;
#24075 = PLANE ( 'NONE',  #6718 ) ;
#24076 = VECTOR ( 'NONE', #31576, 1000.000000000000000 ) ;
#24077 = EDGE_CURVE ( 'NONE', #42568, #49872, #41889, .T. ) ;
#24078 = VECTOR ( 'NONE', #3660, 1000.000000000000000 ) ;
#24079 = LINE ( 'NONE', #3842, #5852 ) ;
#24080 = SHAPE_REPRESENTATION ( 'Flanges', ( #31742 ), #49435 ) ;
#24081 = AXIS2_PLACEMENT_3D ( 'NONE', #51298, #27099, #22916 ) ;
#24083 = AXIS2_PLACEMENT_3D ( 'NONE', #42384, #22162, #45820 ) ;
#24082 = FACE_BOUND ( 'NONE', #32179, .T. ) ;
#24084 = DIRECTION ( 'NONE',  ( 0.5586467658036594619, 0.000000000000000000, -0.8294056854501971054 ) ) ;
#24085 = VERTEX_POINT ( 'NONE', #16498 ) ;
#24086 = EDGE_CURVE ( 'NONE', #41453, #1515, #4938, .T. ) ;
#24087 = VECTOR ( 'NONE', #28255, 1000.000000000000114 ) ;
#24088 = EDGE_CURVE ( 'NONE', #22824, #16966, #24133, .T. ) ;
#24089 = AXIS2_PLACEMENT_3D ( 'NONE', #28595, #47557, #11542 ) ;
#24090 = CARTESIAN_POINT ( 'NONE',  ( 25.00456841203573077, 65.00000000000000000, 3.062176466986057355E-15 ) ) ;
#24091 = VERTEX_POINT ( 'NONE', #1226 ) ;
#24093 = EDGE_LOOP ( 'NONE', ( #12438, #1136, #34383, #10362 ) ) ;
#24092 = CARTESIAN_POINT ( 'NONE',  ( 72.05536924052414349, -175.3837268820161057, 33.11246405730899056 ) ) ;
#24094 = EDGE_LOOP ( 'NONE', ( #2425, #25932, #27736, #38020 ) ) ;
#24095 = PLANE ( 'NONE',  #3118 ) ;
#24096 = FACE_OUTER_BOUND ( 'NONE', #15103, .T. ) ;
#24097 = CARTESIAN_POINT ( 'NONE',  ( -305.0000000000000568, -123.5000000000000284, 20.00000000000001066 ) ) ;
#24098 = DIRECTION ( 'NONE',  ( 0.9266896074318370369, 0.000000000000000000, -0.3758275821142292306 ) ) ;
#24099 = ORIENTED_EDGE ( 'NONE', *, *, #1027, .T. ) ;
#24100 = DIRECTION ( 'NONE',  ( 1.000000000000000000, 0.000000000000000000, 0.000000000000000000 ) ) ;
#24101 = ORIENTED_EDGE ( 'NONE', *, *, #35262, .F. ) ;
#24102 = EDGE_CURVE ( 'NONE', #19363, #48057, #16734, .T. ) ;
#24103 = EDGE_CURVE ( 'NONE', #34369, #19650, #44364, .T. ) ;
#24104 = ORIENTED_EDGE ( 'NONE', *, *, #1230, .F. ) ;
#24105 = CARTESIAN_POINT ( 'NONE',  ( -60.00000000000000000, -43.50000000000000000, -0.000000000000000000 ) ) ;
#24106 = AXIS2_PLACEMENT_3D ( 'NONE', #34857, #3070, #39332 ) ;
#24107 = AXIS2_PLACEMENT_3D ( 'NONE', #35731, #31529, #12064 ) ;
#24108 = CARTESIAN_POINT ( 'NONE',  ( -49.46816693883101834, -193.5000000000000000, 0.1476465640024780257 ) ) ;
#24109 = DIRECTION ( 'NONE',  ( 0.000000000000000000, 1.000000000000000000, -0.000000000000000000 ) ) ;
#24110 = PLANE ( 'NONE',  #8821 ) ;
#24111 = VECTOR ( 'NONE', #12662, 1000.000000000000000 ) ;
#24112 = DIRECTION ( 'NONE',  ( 0.000000000000000000, 0.000000000000000000, -1.000000000000000000 ) ) ;
#24113 = CARTESIAN_POINT ( 'NONE',  ( -172.0839188101924719, -189.7472609257535510, -18.62405380494754681 ) ) ;
#24114 = ORIENTED_EDGE ( 'NONE', *, *, #32332, .F. ) ;
#24115 = DIRECTION ( 'NONE',  ( 1.000000000000000000, 0.000000000000000000, 0.000000000000000000 ) ) ;
#24116 = DIRECTION ( 'NONE',  ( 0.000000000000000000, 0.000000000000000000, 1.000000000000000000 ) ) ;
#24117 = FACE_BOUND ( 'NONE', #32547, .T. ) ;
#24118 = ORIENTED_EDGE ( 'NONE', *, *, #9529, .F. ) ;
#24119 = CIRCLE ( 'NONE', #13195, 125.0000000000000000 ) ;
#24120 = VECTOR ( 'NONE', #16903, 1000.000000000000000 ) ;
#24121 = DIRECTION ( 'NONE',  ( 0.000000000000000000, -1.000000000000000000, -0.000000000000000000 ) ) ;
#24122 = AXIS2_PLACEMENT_3D ( 'NONE', #14649, #2812, #34859 ) ;
#24123 = DIRECTION ( 'NONE',  ( 0.000000000000000000, -1.000000000000000000, 0.000000000000000000 ) ) ;
#24124 = EDGE_CURVE ( 'NONE', #48059, #49114, #29081, .T. ) ;
#24125 = EDGE_LOOP ( 'NONE', ( #21391, #37501, #45279, #25809 ) ) ;
#24126 = ADVANCED_FACE ( 'NONE', ( #32520 ), #48569, .T. ) ;
#24127 = CARTESIAN_POINT ( 'NONE',  ( 75.67769207106684348, -177.1207230881787780, 14.49428645563876650 ) ) ;
#24128 = VECTOR ( 'NONE', #7955, 1000.000000000000000 ) ;
#24129 = VERTEX_POINT ( 'NONE', #37239 ) ;
#24130 = AXIS2_PLACEMENT_3D ( 'NONE', #6878, #18710, #34724 ) ;
#24131 = ADVANCED_FACE ( 'NONE', ( #36979 ), #29346, .F. ) ;
#24132 = DIRECTION ( 'NONE',  ( 0.000000000000000000, 0.000000000000000000, 1.000000000000000000 ) ) ;
#24133 = LINE ( 'NONE', #41174, #4990 ) ;
#24134 = DIRECTION ( 'NONE',  ( -0.000000000000000000, -0.6631226582407989678, -0.7485107481710977506 ) ) ;
#24135 = CARTESIAN_POINT ( 'NONE',  ( -305.0000000000000568, -64.15626348514393840, -8.849911663702499709 ) ) ;
#24136 = VERTEX_POINT ( 'NONE', #16771 ) ;
#24137 = ORIENTED_EDGE ( 'NONE', *, *, #39398, .T. ) ;
#24138 = DIRECTION ( 'NONE',  ( 0.000000000000000000, 1.000000000000000000, 0.000000000000000000 ) ) ;
#24139 = AXIS2_PLACEMENT_3D ( 'NONE', #19311, #35324, #50338 ) ;
#24140 = CIRCLE ( 'NONE', #1478, 125.0000000000000000 ) ;
#24141 = ORIENTED_EDGE ( 'NONE', *, *, #22747, .T. ) ;
#24142 = EDGE_CURVE ( 'NONE', #29051, #38775, #10822, .T. ) ;
#24143 = DIRECTION ( 'NONE',  ( -1.000000000000000000, 0.000000000000000000, 0.000000000000000000 ) ) ;
#24144 = CARTESIAN_POINT ( 'NONE',  ( 14.37129481273060172, -175.3837268820161057, -108.0501018472328099 ) ) ;
#24145 = AXIS2_PLACEMENT_3D ( 'NONE', #49661, #12868, #32839 ) ;
#24146 = EDGE_CURVE ( 'NONE', #35564, #21924, #28817, .T. ) ;
#24147 = CARTESIAN_POINT ( 'NONE',  ( -110.8210171970983566, -189.7472609257535510, 107.1890582354659074 ) ) ;
#24148 = ORIENTED_EDGE ( 'NONE', *, *, #14324, .T. ) ;
#24151 = ORIENTED_EDGE ( 'NONE', *, *, #38996, .T. ) ;
#24150 = FACE_OUTER_BOUND ( 'NONE', #27125, .T. ) ;
#24149 = DIRECTION ( 'NONE',  ( 0.000000000000000000, 1.000000000000000000, 0.000000000000000000 ) ) ;
#24152 = AXIS2_PLACEMENT_3D ( 'NONE', #26118, #14570, #42147 ) ;
#24153 = ORIENTED_EDGE ( 'NONE', *, *, #49529, .F. ) ;
#24154 = VECTOR ( 'NONE', #1834, 1000.000000000000000 ) ;
#24155 = VECTOR ( 'NONE', #13752, 1000.000000000000000 ) ;
#24156 = PLANE ( 'NONE',  #43279 ) ;
#24157 = ORIENTED_EDGE ( 'NONE', *, *, #11333, .T. ) ;
#24158 = CARTESIAN_POINT ( 'NONE',  ( 66.49421114223471818, -193.5000000000000000, -46.44493303993018429 ) ) ;
#24159 = ORIENTED_EDGE ( 'NONE', *, *, #20947, .F. ) ;
#24160 = LINE ( 'NONE', #32274, #39303 ) ;
#24161 = EDGE_LOOP ( 'NONE', ( #5745, #22757, #42888, #38340 ) ) ;
#24163 = CARTESIAN_POINT ( 'NONE',  ( -47.78257572244586271, -183.6283474603465606, 0.7175072570443418174 ) ) ;
#24162 = CARTESIAN_POINT ( 'NONE',  ( -339.1964088526558498, -96.52406086224361559, 52.47426709956096147 ) ) ;
#24164 = ORIENTED_EDGE ( 'NONE', *, *, #26739, .T. ) ;
#24165 = VECTOR ( 'NONE', #51233, 1000.000000000000000 ) ;
#24166 = EDGE_LOOP ( 'NONE', ( #11833, #2487, #9986, #40100 ) ) ;
#24167 = DIRECTION ( 'NONE',  ( -0.000000000000000000, 1.000000000000000000, -0.000000000000000000 ) ) ;
#24168 = DIRECTION ( 'NONE',  ( 0.6300878435817148793, 0.000000000000000000, -0.7765238627180394149 ) ) ;
#24169 = LINE ( 'NONE', #40178, #12074 ) ;
#24170 = CARTESIAN_POINT ( 'NONE',  ( 31.84037011350117297, -175.3837268820161057, -94.47107458416900272 ) ) ;
#24171 = DIRECTION ( 'NONE',  ( -0.000000000000000000, 0.9709418174260527890, 0.2393156642875547968 ) ) ;
#24172 = DIRECTION ( 'NONE',  ( -0.4031234292879665171, 0.000000000000000000, -0.9151456172430210145 ) ) ;
#24173 = ORIENTED_EDGE ( 'NONE', *, *, #24184, .F. ) ;
#24174 = PLANE ( 'NONE',  #25488 ) ;
#24175 = CARTESIAN_POINT ( 'NONE',  ( -108.4791267515088435, -173.5000000000000284, 60.00000000000002132 ) ) ;
#24176 = CARTESIAN_POINT ( 'NONE',  ( -134.9734323446613473, -189.7472609257535510, 88.85232316304889366 ) ) ;
#24177 = ORIENTED_EDGE ( 'NONE', *, *, #45830, .T. ) ;
#24178 = VECTOR ( 'NONE', #17766, 1000.000000000000000 ) ;
#24179 = DIRECTION ( 'NONE',  ( -0.000000000000000000, 0.5680647467311540355, -0.8229838658936575735 ) ) ;
#24180 = VECTOR ( 'NONE', #9334, 1000.000000000000000 ) ;
#24181 = DIRECTION ( 'NONE',  ( 0.000000000000000000, 5.319818659662208160E-15, -1.000000000000000000 ) ) ;
#24182 = PLANE ( 'NONE',  #17408 ) ;
#24183 = ORIENTED_EDGE ( 'NONE', *, *, #32435, .F. ) ;
#24184 = EDGE_CURVE ( 'NONE', #49764, #23726, #30375, .T. ) ;
#24185 = ORIENTED_EDGE ( 'NONE', *, *, #39151, .F. ) ;
#24186 = VERTEX_POINT ( 'NONE', #17546 ) ;
#24187 = AXIS2_PLACEMENT_3D ( 'NONE', #11513, #30452, #22836 ) ;
#24188 = DIRECTION ( 'NONE',  ( 0.000000000000000000, -1.000000000000000000, 0.000000000000000000 ) ) ;
#24189 = CARTESIAN_POINT ( 'NONE',  ( -69.77312546433407192, -175.3837268820161057, 123.1729094355500109 ) ) ;
#24190 = LINE ( 'NONE', #23414, #44708 ) ;
#24191 = PLANE ( 'NONE',  #42152 ) ;
#24192 = EDGE_LOOP ( 'NONE', ( #42089, #19473 ) ) ;
#24193 = CARTESIAN_POINT ( 'NONE',  ( -330.4913330509368166, -63.50208336950359467, 0.4999999999999551470 ) ) ;
#24194 = EDGE_LOOP ( 'NONE', ( #48591, #27497, #3189, #41816 ) ) ;
#24195 = CIRCLE ( 'NONE', #6611, 60.00000000000000000 ) ;
#24196 = VERTEX_POINT ( 'NONE', #37752 ) ;
#24197 = ORIENTED_EDGE ( 'NONE', *, *, #9939, .T. ) ;
#24198 = EDGE_CURVE ( 'NONE', #32264, #49114, #33561, .T. ) ;
#24199 = DIRECTION ( 'NONE',  ( -0.5586467658036535777, 0.000000000000000000, 0.8294056854502011022 ) ) ;
#24200 = ORIENTED_EDGE ( 'NONE', *, *, #29496, .T. ) ;
#24201 = LINE ( 'NONE', #16309, #31745 ) ;
#24202 = CARTESIAN_POINT ( 'NONE',  ( -90.87721961371605062, -193.5000000000000000, 116.5264228893328635 ) ) ;
#24205 = ORIENTED_EDGE ( 'NONE', *, *, #35436, .T. ) ;
#24204 = CARTESIAN_POINT ( 'NONE',  ( 0.000000000000000000, -116.3883358649353141, 58.56982357178514320 ) ) ;
#24203 = CARTESIAN_POINT ( 'NONE',  ( -142.3192003680973130, -193.5000000000000000, 82.57748230379306165 ) ) ;
#24206 = AXIS2_PLACEMENT_3D ( 'NONE', #9814, #20870, #45315 ) ;
#24207 = VECTOR ( 'NONE', #23664, 1000.000000000000000 ) ;
#24208 = EDGE_CURVE ( 'NONE', #23027, #51264, #1497, .T. ) ;
#24209 = PLANE ( 'NONE',  #40715 ) ;
#24210 = ORIENTED_EDGE ( 'NONE', *, *, #37557, .T. ) ;
#24211 = CARTESIAN_POINT ( 'NONE',  ( -117.6201219941651601, -175.3837268820161057, 104.1370384486469902 ) ) ;
#24212 = AXIS2_PLACEMENT_3D ( 'NONE', #5275, #28897, #797 ) ;
#24213 = ORIENTED_EDGE ( 'NONE', *, *, #4147, .T. ) ;
#24214 = DIRECTION ( 'NONE',  ( -0.000000000000000000, 1.000000000000000000, -0.000000000000000000 ) ) ;
#24215 = EDGE_CURVE ( 'NONE', #39946, #43466, #41050, .T. ) ;
#24216 = DIRECTION ( 'NONE',  ( 0.000000000000000000, -0.7485107481711069655, -0.6631226582407885317 ) ) ;
#24218 = DIRECTION ( 'NONE',  ( 0.000000000000000000, 0.000000000000000000, 1.000000000000000000 ) ) ;
#24217 = DIRECTION ( 'NONE',  ( 0.000000000000000000, 0.8660254037844379305, 0.5000000000000011102 ) ) ;
#24219 = VECTOR ( 'NONE', #28825, 1000.000000000000000 ) ;
#24220 = DIRECTION ( 'NONE',  ( -0.000000000000000000, 1.000000000000000000, -0.000000000000000000 ) ) ;
#24221 = CARTESIAN_POINT ( 'NONE',  ( -330.4913330509368166, -79.66942718702547666, -39.49849221029252533 ) ) ;
#24222 = ORIENTED_EDGE ( 'NONE', *, *, #28561, .F. ) ;
#24223 = DIRECTION ( 'NONE',  ( -0.000000000000000000, -1.000000000000000000, 0.000000000000000000 ) ) ;
#24224 = FACE_OUTER_BOUND ( 'NONE', #27612, .T. ) ;
#24225 = FACE_OUTER_BOUND ( 'NONE', #35438, .T. ) ;
#24226 = ORIENTED_EDGE ( 'NONE', *, *, #9138, .F. ) ;
#24227 = DIRECTION ( 'NONE',  ( 0.7948544414133481562, 0.000000000000000000, 0.6068001458186002006 ) ) ;
#24228 = CARTESIAN_POINT ( 'NONE',  ( 60.00000000000000000, -113.5000000000000142, -60.00000000000001421 ) ) ;
#24229 = AXIS2_PLACEMENT_3D ( 'NONE', #4127, #40880, #32488 ) ;
#24230 = EDGE_CURVE ( 'NONE', #41086, #45277, #12509, .T. ) ;
#24231 = ORIENTED_EDGE ( 'NONE', *, *, #14748, .T. ) ;
#24232 = CARTESIAN_POINT ( 'NONE',  ( 1.663811650136604481, -193.5000000000000000, -113.4093733337827672 ) ) ;
#24233 = EDGE_LOOP ( 'NONE', ( #20911, #2841, #3500, #3526 ) ) ;
#24234 = DIRECTION ( 'NONE',  ( 0.8757349421956379665, 0.000000000000000000, -0.4827922027307427477 ) ) ;
#24235 = DIRECTION ( 'NONE',  ( 0.000000000000000000, 0.000000000000000000, 1.000000000000000000 ) ) ;
#24236 = FACE_OUTER_BOUND ( 'NONE', #26487, .T. ) ;
#24237 = LINE ( 'NONE', #3476, #24743 ) ;
#24238 = LINE ( 'NONE', #48417, #10629 ) ;
#24239 = EDGE_CURVE ( 'NONE', #7213, #5675, #37493, .T. ) ;
#24240 = EDGE_CURVE ( 'NONE', #29344, #20898, #18046, .T. ) ;
#24241 = DIRECTION ( 'NONE',  ( -1.000000000000000000, -2.497772389992478923E-15, 1.013386094502324929E-14 ) ) ;
#24242 = VECTOR ( 'NONE', #7433, 1000.000000000000000 ) ;
#24243 = EDGE_CURVE ( 'NONE', #24900, #39679, #47781, .T. ) ;
#24244 = VECTOR ( 'NONE', #3378, 1000.000000000000000 ) ;
#24245 = CARTESIAN_POINT ( 'NONE',  ( -339.1964088526558498, -74.40671499923389831, 34.49419324804615172 ) ) ;
#24246 = CARTESIAN_POINT ( 'NONE',  ( -108.4791267515088435, -173.5000000000000284, -60.00000000000002842 ) ) ;
#24248 = ORIENTED_EDGE ( 'NONE', *, *, #17098, .F. ) ;
#24247 = CARTESIAN_POINT ( 'NONE',  ( -339.1964088526558498, -167.9936954712150339, 38.74998146212178796 ) ) ;
#24249 = AXIS2_PLACEMENT_3D ( 'NONE', #26776, #14698, #43065 ) ;
#24250 = ORIENTED_EDGE ( 'NONE', *, *, #6916, .T. ) ;
#24251 = DIRECTION ( 'NONE',  ( -0.000000000000000000, 1.000000000000000000, -0.000000000000000000 ) ) ;
#24252 = FACE_OUTER_BOUND ( 'NONE', #44225, .T. ) ;
#24253 = ORIENTED_EDGE ( 'NONE', *, *, #33844, .T. ) ;
#24254 = VECTOR ( 'NONE', #51934, 1000.000000000000000 ) ;
#24255 = EDGE_LOOP ( 'NONE', ( #6063, #9592, #30554, #46024 ) ) ;
#24256 = ORIENTED_EDGE ( 'NONE', *, *, #46239, .T. ) ;
#24257 = EDGE_CURVE ( 'NONE', #1001, #43120, #25666, .T. ) ;
#24258 = PLANE ( 'NONE',  #20804 ) ;
#24259 = DIRECTION ( 'NONE',  ( -0.000000000000000000, 1.000000000000000000, 0.000000000000000000 ) ) ;
#24260 = FACE_OUTER_BOUND ( 'NONE', #30746, .T. ) ;
#24261 = EDGE_LOOP ( 'NONE', ( #29677, #41820, #43464, #46955 ) ) ;
#24262 = ORIENTED_EDGE ( 'NONE', *, *, #17007, .F. ) ;
#24263 = ORIENTED_EDGE ( 'NONE', *, *, #5314, .T. ) ;
#24264 = VECTOR ( 'NONE', #13299, 1000.000000000000000 ) ;
#24265 = FACE_OUTER_BOUND ( 'NONE', #9634, .T. ) ;
#24266 = LINE ( 'NONE', #15610, #34426 ) ;
#24267 = FACE_OUTER_BOUND ( 'NONE', #42385, .T. ) ;
#24268 = CARTESIAN_POINT ( 'NONE',  ( -336.3521761649654422, -172.9832938399466684, -32.17247266903247294 ) ) ;
#24269 = LINE ( 'NONE', #24002, #21377 ) ;
#24270 = ORIENTED_EDGE ( 'NONE', *, *, #38250, .T. ) ;
#24271 = DIRECTION ( 'NONE',  ( -0.000000000000000000, 1.000000000000000000, -0.000000000000000000 ) ) ;
#24272 = LINE ( 'NONE', #40277, #50125 ) ;
#24273 = DIRECTION ( 'NONE',  ( 0.000000000000000000, -1.000000000000000000, 0.000000000000000000 ) ) ;
#24274 = CARTESIAN_POINT ( 'NONE',  ( -336.3521761649654422, -182.2665742509934148, -5.491276508484069119 ) ) ;
#24275 = EDGE_LOOP ( 'NONE', ( #21237, #18041, #9729, #16657 ) ) ;
#24276 = ORIENTED_EDGE ( 'NONE', *, *, #16334, .F. ) ;
#24277 = ORIENTED_EDGE ( 'NONE', *, *, #45496, .T. ) ;
#24278 = CARTESIAN_POINT ( 'NONE',  ( -68.09401750944518028, -183.6283474603465606, -122.4396006697294581 ) ) ;
#24280 = AXIS2_PLACEMENT_3D ( 'NONE', #51217, #2846, #11241 ) ;
#24279 = PLANE ( 'NONE',  #7377 ) ;
#24281 = ORIENTED_EDGE ( 'NONE', *, *, #13584, .F. ) ;
#24282 = DIRECTION ( 'NONE',  ( 0.000000000000000000, 1.000000000000000000, 0.000000000000000000 ) ) ;
#24283 = CIRCLE ( 'NONE', #39382, 124.9999999999999858 ) ;
#24284 = DIRECTION ( 'NONE',  ( -0.000000000000000000, 1.000000000000000000, -0.000000000000000000 ) ) ;
#24285 = ADVANCED_FACE ( 'NONE', ( #2279 ), #38535, .T. ) ;
#24286 = ADVANCED_FACE ( 'NONE', ( #26172, #10409 ), #49853, .F. ) ;
#24287 = ORIENTED_EDGE ( 'NONE', *, *, #50302, .T. ) ;
#24288 = CARTESIAN_POINT ( 'NONE',  ( -336.3521761649654422, -142.8954717479169574, 55.74477592174805096 ) ) ;
#24289 = CARTESIAN_POINT ( 'NONE',  ( -11.80936624585915418, -189.7472609257535510, -119.5003291395395877 ) ) ;
#24290 = ORIENTED_EDGE ( 'NONE', *, *, #49583, .F. ) ;
#24291 = FACE_OUTER_BOUND ( 'NONE', #4617, .T. ) ;
#24292 = DIRECTION ( 'NONE',  ( -0.8757349421956310831, 0.000000000000000000, -0.4827922027307550712 ) ) ;
#24293 = VERTEX_POINT ( 'NONE', #21987 ) ;
#24294 = CARTESIAN_POINT ( 'NONE',  ( -336.3521761649654422, -114.7679482383557144, 58.37307289257701370 ) ) ;
#24295 = DIRECTION ( 'NONE',  ( -1.000000000000000000, -0.000000000000000000, 0.000000000000000000 ) ) ;
#24296 = CARTESIAN_POINT ( 'NONE',  ( -152.8713435144644563, -183.6283474603465606, -68.75510947788596638 ) ) ;
#24297 = ADVANCED_FACE ( 'NONE', ( #18316 ), #10152, .F. ) ;
#24298 = FACE_OUTER_BOUND ( 'NONE', #18357, .T. ) ;
#24299 = ADVANCED_FACE ( 'NONE', ( #50374 ), #26433, .T. ) ;
#24300 = VECTOR ( 'NONE', #25009, 1000.000000000000000 ) ;
#24301 = ORIENTED_EDGE ( 'NONE', *, *, #31700, .F. ) ;
#24302 = CARTESIAN_POINT ( 'NONE',  ( -23.99795575808071035, -177.1207230881787780, -122.5792489240757703 ) ) ;
#24303 = ORIENTED_EDGE ( 'NONE', *, *, #19516, .T. ) ;
#24304 = ORIENTED_EDGE ( 'NONE', *, *, #14633, .F. ) ;
#24305 = EDGE_CURVE ( 'NONE', #41471, #10047, #36856, .T. ) ;
#24306 = CARTESIAN_POINT ( 'NONE',  ( 59.00260725618642965, -177.1207230881787780, -63.81752780152989857 ) ) ;
#24308 = EDGE_LOOP ( 'NONE', ( #44565, #39654, #32922, #35127 ) ) ;
#24307 = DIRECTION ( 'NONE',  ( 0.000000000000000000, -1.000000000000000000, 0.000000000000000000 ) ) ;
#24309 = ADVANCED_FACE ( 'NONE', ( #18562 ), #21734, .F. ) ;
#24310 = ORIENTED_EDGE ( 'NONE', *, *, #41519, .T. ) ;
#24311 = CARTESIAN_POINT ( 'NONE',  ( -339.1964088526558498, -64.50000000000000000, -0.5000000000000457412 ) ) ;
#24312 = CARTESIAN_POINT ( 'NONE',  ( -48.47912675150883643, -175.3837268820161057, -125.0000000000000000 ) ) ;
#24313 = ORIENTED_EDGE ( 'NONE', *, *, #39934, .T. ) ;
#24314 = AXIS2_PLACEMENT_3D ( 'NONE', #2530, #51407, #10406 ) ;
#24315 = CARTESIAN_POINT ( 'NONE',  ( -48.64924157374594671, -193.5000000000000000, 123.9998842437354227 ) ) ;
#24316 = CARTESIAN_POINT ( 'NONE',  ( -330.4913330509368166, -123.5000000000000284, 0.000000000000000000 ) ) ;
#24317 = ORIENTED_EDGE ( 'NONE', *, *, #47190, .T. ) ;
#24318 = FACE_OUTER_BOUND ( 'NONE', #13479, .T. ) ;
#24319 = CARTESIAN_POINT ( 'NONE',  ( 12.54192669111252734, -177.1207230881787780, 107.9473519284347418 ) ) ;
#24320 = CARTESIAN_POINT ( 'NONE',  ( -173.2419626162308646, -183.6283474603465606, 7.696413904698412800 ) ) ;
#24321 = FACE_OUTER_BOUND ( 'NONE', #10686, .T. ) ;
#24322 = ORIENTED_EDGE ( 'NONE', *, *, #35138, .T. ) ;
#24323 = EDGE_LOOP ( 'NONE', ( #26795, #35922, #10950, #6186 ) ) ;
#24324 = ORIENTED_EDGE ( 'NONE', *, *, #21289, .F. ) ;
#24325 = CARTESIAN_POINT ( 'NONE',  ( -148.7414553014637590, -189.7472609257535510, 72.96212019587208886 ) ) ;
#24326 = CARTESIAN_POINT ( 'NONE',  ( 0.000000000000000000, -150.9186671505826212, -52.24190551353930090 ) ) ;
#24327 = LINE ( 'NONE', #4354, #4982 ) ;
#24328 = FACE_BOUND ( 'NONE', #17180, .T. ) ;
#24329 = DIRECTION ( 'NONE',  ( 0.000000000000000000, 1.000000000000000000, 0.000000000000000000 ) ) ;
#24330 = ORIENTED_EDGE ( 'NONE', *, *, #9582, .T. ) ;
#24331 = AXIS2_PLACEMENT_3D ( 'NONE', #25616, #28766, #41130 ) ;
#24332 = VECTOR ( 'NONE', #25862, 1000.000000000000000 ) ;
#24333 = EDGE_CURVE ( 'NONE', #32376, #39548, #33809, .T. ) ;
#24334 = EDGE_LOOP ( 'NONE', ( #37710, #29119, #25239, #27574 ) ) ;
#24336 = ORIENTED_EDGE ( 'NONE', *, *, #2756, .T. ) ;
#24335 = DIRECTION ( 'NONE',  ( 0.000000000000000000, 0.000000000000000000, 1.000000000000000000 ) ) ;
#24337 = ORIENTED_EDGE ( 'NONE', *, *, #6734, .T. ) ;
#24338 = DIRECTION ( 'NONE',  ( 0.8455960035018272869, 0.000000000000000000, -0.5338233779647886257 ) ) ;
#24339 = FACE_OUTER_BOUND ( 'NONE', #17080, .T. ) ;
#24340 = ADVANCED_FACE ( 'NONE', ( #14622 ), #9390, .T. ) ;
#24341 = CARTESIAN_POINT ( 'NONE',  ( -336.3521761649654422, -170.1129345408508868, -37.77875505479702412 ) ) ;
#24342 = EDGE_CURVE ( 'NONE', #9658, #35836, #15148, .T. ) ;
#24343 = ADVANCED_FACE ( 'NONE', ( #7516, #26954, #2781, #39031, #43760, #31157, #39549, #23534, #38776, #3042 ), #7765, .F. ) ;
#24344 = DIRECTION ( 'NONE',  ( 0.000000000000000000, 1.000000000000000000, 0.000000000000000000 ) ) ;
#24345 = ORIENTED_EDGE ( 'NONE', *, *, #852, .F. ) ;
#24346 = LINE ( 'NONE', #4630, #5729 ) ;
#24347 = EDGE_LOOP ( 'NONE', ( #2788, #46637, #26354, #12640 ) ) ;
#24348 = EDGE_CURVE ( 'NONE', #10662, #23768, #14895, .T. ) ;
#24349 = VERTEX_POINT ( 'NONE', #51665 ) ;
#24350 = DIRECTION ( 'NONE',  ( -0.000000000000000000, 1.000000000000000000, -0.000000000000000000 ) ) ;
#24351 = VECTOR ( 'NONE', #16837, 1000.000000000000000 ) ;
#24352 = EDGE_CURVE ( 'NONE', #31195, #12905, #10932, .T. ) ;
#24353 = CARTESIAN_POINT ( 'NONE',  ( -94.78385179329468713, -193.5000000000000000, 115.0304316645283222 ) ) ;
#24354 = DIRECTION ( 'NONE',  ( -1.000000000000000000, 0.000000000000000000, 0.000000000000000000 ) ) ;
#24355 = PLANE ( 'NONE',  #18875 ) ;
#24356 = DIRECTION ( 'NONE',  ( 0.000000000000000000, -0.000000000000000000, 1.000000000000000000 ) ) ;
#24357 = DIRECTION ( 'NONE',  ( 0.000000000000000000, 1.000000000000000000, 0.000000000000000000 ) ) ;
#24358 = EDGE_CURVE ( 'NONE', #37425, #7460, #15665, .T. ) ;
#24359 = ORIENTED_EDGE ( 'NONE', *, *, #16489, .F. ) ;
#24360 = DIRECTION ( 'NONE',  ( -0.000000000000000000, 1.000000000000000000, -0.000000000000000000 ) ) ;
#24361 = DIRECTION ( 'NONE',  ( 1.000000000000000000, -0.000000000000000000, -0.000000000000000000 ) ) ;
#24362 = EDGE_CURVE ( 'NONE', #40230, #37865, #19589, .T. ) ;
#24363 = CARTESIAN_POINT ( 'NONE',  ( -28.74596282265200387, -183.6283474603465606, 123.4325817657431230 ) ) ;
#24364 = FACE_BOUND ( 'NONE', #44575, .T. ) ;
#24365 = ORIENTED_EDGE ( 'NONE', *, *, #35612, .F. ) ;
#24366 = EDGE_CURVE ( 'NONE', #17543, #36353, #43242, .T. ) ;
#24367 = CARTESIAN_POINT ( 'NONE',  ( -48.88225018079683082, -177.1207230881787780, 0.9151456172430223468 ) ) ;
#24368 = LINE ( 'NONE', #5188, #2608 ) ;
#24369 = ADVANCED_FACE ( 'NONE', ( #47725 ), #15923, .F. ) ;
#24370 = ORIENTED_EDGE ( 'NONE', *, *, #34681, .F. ) ;
#24371 = CARTESIAN_POINT ( 'NONE',  ( -336.3521761649654422, -126.1322888500942270, -59.00000000000001421 ) ) ;
#24372 = ORIENTED_EDGE ( 'NONE', *, *, #9184, .T. ) ;
#24373 = ADVANCED_FACE ( 'NONE', ( #46682 ), #19088, .T. ) ;
#24374 = VECTOR ( 'NONE', #12425, 1000.000000000000000 ) ;
#24375 = AXIS2_PLACEMENT_3D ( 'NONE', #27657, #7930, #47647 ) ;
#24376 = CARTESIAN_POINT ( 'NONE',  ( -48.47912675150885065, -189.7472609257535510, 6.938893903907228378E-15 ) ) ;
#24377 = CARTESIAN_POINT ( 'NONE',  ( -260.0000000000000000, -113.5000000000000000, -40.00000000000001421 ) ) ;
#24378 = DIRECTION ( 'NONE',  ( 0.000000000000000000, -0.000000000000000000, -1.000000000000000000 ) ) ;
#24379 = DIRECTION ( 'NONE',  ( 0.000000000000000000, 0.000000000000000000, 1.000000000000000000 ) ) ;
#24380 = EDGE_CURVE ( 'NONE', #14956, #2833, #42739, .T. ) ;
#24381 = ORIENTED_EDGE ( 'NONE', *, *, #13872, .F. ) ;
#24382 = ORIENTED_EDGE ( 'NONE', *, *, #9116, .F. ) ;
#24383 = DIRECTION ( 'NONE',  ( 0.000000000000000000, -1.000000000000000000, 0.000000000000000000 ) ) ;
#24384 = VECTOR ( 'NONE', #8598, 1000.000000000000000 ) ;
#24385 = VERTEX_POINT ( 'NONE', #51164 ) ;
#24386 = CARTESIAN_POINT ( 'NONE',  ( -48.47912675150885065, -183.6283474603465606, 6.938893903907228378E-15 ) ) ;
#24387 = FACE_OUTER_BOUND ( 'NONE', #999, .T. ) ;
#24388 = PLANE ( 'NONE',  #31383 ) ;
#24389 = DIRECTION ( 'NONE',  ( 0.000000000000000000, -0.5680647467311625842, -0.8229838658936516893 ) ) ;
#24390 = DIRECTION ( 'NONE',  ( 0.000000000000000000, -0.1205366802553303196, -0.9927088740980530845 ) ) ;
#24391 = ORIENTED_EDGE ( 'NONE', *, *, #14402, .T. ) ;
#24394 = ORIENTED_EDGE ( 'NONE', *, *, #10533, .F. ) ;
#24393 = DIRECTION ( 'NONE',  ( -0.000000000000000000, 1.000000000000000000, -0.000000000000000000 ) ) ;
#24392 = PLANE ( 'NONE',  #28344 ) ;
#24395 = ORIENTED_EDGE ( 'NONE', *, *, #37829, .F. ) ;
#24396 = LINE ( 'NONE', #48849, #3863 ) ;
#24397 = EDGE_LOOP ( 'NONE', ( #25421, #47181, #33909, #51690 ) ) ;
#24398 = CARTESIAN_POINT ( 'NONE',  ( -48.77118352214583297, -189.7472609257535510, 0.9564009842765270886 ) ) ;
#24399 = CIRCLE ( 'NONE', #31114, 125.0000000000000000 ) ;
#24400 = VERTEX_POINT ( 'NONE', #30908 ) ;
#24401 = EDGE_CURVE ( 'NONE', #50764, #18911, #23291, .T. ) ;
#24402 = CARTESIAN_POINT ( 'NONE',  ( -336.3521761649654422, -100.1170788342122080, 54.23253582808833073 ) ) ;
#24403 = EDGE_CURVE ( 'NONE', #27379, #11274, #35689, .T. ) ;
#24404 = DIRECTION ( 'NONE',  ( -0.000000000000000000, 1.000000000000000000, -0.000000000000000000 ) ) ;
#24405 = ORIENTED_EDGE ( 'NONE', *, *, #41361, .F. ) ;
#24407 = DIRECTION ( 'NONE',  ( -0.8455960035018199594, 0.000000000000000000, -0.5338233779648003940 ) ) ;
#24406 = DIRECTION ( 'NONE',  ( 0.5338233779647948429, 0.000000000000000000, -0.8455960035018234011 ) ) ;
#24408 = VERTEX_POINT ( 'NONE', #27205 ) ;
#24409 = EDGE_CURVE ( 'NONE', #21525, #24900, #39307, .T. ) ;
#24410 = VECTOR ( 'NONE', #25984, 1000.000000000000000 ) ;
#24411 = EDGE_CURVE ( 'NONE', #4174, #19776, #15405, .T. ) ;
#24412 = ORIENTED_EDGE ( 'NONE', *, *, #11312, .F. ) ;
#24413 = DIRECTION ( 'NONE',  ( 0.000000000000000000, 0.000000000000000000, 1.000000000000000000 ) ) ;
#24414 = CARTESIAN_POINT ( 'NONE',  ( -85.77912150413021664, -193.5000000000000000, -119.3051146910911768 ) ) ;
#24415 = CARTESIAN_POINT ( 'NONE',  ( -49.40581635894069024, -189.7472609257535510, 0.3758275821142362250 ) ) ;
#24416 = CARTESIAN_POINT ( 'NONE',  ( -336.3521761649654422, -78.25545813661345562, 37.90245108779119931 ) ) ;
#24417 = DIRECTION ( 'NONE',  ( 0.000000000000000000, -1.000000000000000000, -0.000000000000000000 ) ) ;
#24418 = ORIENTED_EDGE ( 'NONE', *, *, #10876, .F. ) ;
#24419 = APPLICATION_PROTOCOL_DEFINITION ( 'draft international standard', 'automotive_design', 1998, #7870 ) ;
#24420 = CARTESIAN_POINT ( 'NONE',  ( -51.83230197877468015, -177.1207230881787780, 123.9551692589637639 ) ) ;
#24421 = DIRECTION ( 'NONE',  ( 0.000000000000000000, 0.000000000000000000, -1.000000000000000000 ) ) ;
#24422 = CARTESIAN_POINT ( 'NONE',  ( 69.88207517204676833, -189.7472609257535510, 40.19484891390058579 ) ) ;
#24423 = CARTESIAN_POINT ( 'NONE',  ( -19.92568551777507224, -193.5000000000000000, -121.6951149130962904 ) ) ;
#24424 = ORIENTED_EDGE ( 'NONE', *, *, #39397, .T. ) ;
#24425 = AXIS2_PLACEMENT_3D ( 'NONE', #3832, #51939, #8536 ) ;
#24426 = FACE_OUTER_BOUND ( 'NONE', #44169, .T. ) ;
#24427 = ADVANCED_FACE ( 'NONE', ( #130 ), #9074, .T. ) ;
#24428 = CARTESIAN_POINT ( 'NONE',  ( -48.47912675150885065, -183.6283474603465606, 6.938893903907228378E-15 ) ) ;
#24429 = CARTESIAN_POINT ( 'NONE',  ( -170.0502155641509319, -177.1207230881787780, -29.07697310430878090 ) ) ;
#24430 = VERTEX_POINT ( 'NONE', #16959 ) ;
#24431 = ORIENTED_EDGE ( 'NONE', *, *, #23167, .F. ) ;
#24432 = ORIENTED_EDGE ( 'NONE', *, *, #33427, .F. ) ;
#24433 = EDGE_CURVE ( 'NONE', #50666, #34406, #37351, .T. ) ;
#24434 = CARTESIAN_POINT ( 'NONE',  ( -48.47912675150885065, -175.3837268820161057, 6.938893903907228378E-15 ) ) ;
#24435 = CARTESIAN_POINT ( 'NONE',  ( 0.000000000000000000, -178.6659583184393796, 20.92168833551003004 ) ) ;
#24436 = DIRECTION ( 'NONE',  ( -0.000000000000000000, 1.000000000000000000, -0.000000000000000000 ) ) ;
#24437 = DIRECTION ( 'NONE',  ( -0.000000000000000000, 1.000000000000000000, -0.000000000000000000 ) ) ;
#24438 = AXIS2_PLACEMENT_3D ( 'NONE', #32879, #20028, #40243 ) ;
#24439 = VERTEX_POINT ( 'NONE', #44546 ) ;
#24440 = DIRECTION ( 'NONE',  ( 0.000000000000000000, 0.000000000000000000, -1.000000000000000000 ) ) ;
#24441 = CARTESIAN_POINT ( 'NONE',  ( 52.36832552120770146, -193.5000000000000000, -72.15117186584490128 ) ) ;
#24442 = ORIENTED_EDGE ( 'NONE', *, *, #39677, .F. ) ;
#24443 = CIRCLE ( 'NONE', #4298, 125.0000000000000000 ) ;
#24444 = ORIENTED_EDGE ( 'NONE', *, *, #12717, .T. ) ;
#24445 = CIRCLE ( 'NONE', #17645, 60.00000000000000000 ) ;
#24446 = VERTEX_POINT ( 'NONE', #40849 ) ;
#24447 = DIRECTION ( 'NONE',  ( -1.000000000000000000, -0.000000000000000000, 0.000000000000000000 ) ) ;
#24448 = FACE_OUTER_BOUND ( 'NONE', #10927, .T. ) ;
#24449 = LINE ( 'NONE', #8950, #49977 ) ;
#24451 = DIRECTION ( 'NONE',  ( -0.000000000000000000, 0.9927088740980526405, -0.1205366802553337890 ) ) ;
#24450 = CARTESIAN_POINT ( 'NONE',  ( -166.0019676197264005, -189.7472609257535510, 39.55227055146323067 ) ) ;
#24452 = AXIS2_PLACEMENT_3D ( 'NONE', #28441, #24259, #44747 ) ;
#24453 = FACE_OUTER_BOUND ( 'NONE', #21478, .T. ) ;
#24454 = ORIENTED_EDGE ( 'NONE', *, *, #23297, .F. ) ;
#24455 = CARTESIAN_POINT ( 'NONE',  ( 36.84288420123323249, -177.1207230881787780, 91.35181687837503262 ) ) ;
#24456 = CARTESIAN_POINT ( 'NONE',  ( -170.0000000000000284, -173.5000000000000284, -60.00000000000001421 ) ) ;
#24457 = ORIENTED_EDGE ( 'NONE', *, *, #25097, .F. ) ;
#24458 = EDGE_CURVE ( 'NONE', #11058, #41322, #47449, .T. ) ;
#24460 = ADVANCED_FACE ( 'NONE', ( #29018 ), #16710, .F. ) ;
#24459 = DIRECTION ( 'NONE',  ( 0.000000000000000000, -1.000000000000000000, -0.000000000000000000 ) ) ;
#24461 = DIRECTION ( 'NONE',  ( 0.000000000000000000, 0.000000000000000000, -1.000000000000000000 ) ) ;
#24463 = DIRECTION ( 'NONE',  ( 0.000000000000000000, -6.846375318521798245E-14, -1.000000000000000000 ) ) ;
#24462 = DIRECTION ( 'NONE',  ( 0.000000000000000000, -1.000000000000000000, 0.000000000000000000 ) ) ;
#24464 = ORIENTED_EDGE ( 'NONE', *, *, #48396, .T. ) ;
#24465 = DIRECTION ( 'NONE',  ( -0.3482016354343866471, 0.000000000000000000, -0.9374196611341253371 ) ) ;
#24466 = DIRECTION ( 'NONE',  ( -0.9646355819083576311, 0.000000000000000000, -0.2635871660690715101 ) ) ;
#24467 = ORIENTED_EDGE ( 'NONE', *, *, #26000, .T. ) ;
#24468 = CARTESIAN_POINT ( 'NONE',  ( -173.4291566779743050, -193.5000000000000000, 3.534122433558352760 ) ) ;
#24469 = CARTESIAN_POINT ( 'NONE',  ( -330.4913330509368166, -116.8846903019851311, -58.63009191191288494 ) ) ;
#24470 = VECTOR ( 'NONE', #37223, 1000.000000000000000 ) ;
#24471 = CARTESIAN_POINT ( 'NONE',  ( -156.2577088867455473, -177.1207230881787780, -63.31490529818420754 ) ) ;
#24472 = EDGE_LOOP ( 'NONE', ( #42095, #27924, #50654, #6502 ) ) ;
#24473 = CARTESIAN_POINT ( 'NONE',  ( -135.6699833737243353, -175.3837268820161057, 89.56983042009326823 ) ) ;
#24474 = VECTOR ( 'NONE', #50417, 1000.000000000000000 ) ;
#24475 = LINE ( 'NONE', #20530, #39860 ) ;
#24476 = VERTEX_POINT ( 'NONE', #12215 ) ;
#24477 = CARTESIAN_POINT ( 'NONE',  ( 8.448131207122532516, -193.5000000000000000, 111.2847127925100352 ) ) ;
#24478 = ORIENTED_EDGE ( 'NONE', *, *, #2923, .T. ) ;
#24479 = LINE ( 'NONE', #43936, #25628 ) ;
#24480 = DIRECTION ( 'NONE',  ( -0.000000000000000000, 1.000000000000000000, -0.000000000000000000 ) ) ;
#24481 = EDGE_CURVE ( 'NONE', #13211, #17151, #28965, .T. ) ;
#24482 = CARTESIAN_POINT ( 'NONE',  ( -162.7543581613524282, -193.5000000000000000, 50.65739320402010293 ) ) ;
#24483 = PLANE ( 'NONE',  #14690 ) ;
#24484 = PLANE ( 'NONE',  #9844 ) ;
#24485 = AXIS2_PLACEMENT_3D ( 'NONE', #6922, #2971, #35039 ) ;
#24486 = ADVANCED_FACE ( 'NONE', ( #25108 ), #47973, .T. ) ;
#24487 = DIRECTION ( 'NONE',  ( 0.000000000000000000, 0.000000000000000000, 1.000000000000000000 ) ) ;
#24488 = VECTOR ( 'NONE', #49358, 1000.000000000000000 ) ;
#24489 = CARTESIAN_POINT ( 'NONE',  ( 31.28129687248616619, -193.5000000000000000, 96.24590808611479531 ) ) ;
#24490 = LINE ( 'NONE', #40509, #1242 ) ;
#24492 = ORIENTED_EDGE ( 'NONE', *, *, #8294, .F. ) ;
#24491 = DIRECTION ( 'NONE',  ( -0.000000000000000000, 1.000000000000000000, -0.000000000000000000 ) ) ;
#24493 = ORIENTED_EDGE ( 'NONE', *, *, #1663, .T. ) ;
#24494 = CARTESIAN_POINT ( 'NONE',  ( 0.000000000000000000, -74.94395191227431496, -33.51582005713827783 ) ) ;
#24495 = EDGE_CURVE ( 'NONE', #20143, #50250, #24567, .T. ) ;
#24496 = CARTESIAN_POINT ( 'NONE',  ( -98.71382891444399377, -175.3837268820161057, -114.4616734920523555 ) ) ;
#24497 = ORIENTED_EDGE ( 'NONE', *, *, #10184, .T. ) ;
#24498 = ORIENTED_EDGE ( 'NONE', *, *, #2145, .F. ) ;
#24499 = VERTEX_POINT ( 'NONE', #24060 ) ;
#24500 = DIRECTION ( 'NONE',  ( -0.000000000000000000, 1.000000000000000000, -0.000000000000000000 ) ) ;
#24501 = VECTOR ( 'NONE', #17199, 1000.000000000000114 ) ;
#24502 = CARTESIAN_POINT ( 'NONE',  ( -330.4913330509368166, -130.2355952558261549, 59.62073260661674112 ) ) ;
#24503 = CARTESIAN_POINT ( 'NONE',  ( -336.3521761649654422, -174.5186198893880771, 29.74944317415823392 ) ) ;
#24504 = CIRCLE ( 'NONE', #54, 60.00000000000000000 ) ;
#24505 = ORIENTED_EDGE ( 'NONE', *, *, #42848, .T. ) ;
#24506 = ORIENTED_EDGE ( 'NONE', *, *, #38897, .T. ) ;
#24508 = VERTEX_POINT ( 'NONE', #20626 ) ;
#24507 = AXIS2_PLACEMENT_3D ( 'NONE', #16294, #50443, #34139 ) ;
#24509 = EDGE_CURVE ( 'NONE', #39324, #5146, #42373, .T. ) ;
#24510 = LINE ( 'NONE', #51604, #4834 ) ;
#24511 = CARTESIAN_POINT ( 'NONE',  ( -139.4082623311987277, -189.7472609257535510, 84.30834960113001841 ) ) ;
#24513 = ORIENTED_EDGE ( 'NONE', *, *, #4414, .T. ) ;
#24512 = DIRECTION ( 'NONE',  ( -0.6965510290629932655, 0.000000000000000000, -0.7175072570443347120 ) ) ;
#24514 = DIRECTION ( 'NONE',  ( 1.000000000000000000, 0.000000000000000000, -0.000000000000000000 ) ) ;
#24515 = FACE_OUTER_BOUND ( 'NONE', #14758, .T. ) ;
#24516 = ORIENTED_EDGE ( 'NONE', *, *, #17614, .T. ) ;
#24517 = PLANE ( 'NONE',  #12939 ) ;
#24518 = EDGE_CURVE ( 'NONE', #27048, #47761, #32715, .T. ) ;
#24519 = DIRECTION ( 'NONE',  ( 1.000000000000000000, 0.000000000000000000, 0.000000000000000000 ) ) ;
#24520 = EDGE_CURVE ( 'NONE', #51281, #19239, #384, .T. ) ;
#24521 = CARTESIAN_POINT ( 'NONE',  ( -48.13092511607445090, -193.5000000000000000, -0.9374196611341135688 ) ) ;
#24522 = DIRECTION ( 'NONE',  ( -0.6068001458185945385, 0.000000000000000000, 0.7948544414133523750 ) ) ;
#24523 = VECTOR ( 'NONE', #31814, 1000.000000000000000 ) ;
#24524 = VECTOR ( 'NONE', #22793, 1000.000000000000114 ) ;
#24525 = ORIENTED_EDGE ( 'NONE', *, *, #21021, .T. ) ;
#24526 = AXIS2_PLACEMENT_3D ( 'NONE', #20364, #43761, #19590 ) ;
#24527 = EDGE_CURVE ( 'NONE', #27120, #36746, #36389, .T. ) ;
#24528 = ORIENTED_EDGE ( 'NONE', *, *, #47267, .F. ) ;
#24529 = VECTOR ( 'NONE', #5928, 1000.000000000000114 ) ;
#24530 = LINE ( 'NONE', #48466, #44049 ) ;
#24531 = PLANE ( 'NONE',  #6552 ) ;
#24532 = ORIENTED_EDGE ( 'NONE', *, *, #23098, .T. ) ;
#24533 = DIRECTION ( 'NONE',  ( 0.000000000000000000, -0.6631226582408017434, -0.7485107481710954191 ) ) ;
#24534 = CARTESIAN_POINT ( 'NONE',  ( -13.05859477122062806, -193.5000000000000000, -118.8334608768479654 ) ) ;
#24535 = ADVANCED_FACE ( 'NONE', ( #12729 ), #4878, .F. ) ;
#24536 = ORIENTED_EDGE ( 'NONE', *, *, #3377, .F. ) ;
#24537 = CARTESIAN_POINT ( 'NONE',  ( 47.70255505652111339, -175.3837268820161057, 78.26291788638732783 ) ) ;
#24538 = DIRECTION ( 'NONE',  ( -0.000000000000000000, 0.7485107481711089639, 0.6631226582407863113 ) ) ;
#24539 = ORIENTED_EDGE ( 'NONE', *, *, #7338, .F. ) ;
#24540 = DIRECTION ( 'NONE',  ( 0.000000000000000000, 1.000000000000000000, -0.000000000000000000 ) ) ;
#24541 = ORIENTED_EDGE ( 'NONE', *, *, #15090, .T. ) ;
#24542 = LINE ( 'NONE', #20336, #42968 ) ;
#24543 = EDGE_CURVE ( 'NONE', #13751, #6162, #20108, .T. ) ;
#24544 = VERTEX_POINT ( 'NONE', #20905 ) ;
#24545 = VECTOR ( 'NONE', #36229, 1000.000000000000114 ) ;
#24546 = DIRECTION ( 'NONE',  ( -0.000000000000000000, 0.4647231720437664526, -0.8854560256532110207 ) ) ;
#24547 = FACE_OUTER_BOUND ( 'NONE', #13660, .T. ) ;
#24548 = CARTESIAN_POINT ( 'NONE',  ( 75.46126020185813843, -193.5000000000000000, 3.844569333773215192 ) ) ;
#24549 = DIRECTION ( 'NONE',  ( 0.000000000000000000, 0.000000000000000000, -1.000000000000000000 ) ) ;
#24550 = AXIS2_PLACEMENT_3D ( 'NONE', #44936, #40984, #36512 ) ;
#24551 = ORIENTED_EDGE ( 'NONE', *, *, #28832, .F. ) ;
#24552 = FACE_OUTER_BOUND ( 'NONE', #29798, .T. ) ;
#24553 = ORIENTED_EDGE ( 'NONE', *, *, #32052, .T. ) ;
#24554 = ORIENTED_EDGE ( 'NONE', *, *, #29448, .F. ) ;
#24555 = DIRECTION ( 'NONE',  ( -0.000000000000000000, 1.000000000000000000, -0.000000000000000000 ) ) ;
#24557 = ORIENTED_EDGE ( 'NONE', *, *, #31286, .F. ) ;
#24556 = CARTESIAN_POINT ( 'NONE',  ( 0.000000000000000000, -182.0698235717851787, 7.111664135064491354 ) ) ;
#24558 = ORIENTED_EDGE ( 'NONE', *, *, #21753, .T. ) ;
#24559 = LINE ( 'NONE', #48232, #9369 ) ;
#24560 = AXIS2_PLACEMENT_3D ( 'NONE', #25163, #41175, #17278 ) ;
#24561 = VECTOR ( 'NONE', #28527, 999.9999999999998863 ) ;
#24562 = DIRECTION ( 'NONE',  ( -0.000000000000000000, 1.000000000000000000, -0.000000000000000000 ) ) ;
#24563 = CARTESIAN_POINT ( 'NONE',  ( 30.05499637021958392, -193.5000000000000000, -97.24912084693205827 ) ) ;
#24564 = CIRCLE ( 'NONE', #17865, 60.00000000000000000 ) ;
#24565 = CIRCLE ( 'NONE', #35472, 125.0000000000000000 ) ;
#24566 = ORIENTED_EDGE ( 'NONE', *, *, #47209, .T. ) ;
#24567 = LINE ( 'NONE', #40580, #13876 ) ;
#24568 = ORIENTED_EDGE ( 'NONE', *, *, #37821, .F. ) ;
#24569 = DIRECTION ( 'NONE',  ( 0.000000000000000000, -0.000000000000000000, -1.000000000000000000 ) ) ;
#24570 = PLANE ( 'NONE',  #30853 ) ;
#24571 = EDGE_CURVE ( 'NONE', #26067, #9084, #32191, .T. ) ;
#24572 = DIRECTION ( 'NONE',  ( 0.1768902751225666370, 0.000000000000000000, 0.9842305779475979399 ) ) ;
#24573 = CARTESIAN_POINT ( 'NONE',  ( 10.73478887071927623, -177.1207230881787780, -110.0850225811106924 ) ) ;
#24574 = EDGE_LOOP ( 'NONE', ( #37694, #43020, #12840, #19057 ) ) ;
#24575 = EDGE_LOOP ( 'NONE', ( #27183, #35398, #33190, #9384 ) ) ;
#24576 = ORIENTED_EDGE ( 'NONE', *, *, #20147, .T. ) ;
#24577 = DIRECTION ( 'NONE',  ( 0.2635871660690581320, 0.000000000000000000, 0.9646355819083614058 ) ) ;
#24578 = PLANE ( 'NONE',  #19 ) ;
#24579 = LINE ( 'NONE', #40596, #7488 ) ;
#24580 = FACE_BOUND ( 'NONE', #23197, .T. ) ;
#24581 = DIRECTION ( 'NONE',  ( -0.000000000000000000, 1.000000000000000000, -0.000000000000000000 ) ) ;
#24582 = AXIS2_PLACEMENT_3D ( 'NONE', #16749, #13558, #49315 ) ;
#24583 = ORIENTED_EDGE ( 'NONE', *, *, #6975, .F. ) ;
#24584 = EDGE_CURVE ( 'NONE', #51089, #8376, #48237, .T. ) ;
#24585 = EDGE_CURVE ( 'NONE', #6023, #11792, #30619, .T. ) ;
#24586 = CIRCLE ( 'NONE', #45581, 125.0000000000000000 ) ;
#24587 = ORIENTED_EDGE ( 'NONE', *, *, #14379, .F. ) ;
#24589 = VERTEX_POINT ( 'NONE', #45085 ) ;
#24588 = FACE_OUTER_BOUND ( 'NONE', #43595, .T. ) ;
#24590 = ORIENTED_EDGE ( 'NONE', *, *, #26584, .T. ) ;
#24591 = EDGE_CURVE ( 'NONE', #12134, #2552, #38207, .T. ) ;
#24592 = PLANE ( 'NONE',  #37522 ) ;
#24593 = DIRECTION ( 'NONE',  ( 1.000000000000000000, -0.000000000000000000, -0.000000000000000000 ) ) ;
#24594 = LINE ( 'NONE', #4627, #4418 ) ;
#24595 = CYLINDRICAL_SURFACE ( 'NONE', #2440, 4.000000000000003553 ) ;
#24596 = ORIENTED_EDGE ( 'NONE', *, *, #35799, .F. ) ;
#24597 = FACE_OUTER_BOUND ( 'NONE', #38821, .T. ) ;
#24598 = AXIS2_PLACEMENT_3D ( 'NONE', #50488, #42317, #13961 ) ;
#24599 = ORIENTED_EDGE ( 'NONE', *, *, #11988, .T. ) ;
#24600 = AXIS2_PLACEMENT_3D ( 'NONE', #26955, #42990, #18812 ) ;
#24601 = VERTEX_POINT ( 'NONE', #42410 ) ;
#24602 = DIRECTION ( 'NONE',  ( 0.000000000000000000, -0.000000000000000000, 1.000000000000000000 ) ) ;
#24603 = AXIS2_PLACEMENT_3D ( 'NONE', #46300, #45771, #9766 ) ;
#24604 = LINE ( 'NONE', #16995, #30362 ) ;
#24605 = DIRECTION ( 'NONE',  ( -0.000000000000000000, 1.000000000000000000, -0.000000000000000000 ) ) ;
#24606 = CARTESIAN_POINT ( 'NONE',  ( -330.4913330509368166, -182.0095552316575152, 7.608018572113473432 ) ) ;
#24607 = DIRECTION ( 'NONE',  ( 0.8455960035018234011, 0.000000000000000000, 0.5338233779647948429 ) ) ;
#24608 = LINE ( 'NONE', #40621, #21201 ) ;
#24609 = VECTOR ( 'NONE', #31151, 1000.000000000000000 ) ;
#24610 = EDGE_LOOP ( 'NONE', ( #29900, #21659, #33322, #47207 ) ) ;
#24611 = DIRECTION ( 'NONE',  ( 0.000000000000000000, 0.000000000000000000, -1.000000000000000000 ) ) ;
#24612 = DIRECTION ( 'NONE',  ( 0.000000000000000000, 0.000000000000000000, 1.000000000000000000 ) ) ;
#24613 = LINE ( 'NONE', #40627, #18588 ) ;
#24614 = FACE_BOUND ( 'NONE', #38704, .T. ) ;
#24615 = ORIENTED_EDGE ( 'NONE', *, *, #20788, .F. ) ;
#24616 = CARTESIAN_POINT ( 'NONE',  ( -330.4913330509368166, -66.09477493971897388, 13.63415328425216622 ) ) ;
#24617 = ORIENTED_EDGE ( 'NONE', *, *, #4779, .T. ) ;
#24618 = AXIS2_PLACEMENT_3D ( 'NONE', #42314, #6331, #11800 ) ;
#24619 = DIRECTION ( 'NONE',  ( -0.000000000000000000, 0.000000000000000000, 1.000000000000000000 ) ) ;
#24620 = VERTEX_POINT ( 'NONE', #14055 ) ;
#24621 = DIRECTION ( 'NONE',  ( 0.000000000000000000, 0.000000000000000000, -1.000000000000000000 ) ) ;
#24622 = ORIENTED_EDGE ( 'NONE', *, *, #29520, .F. ) ;
#24623 = AXIS2_PLACEMENT_3D ( 'NONE', #22124, #26057, #42086 ) ;
#24624 = DIRECTION ( 'NONE',  ( -0.9890401873221654760, 0.000000000000000000, 0.1476465640024710868 ) ) ;
#24625 = FACE_BOUND ( 'NONE', #25964, .T. ) ;
#24627 = ORIENTED_EDGE ( 'NONE', *, *, #4956, .T. ) ;
#24626 = CARTESIAN_POINT ( 'NONE',  ( -339.1964088526558498, -162.2499814621216672, -44.49369547121515467 ) ) ;
#24628 = EDGE_CURVE ( 'NONE', #9774, #45236, #9581, .T. ) ;
#24629 = EDGE_CURVE ( 'NONE', #44745, #4167, #2949, .T. ) ;
#24630 = EDGE_CURVE ( 'NONE', #33552, #34512, #26425, .T. ) ;
#24631 = CARTESIAN_POINT ( 'NONE',  ( -49.40581635894068313, -183.6283474603465606, -0.3758275821142418316 ) ) ;
#24632 = ORIENTED_EDGE ( 'NONE', *, *, #38831, .F. ) ;
#24633 = EDGE_CURVE ( 'NONE', #44162, #48670, #37431, .T. ) ;
#24634 = ORIENTED_EDGE ( 'NONE', *, *, #46430, .T. ) ;
#24635 = CARTESIAN_POINT ( 'NONE',  ( 41.00573479224733120, -177.1207230881787780, -87.27805883780175122 ) ) ;
#24636 = VECTOR ( 'NONE', #16986, 1000.000000000000000 ) ;
#24637 = ORIENTED_EDGE ( 'NONE', *, *, #1188, .F. ) ;
#24638 = ADVANCED_FACE ( 'NONE', ( #46370 ), #33752, .T. ) ;
#24639 = DIRECTION ( 'NONE',  ( 0.000000000000000000, 0.000000000000000000, -1.000000000000000000 ) ) ;
#24640 = ADVANCED_FACE ( 'NONE', ( #45852 ), #50319, .F. ) ;
#24641 = LINE ( 'NONE', #27617, #18618 ) ;
#24642 = PLANE ( 'NONE',  #43951 ) ;
#24643 = EDGE_CURVE ( 'NONE', #42167, #45648, #39844, .T. ) ;
#24644 = EDGE_CURVE ( 'NONE', #27476, #23880, #35656, .T. ) ;
#24645 = CARTESIAN_POINT ( 'NONE',  ( 64.44365795514079309, -193.5000000000000000, -53.60452120946194299 ) ) ;
#24646 = CARTESIAN_POINT ( 'NONE',  ( 41.41233698655026529, -177.1207230881787780, 86.85922373029362120 ) ) ;
#24647 = ORIENTED_EDGE ( 'NONE', *, *, #31753, .T. ) ;
#24650 = ORIENTED_EDGE ( 'NONE', *, *, #36657, .F. ) ;
#24649 = CARTESIAN_POINT ( 'NONE',  ( 75.17589904515345722, -175.3837268820161057, -18.28755301364250485 ) ) ;
#24648 = FACE_OUTER_BOUND ( 'NONE', #4511, .T. ) ;
#24651 = VERTEX_POINT ( 'NONE', #46121 ) ;
#24652 = EDGE_CURVE ( 'NONE', #32761, #26723, #3769, .T. ) ;
#24653 = DIRECTION ( 'NONE',  ( -0.000000000000000000, -0.5680647467311596976, -0.8229838658936536877 ) ) ;
#24654 = ORIENTED_EDGE ( 'NONE', *, *, #41015, .T. ) ;
#24655 = CARTESIAN_POINT ( 'NONE',  ( -160.4991136281923616, -175.3837268820161057, 53.17445600718625798 ) ) ;
#24656 = VECTOR ( 'NONE', #22812, 1000.000000000000000 ) ;
#24657 = VERTEX_POINT ( 'NONE', #10100 ) ;
#24658 = EDGE_CURVE ( 'NONE', #27596, #33838, #5485, .T. ) ;
#24659 = DIRECTION ( 'NONE',  ( -0.000000000000000000, 0.9927088740980538617, -0.1205366802553232974 ) ) ;
#24660 = DIRECTION ( 'NONE',  ( -0.9473263538541923934, 0.000000000000000000, 0.3202698538628350744 ) ) ;
#24661 = ORIENTED_EDGE ( 'NONE', *, *, #48090, .T. ) ;
#24663 = DIRECTION ( 'NONE',  ( 0.000000000000000000, 0.1205366802553199113, -0.9927088740980544168 ) ) ;
#24662 = CYLINDRICAL_SURFACE ( 'NONE', #41758, 4.999999999999997335 ) ;
#24664 = ORIENTED_EDGE ( 'NONE', *, *, #49091, .F. ) ;
#24665 = AXIS2_PLACEMENT_3D ( 'NONE', #27766, #3602, #35658 ) ;
#24666 = ORIENTED_EDGE ( 'NONE', *, *, #250, .T. ) ;
#24667 = CARTESIAN_POINT ( 'NONE',  ( -336.3521761649654422, -181.7525362123217292, 9.724760635742144999 ) ) ;
#24668 = CARTESIAN_POINT ( 'NONE',  ( -48.24424070572786860, -193.5000000000000000, -0.9720229140804037549 ) ) ;
#24669 = DIRECTION ( 'NONE',  ( 0.000000000000000000, -0.5680647467311510379, 0.8229838658936596829 ) ) ;
#24670 = PLANE ( 'NONE',  #3138 ) ;
#24671 = DIRECTION ( 'NONE',  ( -0.000000000000000000, -0.1205366802553164696, 0.9927088740980548609 ) ) ;
#24672 = CARTESIAN_POINT ( 'NONE',  ( -48.47912675150885065, -177.1207230881787780, 6.938893903907228378E-15 ) ) ;
#24673 = PRODUCT_CONTEXT ( 'NONE', #6200, 'mechanical' ) ;
#24674 = DIRECTION ( 'NONE',  ( 0.000000000000000000, -1.000000000000000000, -0.000000000000000000 ) ) ;
#24675 = AXIS2_PLACEMENT_3D ( 'NONE', #2147, #34219, #17688 ) ;
#24676 = LINE ( 'NONE', #39650, #6185 ) ;
#24677 = EDGE_CURVE ( 'NONE', #14215, #7533, #13272, .T. ) ;
#24678 = CARTESIAN_POINT ( 'NONE',  ( -339.1964088526558498, -84.75001853787875916, -44.49369547121548862 ) ) ;
#24679 = PLANE ( 'NONE',  #15384 ) ;
#24680 = VERTEX_POINT ( 'NONE', #45597 ) ;
#24681 = ORIENTED_EDGE ( 'NONE', *, *, #18548, .F. ) ;
#24682 = DIRECTION ( 'NONE',  ( -0.000000000000000000, 1.000000000000000000, -0.000000000000000000 ) ) ;
#24683 = DIRECTION ( 'NONE',  ( -0.000000000000000000, 0.7485107481710999711, -0.6631226582407964143 ) ) ;
#24684 = DIRECTION ( 'NONE',  ( -0.000000000000000000, 1.000000000000000000, 0.000000000000000000 ) ) ;
#24685 = ORIENTED_EDGE ( 'NONE', *, *, #37879, .F. ) ;
#24686 = ORIENTED_EDGE ( 'NONE', *, *, #14086, .F. ) ;
#24687 = ORIENTED_EDGE ( 'NONE', *, *, #7006, .T. ) ;
#24688 = EDGE_CURVE ( 'NONE', #9490, #39530, #5914, .T. ) ;
#24689 = DIRECTION ( 'NONE',  ( -0.000000000000000000, -1.000000000000000000, -0.000000000000000000 ) ) ;
#24690 = DIRECTION ( 'NONE',  ( 0.6965510290629982615, 0.000000000000000000, -0.7175072570443298270 ) ) ;
#24691 = DIRECTION ( 'NONE',  ( -0.4031234292879730674, 0.000000000000000000, 0.9151456172430181280 ) ) ;
#24692 = CARTESIAN_POINT ( 'NONE',  ( -48.47912675150885065, -189.7472609257535510, 6.938893903907228378E-15 ) ) ;
#24693 = VECTOR ( 'NONE', #21889, 1000.000000000000000 ) ;
#24694 = ORIENTED_EDGE ( 'NONE', *, *, #37666, .T. ) ;
#24695 = AXIS2_PLACEMENT_3D ( 'NONE', #13104, #21515, #16546 ) ;
#24696 = ADVANCED_FACE ( 'NONE', ( #26116 ), #37950, .T. ) ;
#24697 = EDGE_CURVE ( 'NONE', #27708, #23768, #45344, .T. ) ;
#24698 = ADVANCED_FACE ( 'NONE', ( #22454 ), #17992, .F. ) ;
#24699 = DIRECTION ( 'NONE',  ( 1.000000000000000000, -0.000000000000000000, -0.000000000000000000 ) ) ;
#24700 = EDGE_CURVE ( 'NONE', #26506, #24824, #22185, .T. ) ;
#24701 = CARTESIAN_POINT ( 'NONE',  ( -66.64622755927948106, -177.1207230881787780, 123.6727797384707372 ) ) ;
#24702 = ORIENTED_EDGE ( 'NONE', *, *, #1158, .F. ) ;
#24703 = AXIS2_PLACEMENT_3D ( 'NONE', #24036, #12459, #28478 ) ;
#24704 = EDGE_CURVE ( 'NONE', #22194, #27513, #29805, .T. ) ;
#24705 = DIRECTION ( 'NONE',  ( -0.000000000000000000, 1.000000000000000000, -0.000000000000000000 ) ) ;
#24706 = ORIENTED_EDGE ( 'NONE', *, *, #7669, .T. ) ;
#24707 = ORIENTED_EDGE ( 'NONE', *, *, #6695, .T. ) ;
#24708 = EDGE_CURVE ( 'NONE', #26407, #47996, #18075, .T. ) ;
#24709 = EDGE_CURVE ( 'NONE', #16046, #24680, #7155, .T. ) ;
#24710 = DIRECTION ( 'NONE',  ( 0.2920567706369833760, 0.000000000000000000, -0.9564009842765202052 ) ) ;
#24711 = ADVANCED_FACE ( 'NONE', ( #46895 ), #38970, .F. ) ;
#24712 = CIRCLE ( 'NONE', #43993, 125.0000000000000000 ) ;
#24713 = ADVANCED_FACE ( 'NONE', ( #10872 ), #23727, .T. ) ;
#24714 = CARTESIAN_POINT ( 'NONE',  ( -339.1964088526558498, -96.52406086224443982, -52.47426709956138069 ) ) ;
#24715 = PRODUCT_DEFINITION_SHAPE ( 'NONE', 'NONE',  #52046 ) ;
#24716 = DIRECTION ( 'NONE',  ( -0.7175072570443395970, 0.000000000000000000, 0.6965510290629882695 ) ) ;
#24719 = VERTEX_POINT ( 'NONE', #26890 ) ;
#24718 = DIRECTION ( 'NONE',  ( 0.000000000000000000, -1.000000000000000000, -0.000000000000000000 ) ) ;
#24717 = DIRECTION ( 'NONE',  ( 0.000000000000000000, 1.000000000000000000, 0.000000000000000000 ) ) ;
#24720 = EDGE_CURVE ( 'NONE', #34028, #32675, #30849, .T. ) ;
#24721 = CARTESIAN_POINT ( 'NONE',  ( -339.1964088526558498, -90.39567187580880159, -48.84008046109142498 ) ) ;
#24722 = ORIENTED_EDGE ( 'NONE', *, *, #12161, .F. ) ;
#24723 = FACE_OUTER_BOUND ( 'NONE', #15972, .T. ) ;
#24724 = CARTESIAN_POINT ( 'NONE',  ( -260.0000000000000000, -113.5000000000000000, 60.00000000000000711 ) ) ;
#24725 = ORIENTED_EDGE ( 'NONE', *, *, #17657, .F. ) ;
#24726 = EDGE_CURVE ( 'NONE', #21902, #50633, #18760, .T. ) ;
#24727 = CARTESIAN_POINT ( 'NONE',  ( -170.9669310976187830, -175.3837268820161057, -24.93467037017130394 ) ) ;
#24729 = CARTESIAN_POINT ( 'NONE',  ( 45.36094686508022988, -177.1207230881787780, -82.57748230379237953 ) ) ;
#24728 = DIRECTION ( 'NONE',  ( 0.000000000000000000, 0.5000000000000012212, -0.8660254037844378194 ) ) ;
#24730 = ORIENTED_EDGE ( 'NONE', *, *, #24628, .T. ) ;
#24731 = EDGE_CURVE ( 'NONE', #8921, #8740, #3256, .T. ) ;
#24732 = PLANE ( 'NONE',  #44142 ) ;
#24733 = CARTESIAN_POINT ( 'NONE',  ( -48.47912675150885065, -175.3837268820161057, 6.938893903907228378E-15 ) ) ;
#24734 = CARTESIAN_POINT ( 'NONE',  ( -47.49008656418669005, -177.1207230881787780, 0.1476465640024920423 ) ) ;
#24735 = ORIENTED_EDGE ( 'NONE', *, *, #4474, .T. ) ;
#24736 = CARTESIAN_POINT ( 'NONE',  ( -137.2624501260119985, -193.5000000000000000, 87.99159897727967916 ) ) ;
#24737 = CARTESIAN_POINT ( 'NONE',  ( -37.14819544345410662, -193.5000000000000000, 123.4817304940907121 ) ) ;
#24738 = VECTOR ( 'NONE', #48909, 1000.000000000000000 ) ;
#24739 = CARTESIAN_POINT ( 'NONE',  ( 59.70893145360470555, -189.7472609257535510, -60.59166255800331413 ) ) ;
#24740 = VECTOR ( 'NONE', #12401, 1000.000000000000000 ) ;
#24741 = ORIENTED_EDGE ( 'NONE', *, *, #5725, .F. ) ;
#24743 = VECTOR ( 'NONE', #35279, 1000.000000000000000 ) ;
#24742 = DIRECTION ( 'NONE',  ( 5.399917434947259359E-17, 1.000000000000000000, -0.000000000000000000 ) ) ;
#24744 = EDGE_CURVE ( 'NONE', #41591, #11493, #2478, .T. ) ;
#24745 = ORIENTED_EDGE ( 'NONE', *, *, #10877, .T. ) ;
#24746 = DIRECTION ( 'NONE',  ( -0.1182731709213730997, 0.000000000000000000, 0.9929810960135161402 ) ) ;
#24747 = ORIENTED_EDGE ( 'NONE', *, *, #28284, .F. ) ;
#24748 = DIRECTION ( 'NONE',  ( -0.000000000000000000, -1.000000000000000000, 0.000000000000000000 ) ) ;
#24749 = PLANE ( 'NONE',  #29461 ) ;
#24750 = AXIS2_PLACEMENT_3D ( 'NONE', #18397, #33639, #2366 ) ;
#24751 = CARTESIAN_POINT ( 'NONE',  ( -105.4063847101409408, -189.7472609257535510, -111.2847127925096515 ) ) ;
#24752 = FACE_OUTER_BOUND ( 'NONE', #51056, .T. ) ;
#24753 = DIRECTION ( 'NONE',  ( -0.000000000000000000, 1.000000000000000000, -0.000000000000000000 ) ) ;
#24754 = VECTOR ( 'NONE', #42356, 1000.000000000000000 ) ;
#24755 = DIRECTION ( 'NONE',  ( 0.000000000000000000, 0.000000000000000000, -1.000000000000000000 ) ) ;
#24756 = FACE_OUTER_BOUND ( 'NONE', #9172, .T. ) ;
#24757 = CARTESIAN_POINT ( 'NONE',  ( 7.859956736328458149, -175.3837268820161057, -111.5836353223468649 ) ) ;
#24759 = ORIENTED_EDGE ( 'NONE', *, *, #37307, .T. ) ;
#24758 = DIRECTION ( 'NONE',  ( 0.000000000000000000, 0.000000000000000000, 1.000000000000000000 ) ) ;
#24760 = ORIENTED_EDGE ( 'NONE', *, *, #22808, .T. ) ;
#24761 = ADVANCED_FACE ( 'NONE', ( #23482 ), #19290, .F. ) ;
#24762 = ADVANCED_FACE ( 'NONE', ( #35296 ), #27673, .F. ) ;
#24763 = DIRECTION ( 'NONE',  ( 0.1768902751225666370, 0.000000000000000000, 0.9842305779475979399 ) ) ;
#24764 = ORIENTED_EDGE ( 'NONE', *, *, #12038, .T. ) ;
#24765 = ORIENTED_EDGE ( 'NONE', *, *, #41486, .T. ) ;
#24766 = VECTOR ( 'NONE', #36767, 999.9999999999998863 ) ;
#24767 = ORIENTED_EDGE ( 'NONE', *, *, #42903, .T. ) ;
#24768 = DIRECTION ( 'NONE',  ( 0.000000000000000000, 0.000000000000000000, -1.000000000000000000 ) ) ;
#24769 = VECTOR ( 'NONE', #39516, 1000.000000000000000 ) ;
#24770 = VECTOR ( 'NONE', #34624, 1000.000000000000114 ) ;
#24771 = CARTESIAN_POINT ( 'NONE',  ( 50.70030191143630560, -183.6283474603465606, -76.08180419845319875 ) ) ;
#24772 = LINE ( 'NONE', #4279, #20742 ) ;
#24773 = ORIENTED_EDGE ( 'NONE', *, *, #41611, .F. ) ;
#24774 = ORIENTED_EDGE ( 'NONE', *, *, #5625, .T. ) ;
#24775 = CARTESIAN_POINT ( 'NONE',  ( 75.12566530717464275, -175.3837268820161057, 18.62405380494841722 ) ) ;
#24776 = CARTESIAN_POINT ( 'NONE',  ( -56.05401443572774411, -193.5000000000000000, 124.7702732086912931 ) ) ;
#24778 = ORIENTED_EDGE ( 'NONE', *, *, #5529, .T. ) ;
#24777 = LINE ( 'NONE', #12154, #15723 ) ;
#24780 = EDGE_CURVE ( 'NONE', #21924, #13387, #47392, .T. ) ;
#24779 = CIRCLE ( 'NONE', #2122, 125.0000000000000000 ) ;
#24781 = DIRECTION ( 'NONE',  ( 0.000000000000000000, 0.8854560256532126861, 0.4647231720437631775 ) ) ;
#24782 = AXIS2_PLACEMENT_3D ( 'NONE', #49546, #14308, #29292 ) ;
#24783 = DIRECTION ( 'NONE',  ( -0.000000000000000000, 1.000000000000000000, -0.000000000000000000 ) ) ;
#24784 = VERTEX_POINT ( 'NONE', #26647 ) ;
#24785 = DIRECTION ( 'NONE',  ( 0.5085311186492216251, 0.000000000000000000, -0.8610436117673548884 ) ) ;
#24786 = ORIENTED_EDGE ( 'NONE', *, *, #11476, .F. ) ;
#24787 = DIRECTION ( 'NONE',  ( -0.000000000000000000, 1.000000000000000000, -0.000000000000000000 ) ) ;
#24788 = AXIS2_PLACEMENT_3D ( 'NONE', #39950, #47869, #11842 ) ;
#24789 = CARTESIAN_POINT ( 'NONE',  ( 0.000000000000000000, 65.00000000000000000, 0.000000000000000000 ) ) ;
#24790 = CYLINDRICAL_SURFACE ( 'NONE', #33272, 125.0000000000000000 ) ;
#24791 = EDGE_CURVE ( 'NONE', #50432, #5269, #27146, .T. ) ;
#24792 = AXIS2_PLACEMENT_3D ( 'NONE', #38607, #50457, #2084 ) ;
#24793 = EDGE_LOOP ( 'NONE', ( #19982, #18700, #43178, #27627 ) ) ;
#24794 = ORIENTED_EDGE ( 'NONE', *, *, #35670, .T. ) ;
#24795 = CARTESIAN_POINT ( 'NONE',  ( -48.47912675150885065, -213.5000000000000000, 6.938893903907228378E-15 ) ) ;
#24796 = LINE ( 'NONE', #42113, #45201 ) ;
#24797 = ORIENTED_EDGE ( 'NONE', *, *, #19915, .T. ) ;
#24798 = DIRECTION ( 'NONE',  ( -0.000000000000000000, 1.000000000000000000, -0.000000000000000000 ) ) ;
#24799 = CARTESIAN_POINT ( 'NONE',  ( -121.5885020763900997, -177.1207230881787780, -101.3904297239421055 ) ) ;
#24800 = ORIENTED_EDGE ( 'NONE', *, *, #33374, .F. ) ;
#24801 = FACE_BOUND ( 'NONE', #36479, .T. ) ;
#24802 = DIRECTION ( 'NONE',  ( -0.000000000000000000, 1.000000000000000000, -0.000000000000000000 ) ) ;
#24803 = ORIENTED_EDGE ( 'NONE', *, *, #45266, .T. ) ;
#24804 = LINE ( 'NONE', #41342, #3935 ) ;
#24805 = ORIENTED_EDGE ( 'NONE', *, *, #7609, .T. ) ;
#24806 = CARTESIAN_POINT ( 'NONE',  ( -305.0000000000000568, -91.61526299123897843, -50.82679948493848343 ) ) ;
#24807 = AXIS2_PLACEMENT_3D ( 'NONE', #17905, #12906, #28929 ) ;
#24808 = PLANE ( 'NONE',  #22720 ) ;
#24809 = EDGE_LOOP ( 'NONE', ( #26848, #36079, #11454, #43298 ) ) ;
#24810 = AXIS2_PLACEMENT_3D ( 'NONE', #50281, #34736, #7150 ) ;
#24811 = VECTOR ( 'NONE', #43102, 1000.000000000000000 ) ;
#24812 = CARTESIAN_POINT ( 'NONE',  ( -330.4913330509368166, -178.4886558749180949, 21.38919645685269444 ) ) ;
#24813 = DIRECTION ( 'NONE',  ( 0.000000000000000000, -0.000000000000000000, -1.000000000000000000 ) ) ;
#24814 = FACE_OUTER_BOUND ( 'NONE', #22741, .T. ) ;
#24815 = CARTESIAN_POINT ( 'NONE',  ( -49.46816693883101834, -175.3837268820161057, 0.1476465640024780257 ) ) ;
#24816 = VERTEX_POINT ( 'NONE', #42675 ) ;
#24817 = CARTESIAN_POINT ( 'NONE',  ( 26.52087324849106054, -198.5000000000000000, -60.00000000000003553 ) ) ;
#24818 = VERTEX_POINT ( 'NONE', #19520 ) ;
#24819 = ORIENTED_EDGE ( 'NONE', *, *, #31266, .T. ) ;
#24820 = DIRECTION ( 'NONE',  ( -0.000000000000000000, -1.000000000000000000, 0.000000000000000000 ) ) ;
#24822 = ORIENTED_EDGE ( 'NONE', *, *, #35175, .F. ) ;
#24821 = DIRECTION ( 'NONE',  ( -0.000000000000000000, -1.000000000000000000, 0.000000000000000000 ) ) ;
#24823 = VECTOR ( 'NONE', #39733, 1000.000000000000000 ) ;
#24824 = VERTEX_POINT ( 'NONE', #39247 ) ;
#24825 = CARTESIAN_POINT ( 'NONE',  ( -127.6327502296859535, -177.1207230881787780, -95.45105364470086329 ) ) ;
#24826 = ADVANCED_FACE ( 'NONE', ( #51342 ), #11372, .T. ) ;
#24827 = CIRCLE ( 'NONE', #4680, 125.0000000000000000 ) ;
#24828 = AXIS2_PLACEMENT_3D ( 'NONE', #51367, #11392, #27429 ) ;
#24829 = DIRECTION ( 'NONE',  ( 0.000000000000000000, -0.000000000000000000, 1.000000000000000000 ) ) ;
#24830 = ORIENTED_EDGE ( 'NONE', *, *, #51726, .T. ) ;
#24831 = DIRECTION ( 'NONE',  ( 0.000000000000000000, -0.000000000000000000, -1.000000000000000000 ) ) ;
#24832 = ORIENTED_EDGE ( 'NONE', *, *, #40338, .T. ) ;
#24833 = LINE ( 'NONE', #40852, #16623 ) ;
#24834 = CARTESIAN_POINT ( 'NONE',  ( -104.8182102393454045, -193.5000000000000000, 111.5836353223472912 ) ) ;
#24835 = LINE ( 'NONE', #16445, #23559 ) ;
#24836 = CARTESIAN_POINT ( 'NONE',  ( -336.3521761649654422, -75.87119766449505676, -34.85916744524372746 ) ) ;
#24837 = VERTEX_POINT ( 'NONE', #15595 ) ;
#24838 = ORIENTED_EDGE ( 'NONE', *, *, #48029, .F. ) ;
#24839 = ORIENTED_EDGE ( 'NONE', *, *, #12198, .T. ) ;
#24840 = DIRECTION ( 'NONE',  ( 1.000000000000000000, 0.000000000000000000, 0.000000000000000000 ) ) ;
#24841 = CARTESIAN_POINT ( 'NONE',  ( -1.771278280434267272, -193.5000000000000000, -115.9455772817710226 ) ) ;
#24842 = VECTOR ( 'NONE', #44919, 1000.000000000000114 ) ;
#24843 = VECTOR ( 'NONE', #29387, 1000.000000000000000 ) ;
#24844 = EDGE_CURVE ( 'NONE', #37031, #2833, #43703, .T. ) ;
#24845 = CARTESIAN_POINT ( 'NONE',  ( -48.88225018079683082, -183.6283474603465606, 0.9151456172430223468 ) ) ;
#24846 = VECTOR ( 'NONE', #22343, 1000.000000000000000 ) ;
#24847 = CARTESIAN_POINT ( 'NONE',  ( -48.24424070572787571, -177.1207230881787780, 0.9720229140804191870 ) ) ;
#24848 = CARTESIAN_POINT ( 'NONE',  ( -336.3521761649654422, -174.5186198893880771, 29.74944317415823392 ) ) ;
#24849 = EDGE_LOOP ( 'NONE', ( #10088, #38298, #39526, #31533 ) ) ;
#24850 = CIRCLE ( 'NONE', #36584, 125.0000000000000000 ) ;
#24851 = ORIENTED_EDGE ( 'NONE', *, *, #10521, .F. ) ;
#24853 = VERTEX_POINT ( 'NONE', #50566 ) ;
#24852 = CARTESIAN_POINT ( 'NONE',  ( -305.0000000000000568, -64.31210272782786319, -9.838334030657643225 ) ) ;
#24854 = ORIENTED_EDGE ( 'NONE', *, *, #24086, .F. ) ;
#24855 = DIRECTION ( 'NONE',  ( 0.000000000000000000, 0.9350162426854146114, -0.3546048870425363986 ) ) ;
#24856 = AXIS2_PLACEMENT_3D ( 'NONE', #40232, #11616, #23691 ) ;
#24857 = DIRECTION ( 'NONE',  ( 0.000000000000000000, -0.000000000000000000, 1.000000000000000000 ) ) ;
#24858 = AXIS2_PLACEMENT_3D ( 'NONE', #20886, #9052, #37411 ) ;
#24859 = AXIS2_PLACEMENT_3D ( 'NONE', #1613, #33656, #37856 ) ;
#24860 = CARTESIAN_POINT ( 'NONE',  ( 42.61556600127744332, 28.88712326890129845, -46.12484337987545757 ) ) ;
#24861 = DIRECTION ( 'NONE',  ( 0.3758275821142292861, 0.000000000000000000, 0.9266896074318371479 ) ) ;
#24862 = VERTEX_POINT ( 'NONE', #14568 ) ;
#24863 = LINE ( 'NONE', #36695, #13260 ) ;
#24864 = VECTOR ( 'NONE', #29442, 1000.000000000000000 ) ;
#24865 = ORIENTED_EDGE ( 'NONE', *, *, #19258, .T. ) ;
#24866 = AXIS2_PLACEMENT_3D ( 'NONE', #31140, #35340, #2765 ) ;
#24867 = ORIENTED_EDGE ( 'NONE', *, *, #8849, .F. ) ;
#24868 = LINE ( 'NONE', #25392, #3575 ) ;
#24869 = DIRECTION ( 'NONE',  ( 0.000000000000000000, 1.000000000000000000, 0.000000000000000000 ) ) ;
#24870 = LINE ( 'NONE', #15964, #39120 ) ;
#24871 = LINE ( 'NONE', #42386, #51635 ) ;
#24872 = ADVANCED_FACE ( 'NONE', ( #30571 ), #41241, .F. ) ;
#24873 = PLANE ( 'NONE',  #13914 ) ;
#24874 = CARTESIAN_POINT ( 'NONE',  ( -129.4514457347087273, -193.5000000000000000, 95.22858582633115532 ) ) ;
#24875 = DIRECTION ( 'NONE',  ( 0.4566292373937018145, 0.000000000000000000, 0.8896570909947529859 ) ) ;
#24876 = ORIENTED_EDGE ( 'NONE', *, *, #28724, .F. ) ;
#24877 = CARTESIAN_POINT ( 'NONE',  ( -48.47912675150885065, -177.1207230881787780, -0.9999999999999931166 ) ) ;
#24878 = DIRECTION ( 'NONE',  ( 0.000000000000000000, 0.000000000000000000, -1.000000000000000000 ) ) ;
#24879 = EDGE_CURVE ( 'NONE', #23075, #7125, #44684, .T. ) ;
#24880 = CARTESIAN_POINT ( 'NONE',  ( -330.4913330509368166, -123.5000000000000284, 0.000000000000000000 ) ) ;
#24881 = FACE_BOUND ( 'NONE', #6439, .T. ) ;
#24882 = ORIENTED_EDGE ( 'NONE', *, *, #25578, .F. ) ;
#24883 = AXIS2_PLACEMENT_3D ( 'NONE', #29587, #25399, #956 ) ;
#24884 = AXIS2_PLACEMENT_3D ( 'NONE', #19631, #34623, #43289 ) ;
#24885 = CARTESIAN_POINT ( 'NONE',  ( -47.74129347246713451, -193.5000000000000000, 0.6749830015182212151 ) ) ;
#24886 = ORIENTED_EDGE ( 'NONE', *, *, #9165, .F. ) ;
#24887 = VECTOR ( 'NONE', #39146, 1000.000000000000000 ) ;
#24888 = LINE ( 'NONE', #44352, #37876 ) ;
#24889 = VERTEX_POINT ( 'NONE', #33381 ) ;
#24890 = LINE ( 'NONE', #13050, #48103 ) ;
#24891 = EDGE_CURVE ( 'NONE', #44141, #49533, #20619, .T. ) ;
#24892 = EDGE_LOOP ( 'NONE', ( #41843, #3669 ) ) ;
#24893 = EDGE_CURVE ( 'NONE', #29042, #22971, #41500, .T. ) ;
#24894 = CARTESIAN_POINT ( 'NONE',  ( -55.71438232577009586, -175.3837268820161057, -124.7904286264580804 ) ) ;
#24895 = AXIS2_PLACEMENT_3D ( 'NONE', #39767, #11146, #27172 ) ;
#24896 = EDGE_CURVE ( 'NONE', #30672, #30972, #42415, .T. ) ;
#24897 = FACE_BOUND ( 'NONE', #45243, .T. ) ;
#24898 = AXIS2_PLACEMENT_3D ( 'NONE', #14728, #35202, #10264 ) ;
#24900 = VERTEX_POINT ( 'NONE', #36521 ) ;
#24899 = CARTESIAN_POINT ( 'NONE',  ( 29.27398957514434130, -193.5000000000000000, -97.87467957287998388 ) ) ;
#24901 = VECTOR ( 'NONE', #28357, 1000.000000000000114 ) ;
#24902 = ADVANCED_BREP_SHAPE_REPRESENTATION ( '', ( #18528, #31742 ), #18326 ) ;
#24903 = AXIS2_PLACEMENT_3D ( 'NONE', #40041, #11926, #38820 ) ;
#24904 = AXIS2_PLACEMENT_3D ( 'NONE', #35109, #51940, #11711 ) ;
#24905 = PLANE ( 'NONE',  #32754 ) ;
#24906 = VERTEX_POINT ( 'NONE', #28634 ) ;
#24907 = ORIENTED_EDGE ( 'NONE', *, *, #38092, .T. ) ;
#24908 = ORIENTED_EDGE ( 'NONE', *, *, #2799, .T. ) ;
#24909 = VECTOR ( 'NONE', #7724, 1000.000000000000000 ) ;
#24910 = LINE ( 'NONE', #4166, #51961 ) ;
#24911 = DIRECTION ( 'NONE',  ( -0.000000000000000000, 1.000000000000000000, -0.000000000000000000 ) ) ;
#24912 = EDGE_LOOP ( 'NONE', ( #41561, #8322, #49483, #15094 ) ) ;
#24913 = EDGE_CURVE ( 'NONE', #43506, #49860, #37577, .T. ) ;
#24914 = DIRECTION ( 'NONE',  ( -0.000000000000000000, -1.000000000000000000, -0.000000000000000000 ) ) ;
#24915 = LINE ( 'NONE', #32792, #32212 ) ;
#24916 = CARTESIAN_POINT ( 'NONE',  ( -172.2289551866394106, -193.5000000000000000, -17.63462396184707970 ) ) ;
#24917 = PLANE ( 'NONE',  #51699 ) ;
#24918 = ORIENTED_EDGE ( 'NONE', *, *, #31716, .F. ) ;
#24921 = ORIENTED_EDGE ( 'NONE', *, *, #29821, .F. ) ;
#24920 = CARTESIAN_POINT ( 'NONE',  ( 73.66680038934278230, -175.3837268820161057, -26.55884942729568721 ) ) ;
#24919 = CARTESIAN_POINT ( 'NONE',  ( 48.66843973345087448, 30.00000000000000355, -40.95752564483601788 ) ) ;
#24922 = AXIS2_PLACEMENT_3D ( 'NONE', #15385, #27188, #39015 ) ;
#24923 = ORIENTED_EDGE ( 'NONE', *, *, #39358, .F. ) ;
#24924 = VECTOR ( 'NONE', #24753, 1000.000000000000000 ) ;
#24925 = CARTESIAN_POINT ( 'NONE',  ( -330.4913330509368166, -90.39567187580801999, 48.84008046109089918 ) ) ;
#24926 = ORIENTED_EDGE ( 'NONE', *, *, #22631, .T. ) ;
#24927 = FACE_OUTER_BOUND ( 'NONE', #6837, .T. ) ;
#24928 = ORIENTED_EDGE ( 'NONE', *, *, #19407, .F. ) ;
#24929 = VECTOR ( 'NONE', #34514, 1000.000000000000000 ) ;
#24930 = CARTESIAN_POINT ( 'NONE',  ( -330.4913330509368166, -180.9052250602807703, 13.63415328425337236 ) ) ;
#24931 = DIRECTION ( 'NONE',  ( 0.000000000000000000, 0.000000000000000000, -1.000000000000000000 ) ) ;
#24932 = VERTEX_POINT ( 'NONE', #32590 ) ;
#24933 = DIRECTION ( 'NONE',  ( 0.000000000000000000, 0.000000000000000000, -1.000000000000000000 ) ) ;
#24934 = ORIENTED_EDGE ( 'NONE', *, *, #15985, .T. ) ;
#24935 = ORIENTED_EDGE ( 'NONE', *, *, #46256, .T. ) ;
#24936 = DIRECTION ( 'NONE',  ( -0.3202698538628487301, 0.000000000000000000, 0.9473263538541877304 ) ) ;
#24937 = AXIS2_PLACEMENT_3D ( 'NONE', #1966, #41385, #36935 ) ;
#24938 = CYLINDRICAL_SURFACE ( 'NONE', #12140, 125.0000000000000000 ) ;
#24939 = AXIS2_PLACEMENT_3D ( 'NONE', #50774, #2670, #19723 ) ;
#24940 = DIRECTION ( 'NONE',  ( 0.000000000000000000, -0.7485107481710934207, 0.6631226582408039638 ) ) ;
#24941 = LINE ( 'NONE', #28862, #26667 ) ;
#24942 = VERTEX_POINT ( 'NONE', #17361 ) ;
#24943 = VECTOR ( 'NONE', #13607, 1000.000000000000000 ) ;
#24944 = VECTOR ( 'NONE', #46601, 1000.000000000000000 ) ;
#24945 = DIRECTION ( 'NONE',  ( 0.000000000000000000, 0.000000000000000000, 1.000000000000000000 ) ) ;
#24946 = ADVANCED_FACE ( 'NONE', ( #24977 ), #21285, .F. ) ;
#24947 = EDGE_CURVE ( 'NONE', #41267, #17894, #16839, .T. ) ;
#24948 = PRODUCT_CONTEXT ( 'NONE', #8866, 'mechanical' ) ;
#24949 = DIRECTION ( 'NONE',  ( 0.8455960035018199594, 0.000000000000000000, 0.5338233779648003940 ) ) ;
#24950 = VECTOR ( 'NONE', #28660, 1000.000000000000000 ) ;
#24951 = DIRECTION ( 'NONE',  ( -0.000000000000000000, 1.000000000000000000, -0.000000000000000000 ) ) ;
#24952 = CARTESIAN_POINT ( 'NONE',  ( -339.1964088526558498, -175.9742670995615015, -26.97593913775538965 ) ) ;
#24953 = VECTOR ( 'NONE', #26020, 1000.000000000000000 ) ;
#24954 = LINE ( 'NONE', #237, #6164 ) ;
#24955 = VERTEX_POINT ( 'NONE', #20768 ) ;
#24956 = LINE ( 'NONE', #16822, #39087 ) ;
#24957 = CARTESIAN_POINT ( 'NONE',  ( 14.94072793302542124, -175.3837268820161057, 107.7168604805791574 ) ) ;
#24958 = LINE ( 'NONE', #9701, #48930 ) ;
#24959 = VERTEX_POINT ( 'NONE', #37308 ) ;
#24960 = ORIENTED_EDGE ( 'NONE', *, *, #6510, .F. ) ;
#24961 = ADVANCED_FACE ( 'NONE', ( #28893 ), #48640, .T. ) ;
#24962 = EDGE_LOOP ( 'NONE', ( #36264, #18441, #32800, #3804 ) ) ;
#24963 = EDGE_CURVE ( 'NONE', #50756, #15492, #13655, .T. ) ;
#24964 = AXIS2_PLACEMENT_3D ( 'NONE', #10126, #20929, #41652 ) ;
#24965 = FACE_OUTER_BOUND ( 'NONE', #44405, .T. ) ;
#24966 = CIRCLE ( 'NONE', #24107, 25.00456841203573077 ) ;
#24967 = EDGE_CURVE ( 'NONE', #8712, #2850, #29675, .T. ) ;
#24968 = DIRECTION ( 'NONE',  ( 0.000000000000000000, -0.000000000000000000, -1.000000000000000000 ) ) ;
#24969 = DIRECTION ( 'NONE',  ( 1.000000000000000000, -0.000000000000000000, -0.000000000000000000 ) ) ;
#24970 = CARTESIAN_POINT ( 'NONE',  ( -92.16375985330356002, -175.3837268820161057, 117.1181148702521710 ) ) ;
#24971 = VECTOR ( 'NONE', #7520, 1000.000000000000000 ) ;
#24972 = ADVANCED_FACE ( 'NONE', ( #8939 ), #49424, .F. ) ;
#24973 = ORIENTED_EDGE ( 'NONE', *, *, #45415, .F. ) ;
#24974 = CARTESIAN_POINT ( 'NONE',  ( -16.00000000000000711, 65.00000000000000000, 0.000000000000000000 ) ) ;
#24975 = PLANE ( 'NONE',  #36085 ) ;
#24976 = VERTEX_POINT ( 'NONE', #13402 ) ;
#24977 = FACE_OUTER_BOUND ( 'NONE', #48733, .T. ) ;
#24978 = ORIENTED_EDGE ( 'NONE', *, *, #29995, .F. ) ;
#24979 = CARTESIAN_POINT ( 'NONE',  ( 49.88781503343063406, -177.1207230881787780, -75.49882471933871386 ) ) ;
#24980 = AXIS2_PLACEMENT_3D ( 'NONE', #23739, #19792, #23997 ) ;
#24981 = VECTOR ( 'NONE', #2087, 1000.000000000000000 ) ;
#24982 = VERTEX_POINT ( 'NONE', #4740 ) ;
#24983 = CARTESIAN_POINT ( 'NONE',  ( -171.9740864388383557, -193.5000000000000000, -11.18012358327899314 ) ) ;
#24984 = AXIS2_PLACEMENT_3D ( 'NONE', #30658, #37778, #30933 ) ;
#24985 = AXIS2_PLACEMENT_3D ( 'NONE', #6324, #49955, #2108 ) ;
#24986 = AXIS2_PLACEMENT_3D ( 'NONE', #3972, #40469, #43653 ) ;
#24987 = DIRECTION ( 'NONE',  ( -0.000000000000000000, -1.000000000000000000, 0.000000000000000000 ) ) ;
#24988 = DIRECTION ( 'NONE',  ( 0.000000000000000000, 0.000000000000000000, 1.000000000000000000 ) ) ;
#24991 = VERTEX_POINT ( 'NONE', #36799 ) ;
#24990 = CARTESIAN_POINT ( 'NONE',  ( -332.3517673607765914, -178.0871407151310279, 22.44790492310219676 ) ) ;
#24989 = DIRECTION ( 'NONE',  ( 0.000000000000000000, -1.000000000000000000, 0.000000000000000000 ) ) ;
#24992 = CARTESIAN_POINT ( 'NONE',  ( -336.3521761649654422, -68.91285928486892942, -22.44790492310182017 ) ) ;
#24993 = ORIENTED_EDGE ( 'NONE', *, *, #36269, .T. ) ;
#24994 = DIRECTION ( 'NONE',  ( 0.000000000000000000, 0.000000000000000000, 1.000000000000000000 ) ) ;
#24995 = DIRECTION ( 'NONE',  ( -0.000000000000000000, 1.000000000000000000, -0.000000000000000000 ) ) ;
#24996 = ORIENTED_EDGE ( 'NONE', *, *, #22999, .T. ) ;
#24997 = CARTESIAN_POINT ( 'NONE',  ( -339.1964088526558498, -66.09477493971894546, 13.63415328425207917 ) ) ;
#24999 = DIRECTION ( 'NONE',  ( -0.000000000000000000, 1.000000000000000000, -0.000000000000000000 ) ) ;
#24998 = LINE ( 'NONE', #45743, #24953 ) ;
#25000 = ORIENTED_EDGE ( 'NONE', *, *, #43627, .F. ) ;
#25001 = EDGE_CURVE ( 'NONE', #43983, #30132, #25228, .T. ) ;
#25002 = CARTESIAN_POINT ( 'NONE',  ( -330.4913330509368166, -144.3080463282022663, -56.27632902032068785 ) ) ;
#25003 = AXIS2_PLACEMENT_3D ( 'NONE', #22730, #15367, #35074 ) ;
#25004 = DIRECTION ( 'NONE',  ( 0.000000000000000000, 0.000000000000000000, -1.000000000000000000 ) ) ;
#25005 = VECTOR ( 'NONE', #757, 1000.000000000000000 ) ;
#25006 = CARTESIAN_POINT ( 'NONE',  ( -106.2948367055609964, -189.7472609257535510, -110.8257356506552327 ) ) ;
#25007 = ORIENTED_EDGE ( 'NONE', *, *, #20220, .F. ) ;
#25008 = DIRECTION ( 'NONE',  ( -1.000000000000000000, 0.000000000000000000, 0.000000000000000000 ) ) ;
#25009 = DIRECTION ( 'NONE',  ( -0.000000000000000000, 1.000000000000000000, -0.000000000000000000 ) ) ;
#25010 = AXIS2_PLACEMENT_3D ( 'NONE', #30574, #19027, #15340 ) ;
#25011 = CARTESIAN_POINT ( 'NONE',  ( -336.3521761649654422, -64.50000000000000000, -2.632288850093980503 ) ) ;
#25012 = EDGE_CURVE ( 'NONE', #45883, #37758, #8673, .T. ) ;
#25013 = EDGE_CURVE ( 'NONE', #35455, #12928, #49146, .T. ) ;
#25014 = EDGE_LOOP ( 'NONE', ( #37263, #19521, #19966, #3568 ) ) ;
#25015 = EDGE_CURVE ( 'NONE', #24991, #3996, #25482, .T. ) ;
#25016 = DIRECTION ( 'NONE',  ( -0.000000000000000000, 0.6631226582408016323, 0.7485107481710953081 ) ) ;
#25017 = EDGE_CURVE ( 'NONE', #33038, #23726, #46247, .T. ) ;
#25018 = DIRECTION ( 'NONE',  ( 0.000000000000000000, -1.000000000000000000, 0.000000000000000000 ) ) ;
#25019 = ORIENTED_EDGE ( 'NONE', *, *, #23676, .T. ) ;
#25020 = VECTOR ( 'NONE', #5134, 1000.000000000000000 ) ;
#25021 = CARTESIAN_POINT ( 'NONE',  ( -336.3521761649654422, -120.8677111499054320, 59.00000000000000000 ) ) ;
#25022 = EDGE_CURVE ( 'NONE', #50532, #37883, #1299, .T. ) ;
#25023 = PLANE ( 'NONE',  #24438 ) ;
#25024 = LINE ( 'NONE', #12913, #15157 ) ;
#25025 = DIRECTION ( 'NONE',  ( 0.000000000000000000, 1.000000000000000000, 0.000000000000000000 ) ) ;
#25026 = FACE_OUTER_BOUND ( 'NONE', #888, .T. ) ;
#25027 = ADVANCED_FACE ( 'NONE', ( #6561 ), #14440, .F. ) ;
#25028 = EDGE_CURVE ( 'NONE', #33448, #32690, #22056, .T. ) ;
#25030 = VECTOR ( 'NONE', #10239, 1000.000000000000000 ) ;
#25029 = CARTESIAN_POINT ( 'NONE',  ( 1.734723475976807094E-15, 20.00000000000000000, 46.00000000000000711 ) ) ;
#25031 = ADVANCED_FACE ( 'NONE', ( #34405 ), #42801, .T. ) ;
#25032 = DIRECTION ( 'NONE',  ( 0.000000000000000000, 0.000000000000000000, 1.000000000000000000 ) ) ;
#25033 = DIRECTION ( 'NONE',  ( 0.000000000000000000, 0.000000000000000000, 1.000000000000000000 ) ) ;
#25035 = EDGE_LOOP ( 'NONE', ( #39969, #37523, #21849, #35544 ) ) ;
#25034 = PLANE ( 'NONE',  #30370 ) ;
#25036 = EDGE_CURVE ( 'NONE', #47279, #47521, #38598, .T. ) ;
#25037 = ORIENTED_EDGE ( 'NONE', *, *, #35090, .T. ) ;
#25038 = CARTESIAN_POINT ( 'NONE',  ( -339.1964088526558498, -78.25935320507949200, -39.41172259083896279 ) ) ;
#25039 = ADVANCED_FACE ( 'NONE', ( #1822 ), #30206, .T. ) ;
#25040 = CARTESIAN_POINT ( 'NONE',  ( 73.32083127613157103, -177.1207230881787780, 28.10285082451656535 ) ) ;
#25041 = EDGE_LOOP ( 'NONE', ( #39071, #2951, #47790, #7697 ) ) ;
#25042 = AXIS2_PLACEMENT_3D ( 'NONE', #32490, #20142, #8563 ) ;
#25043 = ORIENTED_EDGE ( 'NONE', *, *, #46719, .F. ) ;
#25044 = VECTOR ( 'NONE', #44434, 1000.000000000000000 ) ;
#25045 = VERTEX_POINT ( 'NONE', #30450 ) ;
#25046 = CARTESIAN_POINT ( 'NONE',  ( -330.4913330509368166, -74.65991953890832633, 33.10432812419081472 ) ) ;
#25047 = VECTOR ( 'NONE', #50512, 1000.000000000000114 ) ;
#25048 = CARTESIAN_POINT ( 'NONE',  ( 47.04848625005566731, -193.5000000000000000, 80.61932246194658092 ) ) ;
#25049 = DIRECTION ( 'NONE',  ( 0.000000000000000000, 0.000000000000000000, -1.000000000000000000 ) ) ;
#25050 = ORIENTED_EDGE ( 'NONE', *, *, #35315, .F. ) ;
#25051 = ORIENTED_EDGE ( 'NONE', *, *, #42064, .F. ) ;
#25052 = ADVANCED_FACE ( 'NONE', ( #42023 ), #46758, .T. ) ;
#25053 = DIRECTION ( 'NONE',  ( 0.000000000000000000, -1.000000000000000000, 0.000000000000000000 ) ) ;
#25054 = AXIS2_PLACEMENT_3D ( 'NONE', #45469, #17621, #41502 ) ;
#25056 = ORIENTED_EDGE ( 'NONE', *, *, #28313, .F. ) ;
#25055 = CARTESIAN_POINT ( 'NONE',  ( 59.80284513346456521, -193.5000000000000000, 62.45009659481583952 ) ) ;
#25057 = DIRECTION ( 'NONE',  ( 0.000000000000000000, 0.000000000000000000, 1.000000000000000000 ) ) ;
#25058 = ORIENTED_EDGE ( 'NONE', *, *, #12540, .F. ) ;
#25059 = LINE ( 'NONE', #41065, #33921 ) ;
#25060 = VERTEX_POINT ( 'NONE', #38075 ) ;
#25061 = CARTESIAN_POINT ( 'NONE',  ( -171.5708553757489767, -177.1207230881787780, 14.98512977653257039 ) ) ;
#25062 = CARTESIAN_POINT ( 'NONE',  ( -168.1386673294336163, -193.5000000000000000, 32.52067927015838933 ) ) ;
#25063 = DIRECTION ( 'NONE',  ( -0.7378332790417189146, 0.000000000000000000, -0.6749830015182196608 ) ) ;
#25064 = VECTOR ( 'NONE', #36757, 1000.000000000000000 ) ;
#25065 = VERTEX_POINT ( 'NONE', #21810 ) ;
#25066 = ORIENTED_EDGE ( 'NONE', *, *, #47130, .T. ) ;
#25067 = LINE ( 'NONE', #49512, #6361 ) ;
#25068 = CARTESIAN_POINT ( 'NONE',  ( 2.066935079424590871, -189.7472609257535510, -114.3245189510257660 ) ) ;
#25069 = ORIENTED_EDGE ( 'NONE', *, *, #43111, .T. ) ;
#25070 = DIRECTION ( 'NONE',  ( 0.000000000000000000, -1.000000000000000000, 0.000000000000000000 ) ) ;
#25071 = DIRECTION ( 'NONE',  ( 0.1768902751225802927, 0.000000000000000000, -0.9842305779475953864 ) ) ;
#25072 = ADVANCED_FACE ( 'NONE', ( #10478 ), #2074, .F. ) ;
#25073 = ADVANCED_FACE ( 'NONE', ( #42275 ), #26507, .F. ) ;
#25074 = EDGE_LOOP ( 'NONE', ( #5024, #28207, #1233, #30931 ) ) ;
#25075 = DIRECTION ( 'NONE',  ( 1.000000000000000000, 0.000000000000000000, 0.000000000000000000 ) ) ;
#25076 = DIRECTION ( 'NONE',  ( -0.000000000000000000, 1.000000000000000000, -0.000000000000000000 ) ) ;
#25077 = EDGE_CURVE ( 'NONE', #18623, #43059, #18386, .T. ) ;
#25078 = EDGE_CURVE ( 'NONE', #13689, #28174, #16433, .T. ) ;
#25079 = ORIENTED_EDGE ( 'NONE', *, *, #43283, .T. ) ;
#25080 = CARTESIAN_POINT ( 'NONE',  ( -123.4791267515088435, -198.5000000000000000, 60.00000000000001421 ) ) ;
#25081 = ORIENTED_EDGE ( 'NONE', *, *, #19149, .T. ) ;
#25082 = VECTOR ( 'NONE', #50863, 1000.000000000000000 ) ;
#25083 = CARTESIAN_POINT ( 'NONE',  ( -102.9981419485577590, -177.1207230881787780, -111.3726929437936377 ) ) ;
#25084 = VECTOR ( 'NONE', #32794, 1000.000000000000000 ) ;
#25085 = DIRECTION ( 'NONE',  ( 0.000000000000000000, 0.8229838658936536877, -0.5680647467311596976 ) ) ;
#25086 = ORIENTED_EDGE ( 'NONE', *, *, #35871, .F. ) ;
#25087 = AXIS2_PLACEMENT_3D ( 'NONE', #8100, #43829, #48306 ) ;
#25088 = DIRECTION ( 'NONE',  ( -0.000000000000000000, -0.9350162426854121689, 0.3546048870425426158 ) ) ;
#25089 = CARTESIAN_POINT ( 'NONE',  ( -48.47912675150885065, -177.1207230881787780, 6.938893903907228378E-15 ) ) ;
#25090 = CARTESIAN_POINT ( 'NONE',  ( -49.35486169370449971, -193.5000000000000000, 0.4827922027307437469 ) ) ;
#25091 = DIRECTION ( 'NONE',  ( -0.9960498426152165630, 0.000000000000000000, -0.08879589532293852283 ) ) ;
#25092 = VERTEX_POINT ( 'NONE', #50696 ) ;
#25093 = DIRECTION ( 'NONE',  ( 0.000000000000000000, -0.000000000000000000, -1.000000000000000000 ) ) ;
#25094 = ORIENTED_EDGE ( 'NONE', *, *, #18657, .F. ) ;
#25095 = EDGE_LOOP ( 'NONE', ( #24359, #6540, #41501, #51012 ) ) ;
#25096 = CIRCLE ( 'NONE', #26726, 125.0000000000000000 ) ;
#25097 = EDGE_CURVE ( 'NONE', #42695, #45794, #25746, .T. ) ;
#25098 = LINE ( 'NONE', #20896, #11004 ) ;
#25100 = EDGE_LOOP ( 'NONE', ( #7671, #1480, #24210, #51475 ) ) ;
#25099 = CARTESIAN_POINT ( 'NONE',  ( 60.00000000000000000, -63.50000000000000000, 60.00000000000000711 ) ) ;
#25101 = ORIENTED_EDGE ( 'NONE', *, *, #36441, .F. ) ;
#25102 = DIRECTION ( 'NONE',  ( 0.000000000000000000, 1.000000000000000000, 0.000000000000000000 ) ) ;
#25103 = EDGE_CURVE ( 'NONE', #45420, #50591, #49054, .T. ) ;
#25104 = VECTOR ( 'NONE', #35133, 1000.000000000000000 ) ;
#25105 = CARTESIAN_POINT ( 'NONE',  ( -172.1341525481709880, -193.5000000000000000, 18.28755301364337527 ) ) ;
#25106 = CARTESIAN_POINT ( 'NONE',  ( -180.0000000000000568, -155.0173647354142759, -14.76740078976489201 ) ) ;
#25107 = ORIENTED_EDGE ( 'NONE', *, *, #36426, .T. ) ;
#25108 = FACE_OUTER_BOUND ( 'NONE', #31243, .T. ) ;
#25109 = EDGE_LOOP ( 'NONE', ( #6560, #30328, #16566, #48602 ) ) ;
#25110 = DIRECTION ( 'NONE',  ( 1.000000000000000000, 0.000000000000000000, -0.000000000000000000 ) ) ;
#25111 = CARTESIAN_POINT ( 'NONE',  ( -158.6498865914718408, -177.1207230881787780, 56.90809649257572289 ) ) ;
#25112 = DIRECTION ( 'NONE',  ( -0.000000000000000000, 0.000000000000000000, 1.000000000000000000 ) ) ;
#25113 = CARTESIAN_POINT ( 'NONE',  ( -330.4913330509368166, -123.5000000000000284, 0.000000000000000000 ) ) ;
#25114 = EDGE_LOOP ( 'NONE', ( #23876, #48697 ) ) ;
#25115 = ORIENTED_EDGE ( 'NONE', *, *, #1594, .F. ) ;
#25116 = VERTEX_POINT ( 'NONE', #20667 ) ;
#25117 = LINE ( 'NONE', #1176, #45918 ) ;
#25118 = DIRECTION ( 'NONE',  ( 0.9960498426152158968, 0.000000000000000000, 0.08879589532294571153 ) ) ;
#25119 = VECTOR ( 'NONE', #47271, 1000.000000000000000 ) ;
#25120 = CARTESIAN_POINT ( 'NONE',  ( -330.4913330509368166, -178.4886558749180949, 21.38919645685269444 ) ) ;
#25121 = FACE_BOUND ( 'NONE', #11349, .T. ) ;
#25122 = CARTESIAN_POINT ( 'NONE',  ( -58.17235712592530206, -193.5000000000000000, 123.6213615703899649 ) ) ;
#25123 = ORIENTED_EDGE ( 'NONE', *, *, #15077, .F. ) ;
#25124 = AXIS2_PLACEMENT_3D ( 'NONE', #11968, #28001, #40092 ) ;
#25125 = ORIENTED_EDGE ( 'NONE', *, *, #43507, .T. ) ;
#25127 = VERTEX_POINT ( 'NONE', #33277 ) ;
#25126 = CARTESIAN_POINT ( 'NONE',  ( -47.87232660569026166, -175.3837268820161057, 0.7948544414133635883 ) ) ;
#25128 = EDGE_LOOP ( 'NONE', ( #12344, #25219, #25810, #35481 ) ) ;
#25129 = CARTESIAN_POINT ( 'NONE',  ( -48.47912675150885065, -177.1207230881787780, 6.938893903907228378E-15 ) ) ;
#25130 = CARTESIAN_POINT ( 'NONE',  ( -339.1964088526558498, -123.5000000000000284, 0.000000000000000000 ) ) ;
#25131 = CARTESIAN_POINT ( 'NONE',  ( -213.8817838414232426, -213.5000000000000000, -10.00000000000000000 ) ) ;
#25132 = DIRECTION ( 'NONE',  ( -1.000000000000000000, 0.000000000000000000, 0.000000000000000000 ) ) ;
#25133 = EDGE_CURVE ( 'NONE', #29857, #27624, #6373, .T. ) ;
#25134 = CARTESIAN_POINT ( 'NONE',  ( -48.47912675150885065, -120.5000000000000284, 6.938893903907228378E-15 ) ) ;
#25135 = ORIENTED_EDGE ( 'NONE', *, *, #3906, .T. ) ;
#25136 = CARTESIAN_POINT ( 'NONE',  ( -137.9639882952644143, -177.1207230881787780, 87.27805883780241913 ) ) ;
#25137 = EDGE_LOOP ( 'NONE', ( #11434, #4021, #14140, #24101 ) ) ;
#25138 = AXIS2_PLACEMENT_3D ( 'NONE', #1615, #29710, #45754 ) ;
#25139 = ORIENTED_EDGE ( 'NONE', *, *, #47731, .F. ) ;
#25140 = DIRECTION ( 'NONE',  ( 1.000000000000000000, -0.000000000000000000, 0.000000000000000000 ) ) ;
#25141 = CARTESIAN_POINT ( 'NONE',  ( -47.92047998570520662, -189.7472609257535510, 0.8294056854502119824 ) ) ;
#25142 = DIRECTION ( 'NONE',  ( 0.000000000000000000, 6.938893903907229364E-16, 1.000000000000000000 ) ) ;
#25143 = CARTESIAN_POINT ( 'NONE',  ( -339.1964088526558498, -182.1300919119129560, -6.615309698014600670 ) ) ;
#25144 = LINE ( 'NONE', #41158, #50580 ) ;
#25145 = ORIENTED_EDGE ( 'NONE', *, *, #21819, .F. ) ;
#25146 = FACE_OUTER_BOUND ( 'NONE', #5303, .T. ) ;
#25147 = DIRECTION ( 'NONE',  ( -0.7575112421616191360, 0.000000000000000000, -0.6528221181905227155 ) ) ;
#25148 = DIRECTION ( 'NONE',  ( 1.000000000000000000, 0.000000000000000000, 0.000000000000000000 ) ) ;
#25150 = FACE_BOUND ( 'NONE', #40873, .T. ) ;
#25149 = PRODUCT_RELATED_PRODUCT_CATEGORY ( 'part', '', ( #14281 ) ) ;
#25151 = ORIENTED_EDGE ( 'NONE', *, *, #38474, .T. ) ;
#25152 = CIRCLE ( 'NONE', #2490, 125.0000000000000000 ) ;
#25153 = EDGE_CURVE ( 'NONE', #48128, #27213, #2158, .T. ) ;
#25154 = PLANE ( 'NONE',  #39869 ) ;
#25155 = VERTEX_POINT ( 'NONE', #28798 ) ;
#25156 = AXIS2_PLACEMENT_3D ( 'NONE', #2667, #42351, #47086 ) ;
#25157 = CARTESIAN_POINT ( 'NONE',  ( -180.0000000000000568, -123.5000000000000284, 15.24495751795539711 ) ) ;
#25158 = EDGE_LOOP ( 'NONE', ( #51667, #40336, #45138, #36337 ) ) ;
#25159 = CARTESIAN_POINT ( 'NONE',  ( -33.52607327456454556, -193.5000000000000000, -124.1024020384603119 ) ) ;
#25160 = EDGE_LOOP ( 'NONE', ( #40302, #37999, #47234, #39820 ) ) ;
#25161 = CARTESIAN_POINT ( 'NONE',  ( 74.60098876342244978, -183.6283474603465606, 21.82395850507348811 ) ) ;
#25162 = DIRECTION ( 'NONE',  ( 0.000000000000000000, -1.000000000000000000, 0.000000000000000000 ) ) ;
#25164 = ORIENTED_EDGE ( 'NONE', *, *, #6396, .F. ) ;
#25163 = CARTESIAN_POINT ( 'NONE',  ( -336.3521761649654422, -176.9651911376907094, -25.08789112700655721 ) ) ;
#25165 = EDGE_CURVE ( 'NONE', #26145, #38032, #41414, .T. ) ;
#25166 = CARTESIAN_POINT ( 'NONE',  ( -48.47912675150885065, -189.7472609257535510, 6.938893903907228378E-15 ) ) ;
#25167 = ORIENTED_EDGE ( 'NONE', *, *, #6449, .T. ) ;
#25168 = VERTEX_POINT ( 'NONE', #33789 ) ;
#25169 = AXIS2_PLACEMENT_3D ( 'NONE', #24326, #47985, #19355 ) ;
#25170 = ORIENTED_EDGE ( 'NONE', *, *, #7891, .T. ) ;
#25171 = CARTESIAN_POINT ( 'NONE',  ( -336.3521761649654422, -181.8730728925770563, 8.732051761644092025 ) ) ;
#25172 = CARTESIAN_POINT ( 'NONE',  ( -41.96187976958283627, -189.7472609257535510, -123.8286356280830205 ) ) ;
#25173 = ORIENTED_EDGE ( 'NONE', *, *, #6799, .T. ) ;
#25174 = PRESENTATION_STYLE_ASSIGNMENT (( #25427 ) ) ;
#25175 = CARTESIAN_POINT ( 'NONE',  ( -305.0000000000000568, -183.1207326066167127, -6.735595255826561711 ) ) ;
#25176 = LINE ( 'NONE', #13075, #42296 ) ;
#25177 = ORIENTED_EDGE ( 'NONE', *, *, #17338, .F. ) ;
#25178 = EDGE_CURVE ( 'NONE', #50890, #42195, #45639, .T. ) ;
#25179 = CYLINDRICAL_SURFACE ( 'NONE', #45234, 125.0000000000000000 ) ;
#25180 = LINE ( 'NONE', #32795, #17266 ) ;
#25181 = ORIENTED_EDGE ( 'NONE', *, *, #2231, .F. ) ;
#25184 = ORIENTED_EDGE ( 'NONE', *, *, #32273, .T. ) ;
#25183 = CARTESIAN_POINT ( 'NONE',  ( -48.47912675150885065, -183.6283474603465606, 6.938893903907228378E-15 ) ) ;
#25182 = DIRECTION ( 'NONE',  ( 0.9646355819083594074, 0.000000000000000000, -0.2635871660690647933 ) ) ;
#25185 = VERTEX_POINT ( 'NONE', #48799 ) ;
#25186 = VECTOR ( 'NONE', #44946, 1000.000000000000000 ) ;
#25187 = CARTESIAN_POINT ( 'NONE',  ( -339.1964088526558498, -84.75001853787809125, 44.49369547121489887 ) ) ;
#25188 = ORIENTED_EDGE ( 'NONE', *, *, #42692, .F. ) ;
#25189 = DIRECTION ( 'NONE',  ( 0.000000000000000000, 0.000000000000000000, -1.000000000000000000 ) ) ;
#25190 = VERTEX_POINT ( 'NONE', #49321 ) ;
#25191 = CARTESIAN_POINT ( 'NONE',  ( -332.3517673607765914, -65.12692710742291524, -8.732051761643681687 ) ) ;
#25192 = EDGE_CURVE ( 'NONE', #42748, #16426, #37477, .T. ) ;
#25193 = CARTESIAN_POINT ( 'NONE',  ( -48.47912675150885065, -177.1207230881787780, 6.938893903907228378E-15 ) ) ;
#25194 = ORIENTED_EDGE ( 'NONE', *, *, #36160, .F. ) ;
#25195 = DIRECTION ( 'NONE',  ( 0.000000000000000000, -1.000000000000000000, 0.000000000000000000 ) ) ;
#25196 = ORIENTED_EDGE ( 'NONE', *, *, #41256, .F. ) ;
#25197 = ORIENTED_EDGE ( 'NONE', *, *, #9938, .T. ) ;
#25198 = CARTESIAN_POINT ( 'NONE',  ( -33.98218805075477178, -175.3837268820161057, 123.1496609813405314 ) ) ;
#25199 = ADVANCED_FACE ( 'NONE', ( #33542 ), #13035, .T. ) ;
#25200 = PLANE ( 'NONE',  #45749 ) ;
#25201 = CARTESIAN_POINT ( 'NONE',  ( -36.15208382588832592, -193.5000000000000000, 123.3865623328509287 ) ) ;
#25202 = DIRECTION ( 'NONE',  ( -0.000000000000000000, -0.8229838658936596829, -0.5680647467311510379 ) ) ;
#25203 = VERTEX_POINT ( 'NONE', #36961 ) ;
#25204 = CARTESIAN_POINT ( 'NONE',  ( -305.0000000000000568, -145.2430625708868206, 55.92172413327848801 ) ) ;
#25205 = APPLICATION_PROTOCOL_DEFINITION ( 'draft international standard', 'automotive_design', 1998, #8183 ) ;
#25206 = DIRECTION ( 'NONE',  ( 0.000000000000000000, 0.000000000000000000, 1.000000000000000000 ) ) ;
#25207 = DIRECTION ( 'NONE',  ( -0.000000000000000000, 0.3546048870425331789, -0.9350162426854158326 ) ) ;
#25208 = CARTESIAN_POINT ( 'NONE',  ( -365.0000000000001137, -168.5000000000000284, 0.000000000000000000 ) ) ;
#25209 = CARTESIAN_POINT ( 'NONE',  ( -305.0000000000000568, -144.3080463282017263, 56.27632902032089390 ) ) ;
#25210 = CIRCLE ( 'NONE', #14292, 60.00000000000000000 ) ;
#25211 = VECTOR ( 'NONE', #5574, 1000.000000000000000 ) ;
#25212 = DIRECTION ( 'NONE',  ( 0.000000000000000000, 0.000000000000000000, -1.000000000000000000 ) ) ;
#25213 = ORIENTED_EDGE ( 'NONE', *, *, #33972, .F. ) ;
#25214 = ADVANCED_FACE ( 'NONE', ( #8835 ), #37214, .T. ) ;
#25215 = DIRECTION ( 'NONE',  ( 0.000000000000000000, -0.1205366802553130001, 0.9927088740980553050 ) ) ;
#25216 = DIRECTION ( 'NONE',  ( -0.000000000000000000, -0.4647231720437724478, -0.8854560256532078011 ) ) ;
#25217 = ORIENTED_EDGE ( 'NONE', *, *, #19261, .F. ) ;
#25218 = DIRECTION ( 'NONE',  ( 0.000000000000000000, -0.2393156642875516604, 0.9709418174260535661 ) ) ;
#25219 = ORIENTED_EDGE ( 'NONE', *, *, #5069, .F. ) ;
#25220 = LINE ( 'NONE', #8665, #48607 ) ;
#25221 = VECTOR ( 'NONE', #20964, 1000.000000000000000 ) ;
#25222 = DIRECTION ( 'NONE',  ( 0.000000000000000000, 1.000000000000000000, 0.000000000000000000 ) ) ;
#25223 = CARTESIAN_POINT ( 'NONE',  ( -95.18697522258266019, -177.1207230881787780, 115.9455772817713353 ) ) ;
#25224 = CARTESIAN_POINT ( 'NONE',  ( -173.4291566779743050, -189.7472609257535510, 3.534122433558314125 ) ) ;
#25225 = EDGE_LOOP ( 'NONE', ( #25654, #7889, #16376, #44639 ) ) ;
#25226 = PLANE ( 'NONE',  #24145 ) ;
#25227 = PLANE ( 'NONE',  #17660 ) ;
#25228 = LINE ( 'NONE', #29415, #25640 ) ;
#25229 = VERTEX_POINT ( 'NONE', #9890 ) ;
#25230 = LINE ( 'NONE', #1580, #4040 ) ;
#25231 = ORIENTED_EDGE ( 'NONE', *, *, #15429, .T. ) ;
#25232 = LINE ( 'NONE', #8676, #39287 ) ;
#25233 = ADVANCED_FACE ( 'NONE', ( #12769 ), #24873, .F. ) ;
#25234 = EDGE_CURVE ( 'NONE', #21107, #10986, #41675, .T. ) ;
#25235 = VECTOR ( 'NONE', #42097, 1000.000000000000114 ) ;
#25236 = CIRCLE ( 'NONE', #1751, 124.9999999999999858 ) ;
#25237 = DIRECTION ( 'NONE',  ( -0.000000000000000000, 1.000000000000000000, -0.000000000000000000 ) ) ;
#25238 = LINE ( 'NONE', #17107, #2582 ) ;
#25239 = ORIENTED_EDGE ( 'NONE', *, *, #26626, .T. ) ;
#25242 = EDGE_LOOP ( 'NONE', ( #11061, #24157, #35624, #44184 ) ) ;
#25241 = DIRECTION ( 'NONE',  ( 0.000000000000000000, 0.000000000000000000, -1.000000000000000000 ) ) ;
#25240 = DIRECTION ( 'NONE',  ( -0.000000000000000000, 0.8229838658936634577, 0.5680647467311457088 ) ) ;
#25243 = CARTESIAN_POINT ( 'NONE',  ( -330.4913330509368166, -123.5000000000000284, 0.000000000000000000 ) ) ;
#25244 = ORIENTED_EDGE ( 'NONE', *, *, #30055, .T. ) ;
#25245 = DIRECTION ( 'NONE',  ( 0.000000000000000000, 1.000000000000000000, -0.000000000000000000 ) ) ;
#25246 = DIRECTION ( 'NONE',  ( -0.000000000000000000, -1.000000000000000000, 0.000000000000000000 ) ) ;
#25247 = ORIENTED_EDGE ( 'NONE', *, *, #1081, .T. ) ;
#25248 = EDGE_CURVE ( 'NONE', #22157, #8359, #41935, .T. ) ;
#25249 = CARTESIAN_POINT ( 'NONE',  ( -48.47912675150885065, -177.1207230881787780, 6.938893903907228378E-15 ) ) ;
#25252 = ORIENTED_EDGE ( 'NONE', *, *, #26254, .T. ) ;
#25251 = DIRECTION ( 'NONE',  ( -1.000000000000000000, -0.000000000000000000, 0.000000000000000000 ) ) ;
#25250 = CARTESIAN_POINT ( 'NONE',  ( -339.1964088526558498, -68.51134412508150717, 21.38919645685156112 ) ) ;
#25253 = VERTEX_POINT ( 'NONE', #706 ) ;
#25254 = EDGE_CURVE ( 'NONE', #47106, #43249, #27327, .T. ) ;
#25255 = CARTESIAN_POINT ( 'NONE',  ( -169.9131040279660283, -177.1207230881787780, 29.64437826672835996 ) ) ;
#25256 = FACE_BOUND ( 'NONE', #47993, .T. ) ;
#25257 = ADVANCED_FACE ( 'NONE', ( #20941 ), #16998, .T. ) ;
#25259 = VECTOR ( 'NONE', #27993, 1000.000000000000000 ) ;
#25258 = DIRECTION ( 'NONE',  ( -0.2920567706369628924, 0.000000000000000000, -0.9564009842765264224 ) ) ;
#25260 = VERTEX_POINT ( 'NONE', #33008 ) ;
#25261 = DIRECTION ( 'NONE',  ( 0.000000000000000000, 0.000000000000000000, 1.000000000000000000 ) ) ;
#25262 = CARTESIAN_POINT ( 'NONE',  ( -336.3521761649654422, -111.9361751271348879, -57.91551518289410438 ) ) ;
#25263 = CARTESIAN_POINT ( 'NONE',  ( 21.21056010634072564, -193.5000000000000000, 103.7706487676302061 ) ) ;
#25264 = CARTESIAN_POINT ( 'NONE',  ( -85.77912150413021664, -193.5000000000000000, -119.3051146910911768 ) ) ;
#25265 = EDGE_CURVE ( 'NONE', #21281, #11883, #21718, .T. ) ;
#25266 = EDGE_LOOP ( 'NONE', ( #31300, #48364, #17716, #25079 ) ) ;
#25267 = PLANE ( 'NONE',  #19594 ) ;
#25268 = LINE ( 'NONE', #29204, #17237 ) ;
#25269 = DIRECTION ( 'NONE',  ( 0.000000000000000000, 0.000000000000000000, 1.000000000000000000 ) ) ;
#25270 = ORIENTED_EDGE ( 'NONE', *, *, #30466, .T. ) ;
#25271 = LINE ( 'NONE', #13189, #2142 ) ;
#25272 = FACE_OUTER_BOUND ( 'NONE', #35685, .T. ) ;
#25273 = AXIS2_PLACEMENT_3D ( 'NONE', #22877, #11288, #43374 ) ;
#25274 = DIRECTION ( 'NONE',  ( 0.000000000000000000, 1.000000000000000000, 0.000000000000000000 ) ) ;
#25275 = DIRECTION ( 'NONE',  ( 0.000000000000000000, 0.000000000000000000, -1.000000000000000000 ) ) ;
#25276 = AXIS2_PLACEMENT_3D ( 'NONE', #50680, #29401, #9442 ) ;
#25277 = DIRECTION ( 'NONE',  ( -0.000000000000000000, -1.000000000000000000, 0.000000000000000000 ) ) ;
#25278 = DIRECTION ( 'NONE',  ( 0.000000000000000000, 0.000000000000000000, 1.000000000000000000 ) ) ;
#25279 = CARTESIAN_POINT ( 'NONE',  ( -336.3521761649654422, -169.4076645216271402, -37.15394033962039089 ) ) ;
#25281 = ORIENTED_EDGE ( 'NONE', *, *, #5444, .T. ) ;
#25280 = DIRECTION ( 'NONE',  ( -0.000000000000000000, 1.000000000000000000, 0.000000000000000000 ) ) ;
#25282 = ORIENTED_EDGE ( 'NONE', *, *, #29540, .F. ) ;
#25283 = LINE ( 'NONE', #16888, #10668 ) ;
#25284 = CARTESIAN_POINT ( 'NONE',  ( 141.7825277784304205, -193.5000000000000000, 41.45482488023466772 ) ) ;
#25286 = VERTEX_POINT ( 'NONE', #1735 ) ;
#25285 = DIRECTION ( 'NONE',  ( -0.000000000000000000, 1.000000000000000000, -0.000000000000000000 ) ) ;
#25287 = ORIENTED_EDGE ( 'NONE', *, *, #45162, .T. ) ;
#25288 = VECTOR ( 'NONE', #42928, 999.9999999999998863 ) ;
#25289 = VERTEX_POINT ( 'NONE', #5175 ) ;
#25290 = DIRECTION ( 'NONE',  ( 0.000000000000000000, 0.000000000000000000, 1.000000000000000000 ) ) ;
#25291 = ADVANCED_FACE ( 'NONE', ( #34809 ), #10390, .T. ) ;
#25292 = EDGE_CURVE ( 'NONE', #49664, #3078, #6206, .T. ) ;
#25293 = ADVANCED_FACE ( 'NONE', ( #26414 ), #1990, .T. ) ;
#25294 = CARTESIAN_POINT ( 'NONE',  ( 38.71172987070723792, -189.7472609257535510, -89.56983042009264295 ) ) ;
#25295 = DIRECTION ( 'NONE',  ( 0.000000000000000000, 0.000000000000000000, -1.000000000000000000 ) ) ;
#25296 = ADVANCED_FACE ( 'NONE', ( #46664 ), #3022, .T. ) ;
#25297 = PLANE ( 'NONE',  #7570 ) ;
#25299 = ORIENTED_EDGE ( 'NONE', *, *, #24409, .F. ) ;
#25298 = DIRECTION ( 'NONE',  ( 0.4827922027307490205, 0.000000000000000000, -0.8757349421956345248 ) ) ;
#25300 = ADVANCED_FACE ( 'NONE', ( #21965 ), #38754, .F. ) ;
#25301 = EDGE_CURVE ( 'NONE', #51223, #20567, #27184, .T. ) ;
#25302 = DIRECTION ( 'NONE',  ( 0.000000000000000000, -1.066276696567077385E-13, -1.000000000000000000 ) ) ;
#25303 = VERTEX_POINT ( 'NONE', #19066 ) ;
#25304 = DIRECTION ( 'NONE',  ( -0.000000000000000000, 1.000000000000000000, 0.000000000000000000 ) ) ;
#25305 = AXIS2_PLACEMENT_3D ( 'NONE', #24880, #20948, #9628 ) ;
#25306 = ORIENTED_EDGE ( 'NONE', *, *, #34338, .T. ) ;
#25307 = PLANE ( 'NONE',  #46744 ) ;
#25308 = ADVANCED_FACE ( 'NONE', ( #2763 ), #42722, .T. ) ;
#25309 = CARTESIAN_POINT ( 'NONE',  ( -135.4258661347518284, -189.7472609257535510, -89.80681772907011862 ) ) ;
#25310 = VECTOR ( 'NONE', #6472, 1000.000000000000000 ) ;
#25311 = FACE_OUTER_BOUND ( 'NONE', #29963, .T. ) ;
#25312 = EDGE_CURVE ( 'NONE', #24349, #17499, #6474, .T. ) ;
#25313 = AXIS2_PLACEMENT_3D ( 'NONE', #29725, #33155, #49720 ) ;
#25314 = ORIENTED_EDGE ( 'NONE', *, *, #5633, .F. ) ;
#25315 = ORIENTED_EDGE ( 'NONE', *, *, #22993, .T. ) ;
#25316 = PLANE ( 'NONE',  #9698 ) ;
#25317 = ADVANCED_FACE ( 'NONE', ( #14877 ), #34313, .T. ) ;
#25318 = DIRECTION ( 'NONE',  ( 1.000000000000000000, -0.000000000000000000, -0.000000000000000000 ) ) ;
#25319 = ORIENTED_EDGE ( 'NONE', *, *, #43981, .F. ) ;
#25320 = DIRECTION ( 'NONE',  ( 0.000000000000000000, -0.9350162426854194964, -0.3546048870425235200 ) ) ;
#25321 = EDGE_CURVE ( 'NONE', #29760, #47693, #42482, .T. ) ;
#25322 = ORIENTED_EDGE ( 'NONE', *, *, #23427, .T. ) ;
#25323 = FACE_BOUND ( 'NONE', #49758, .T. ) ;
#25324 = AXIS2_PLACEMENT_3D ( 'NONE', #47585, #43624, #23644 ) ;
#25325 = LINE ( 'NONE', #45052, #23124 ) ;
#25326 = ORIENTED_EDGE ( 'NONE', *, *, #23675, .T. ) ;
#25327 = CARTESIAN_POINT ( 'NONE',  ( -171.7300019102062265, -177.1207230881787780, -20.83798868929513759 ) ) ;
#25328 = VERTEX_POINT ( 'NONE', #46159 ) ;
#25329 = PLANE ( 'NONE',  #25407 ) ;
#25330 = CARTESIAN_POINT ( 'NONE',  ( -127.0132498732365889, -177.1207230881787780, 97.24912084693261249 ) ) ;
#25331 = VERTEX_POINT ( 'NONE', #26153 ) ;
#25332 = FACE_OUTER_BOUND ( 'NONE', #13793, .T. ) ;
#25333 = DIRECTION ( 'NONE',  ( 1.000000000000000000, -0.000000000000000000, -0.000000000000000000 ) ) ;
#25334 = DIRECTION ( 'NONE',  ( 1.043714542225393697E-14, 0.9927088740980527515, -0.1205366802553337890 ) ) ;
#25335 = CARTESIAN_POINT ( 'NONE',  ( -332.3517673607765914, -82.40546666720629787, 42.41660376256258047 ) ) ;
#25336 = EDGE_CURVE ( 'NONE', #13870, #14725, #22222, .T. ) ;
#25337 = VERTEX_POINT ( 'NONE', #14603 ) ;
#25338 = CARTESIAN_POINT ( 'NONE',  ( -48.47912675150885065, -177.1207230881787780, 6.938893903907228378E-15 ) ) ;
#25339 = ORIENTED_EDGE ( 'NONE', *, *, #28306, .T. ) ;
#25340 = ORIENTED_EDGE ( 'NONE', *, *, #31143, .T. ) ;
#25341 = DIRECTION ( 'NONE',  ( -0.000000000000000000, 1.000000000000000000, 0.000000000000000000 ) ) ;
#25343 = ORIENTED_EDGE ( 'NONE', *, *, #11810, .T. ) ;
#25342 = DIRECTION ( 'NONE',  ( -0.9993908270190956511, 0.000000000000000000, 0.03489949670250096919 ) ) ;
#25344 = VECTOR ( 'NONE', #5119, 1000.000000000000000 ) ;
#25345 = ORIENTED_EDGE ( 'NONE', *, *, #18533, .T. ) ;
#25346 = DIRECTION ( 'NONE',  ( 0.000000000000000000, 1.000000000000000000, 0.000000000000000000 ) ) ;
#25347 = AXIS2_PLACEMENT_3D ( 'NONE', #42959, #31387, #51632 ) ;
#25348 = VECTOR ( 'NONE', #5848, 1000.000000000000114 ) ;
#25349 = EDGE_CURVE ( 'NONE', #29823, #25483, #14347, .T. ) ;
#25350 = FACE_OUTER_BOUND ( 'NONE', #30433, .T. ) ;
#25351 = VERTEX_POINT ( 'NONE', #30359 ) ;
#25352 = DIRECTION ( 'NONE',  ( 0.000000000000000000, 0.000000000000000000, 1.000000000000000000 ) ) ;
#25353 = ORIENTED_EDGE ( 'NONE', *, *, #34896, .T. ) ;
#25354 = PLANE ( 'NONE',  #43469 ) ;
#25355 = DIRECTION ( 'NONE',  ( -0.000000000000000000, -1.000000000000000000, 0.000000000000000000 ) ) ;
#25356 = EDGE_CURVE ( 'NONE', #22201, #50750, #38515, .T. ) ;
#25357 = ADVANCED_FACE ( 'NONE', ( #15132 ), #26689, .T. ) ;
#25358 = ADVANCED_FACE ( 'NONE', ( #47183 ), #23002, .F. ) ;
#25359 = CARTESIAN_POINT ( 'NONE',  ( -118.9967449635792462, -193.5000000000000000, -103.2098131075562009 ) ) ;
#25360 = DIRECTION ( 'NONE',  ( 0.000000000000000000, 0.000000000000000000, -1.000000000000000000 ) ) ;
#25361 = EDGE_LOOP ( 'NONE', ( #30025, #38046, #7829, #51474 ) ) ;
#25362 = VECTOR ( 'NONE', #35532, 1000.000000000000000 ) ;
#25363 = ORIENTED_EDGE ( 'NONE', *, *, #50850, .T. ) ;
#25364 = EDGE_CURVE ( 'NONE', #37475, #46340, #35587, .T. ) ;
#25365 = EDGE_LOOP ( 'NONE', ( #46711, #968, #20130, #1438 ) ) ;
#25366 = LINE ( 'NONE', #1449, #2278 ) ;
#25367 = CARTESIAN_POINT ( 'NONE',  ( -89.73513343757494454, -177.1207230881787780, -117.9955164924467397 ) ) ;
#25368 = AXIS2_PLACEMENT_3D ( 'NONE', #13379, #20740, #29390 ) ;
#25369 = AXIS2_PLACEMENT_3D ( 'NONE', #7205, #14582, #31366 ) ;
#25370 = DIRECTION ( 'NONE',  ( 1.000000000000000000, -0.000000000000000000, -0.000000000000000000 ) ) ;
#25371 = LINE ( 'NONE', #41389, #13806 ) ;
#25372 = ORIENTED_EDGE ( 'NONE', *, *, #1921, .F. ) ;
#25373 = PRODUCT_DEFINITION_CONTEXT ( 'detailed design', #2506, 'design' ) ;
#25374 = EDGE_CURVE ( 'NONE', #38762, #30320, #47707, .T. ) ;
#25375 = ORIENTED_EDGE ( 'NONE', *, *, #40547, .F. ) ;
#25377 = ORIENTED_EDGE ( 'NONE', *, *, #39805, .T. ) ;
#25376 = CYLINDRICAL_SURFACE ( 'NONE', #41618, 125.0000000000000000 ) ;
#25378 = EDGE_LOOP ( 'NONE', ( #3486, #50684, #43817, #42840 ) ) ;
#25379 = EDGE_CURVE ( 'NONE', #5922, #26098, #27709, .T. ) ;
#25380 = CARTESIAN_POINT ( 'NONE',  ( -332.3517673607765914, -173.5513585866778214, -31.34948880313881503 ) ) ;
#25381 = DIRECTION ( 'NONE',  ( 0.000000000000000000, 1.000000000000000000, -0.000000000000000000 ) ) ;
#25382 = CIRCLE ( 'NONE', #32081, 1.951623109906645226 ) ;
#25383 = CARTESIAN_POINT ( 'NONE',  ( -332.3517673607765914, -183.2372378732723632, -5.609136410542877371 ) ) ;
#25384 = EDGE_CURVE ( 'NONE', #11395, #11764, #23775, .T. ) ;
#25385 = FACE_OUTER_BOUND ( 'NONE', #15692, .T. ) ;
#25386 = LINE ( 'NONE', #37727, #51150 ) ;
#25387 = VERTEX_POINT ( 'NONE', #16157 ) ;
#25388 = LINE ( 'NONE', #29320, #40103 ) ;
#25389 = ORIENTED_EDGE ( 'NONE', *, *, #35032, .T. ) ;
#25390 = EDGE_CURVE ( 'NONE', #41176, #36336, #7232, .T. ) ;
#25391 = ORIENTED_EDGE ( 'NONE', *, *, #23468, .T. ) ;
#25392 = CARTESIAN_POINT ( 'NONE',  ( -330.4913330509368166, -109.8658467157472813, -57.40522506028090532 ) ) ;
#25393 =( NAMED_UNIT ( * ) PLANE_ANGLE_UNIT ( ) SI_UNIT ( $, .RADIAN. ) );
#25394 = CARTESIAN_POINT ( 'NONE',  ( -260.0000000000000000, -123.5000000000000284, -20.00000000000001066 ) ) ;
#25395 = EDGE_LOOP ( 'NONE', ( #6828, #34283, #20365, #35422 ) ) ;
#25396 = DIRECTION ( 'NONE',  ( 0.000000000000000000, -0.5680647467311540355, 0.8229838658936575735 ) ) ;
#25397 = DIRECTION ( 'NONE',  ( 0.3482016354343866471, 0.000000000000000000, 0.9374196611341253371 ) ) ;
#25398 = DIRECTION ( 'NONE',  ( 0.000000000000000000, 0.000000000000000000, 1.000000000000000000 ) ) ;
#25399 = DIRECTION ( 'NONE',  ( -0.000000000000000000, -1.000000000000000000, -0.000000000000000000 ) ) ;
#25400 = AXIS2_PLACEMENT_3D ( 'NONE', #16044, #44677, #40710 ) ;
#25401 = AXIS2_PLACEMENT_3D ( 'NONE', #40550, #32683, #1129 ) ;
#25402 = EDGE_CURVE ( 'NONE', #29823, #39129, #40047, .T. ) ;
#25403 = PLANE ( 'NONE',  #3461 ) ;
#25404 = FACE_BOUND ( 'NONE', #25551, .T. ) ;
#25405 = ORIENTED_EDGE ( 'NONE', *, *, #30344, .F. ) ;
#25406 = VECTOR ( 'NONE', #48013, 1000.000000000000114 ) ;
#25407 = AXIS2_PLACEMENT_3D ( 'NONE', #21655, #37676, #41344 ) ;
#25408 = DIRECTION ( 'NONE',  ( 0.000000000000000000, 1.000000000000000000, 0.000000000000000000 ) ) ;
#25409 = VERTEX_POINT ( 'NONE', #39781 ) ;
#25410 = VERTEX_POINT ( 'NONE', #3799 ) ;
#25411 = CARTESIAN_POINT ( 'NONE',  ( -173.4787860028527007, -183.6283474603465606, 0.2918682030023308505 ) ) ;
#25412 = ORIENTED_EDGE ( 'NONE', *, *, #6209, .F. ) ;
#25413 = CARTESIAN_POINT ( 'NONE',  ( -26.20043062753592977, -175.3837268820161057, -122.9986166548863196 ) ) ;
#25414 = CARTESIAN_POINT ( 'NONE',  ( -336.3521761649654422, -91.32752733096738496, -49.48329383994654052 ) ) ;
#25416 = ORIENTED_EDGE ( 'NONE', *, *, #11231, .T. ) ;
#25415 = FACE_OUTER_BOUND ( 'NONE', #24575, .T. ) ;
#25417 = ADVANCED_FACE ( 'NONE', ( #31659 ), #19570, .T. ) ;
#25418 = EDGE_CURVE ( 'NONE', #37409, #1436, #18971, .T. ) ;
#25419 = DIRECTION ( 'NONE',  ( -0.6528221181905119463, 0.000000000000000000, -0.7575112421616284619 ) ) ;
#25420 = ORIENTED_EDGE ( 'NONE', *, *, #17167, .F. ) ;
#25421 = ORIENTED_EDGE ( 'NONE', *, *, #27608, .T. ) ;
#25422 = CIRCLE ( 'NONE', #8600, 125.0000000000000000 ) ;
#25423 = EDGE_LOOP ( 'NONE', ( #12171, #18016, #6778, #27155 ) ) ;
#25424 = LINE ( 'NONE', #25171, #20895 ) ;
#25425 = DIRECTION ( 'NONE',  ( -0.5586467658036415873, 0.000000000000000000, -0.8294056854502090959 ) ) ;
#25426 = ORIENTED_EDGE ( 'NONE', *, *, #49119, .F. ) ;
#25427 = SURFACE_STYLE_USAGE ( .BOTH. , #40389 ) ;
#25428 = LINE ( 'NONE', #21487, #45482 ) ;
#25429 = DIRECTION ( 'NONE',  ( 1.000000000000000000, -0.000000000000000000, -0.000000000000000000 ) ) ;
#25430 = ORIENTED_EDGE ( 'NONE', *, *, #8121, .T. ) ;
#25431 = CIRCLE ( 'NONE', #32998, 125.0000000000000000 ) ;
#25432 = VECTOR ( 'NONE', #15207, 1000.000000000000000 ) ;
#25433 = LINE ( 'NONE', #21490, #6624 ) ;
#25434 = CARTESIAN_POINT ( 'NONE',  ( -332.3517673607765914, -123.5000000000000284, 0.000000000000000000 ) ) ;
#25435 = ORIENTED_EDGE ( 'NONE', *, *, #22931, .F. ) ;
#25437 = VERTEX_POINT ( 'NONE', #39288 ) ;
#25436 = DIRECTION ( 'NONE',  ( 0.000000000000000000, 1.000000000000000000, 0.000000000000000000 ) ) ;
#25438 = CIRCLE ( 'NONE', #47281, 4.999999999999997335 ) ;
#25439 = ORIENTED_EDGE ( 'NONE', *, *, #31929, .F. ) ;
#25440 = EDGE_CURVE ( 'NONE', #40342, #41178, #8054, .T. ) ;
#25441 = VERTEX_POINT ( 'NONE', #31913 ) ;
#25442 = DIRECTION ( 'NONE',  ( 0.000000000000000000, 0.000000000000000000, 1.000000000000000000 ) ) ;
#25443 = DIRECTION ( 'NONE',  ( 0.000000000000000000, 0.000000000000000000, -1.000000000000000000 ) ) ;
#25444 = ORIENTED_EDGE ( 'NONE', *, *, #14421, .F. ) ;
#25445 = CARTESIAN_POINT ( 'NONE',  ( -47.63353074800703268, -193.5000000000000000, 0.5338233779648018373 ) ) ;
#25446 = AXIS2_PLACEMENT_3D ( 'NONE', #16768, #7816, #28037 ) ;
#25447 = CYLINDRICAL_SURFACE ( 'NONE', #4955, 125.0000000000000000 ) ;
#25448 = EDGE_LOOP ( 'NONE', ( #3675, #9447, #14284, #30327 ) ) ;
#25449 = LINE ( 'NONE', #46211, #23320 ) ;
#25450 = ORIENTED_EDGE ( 'NONE', *, *, #45146, .F. ) ;
#25451 = EDGE_CURVE ( 'NONE', #14387, #6882, #23987, .T. ) ;
#25452 = EDGE_LOOP ( 'NONE', ( #23903, #16106, #17827, #5022 ) ) ;
#25453 = DIRECTION ( 'NONE',  ( 1.000000000000000000, -0.000000000000000000, -0.000000000000000000 ) ) ;
#25454 = DIRECTION ( 'NONE',  ( 1.000000000000000000, 0.000000000000000000, -0.000000000000000000 ) ) ;
#25455 = CARTESIAN_POINT ( 'NONE',  ( -49.13194886969936448, -189.7472609257535510, -0.7575112421616214675 ) ) ;
#25456 = VERTEX_POINT ( 'NONE', #36371 ) ;
#25457 = DIRECTION ( 'NONE',  ( 0.7765238627180349740, 0.000000000000000000, 0.6300878435817203194 ) ) ;
#25458 = AXIS2_PLACEMENT_3D ( 'NONE', #2393, #27056, #42837 ) ;
#25459 = CARTESIAN_POINT ( 'NONE',  ( 42.10477485469927927, -193.5000000000000000, 86.13684908212515268 ) ) ;
#25460 = SHAPE_DEFINITION_REPRESENTATION ( #2083, #33452 ) ;
#25461 = DIRECTION ( 'NONE',  ( 0.000000000000000000, 1.000000000000000000, 0.000000000000000000 ) ) ;
#25462 = CARTESIAN_POINT ( 'NONE',  ( -167.9436818089035057, -177.1207230881787780, 36.78613984830045069 ) ) ;
#25463 = DIRECTION ( 'NONE',  ( -1.000000000000000000, -7.812315528781888245E-15, -6.921107616850760573E-15 ) ) ;
#25464 = VECTOR ( 'NONE', #51864, 1000.000000000000000 ) ;
#25465 = CARTESIAN_POINT ( 'NONE',  ( 35.45604639379469347, -177.1207230881787780, 91.27439114664650788 ) ) ;
#25466 = ORIENTED_EDGE ( 'NONE', *, *, #17338, .T. ) ;
#25467 = CARTESIAN_POINT ( 'NONE',  ( -99.62791064391781504, -189.7472609257535510, -114.0561348912352315 ) ) ;
#25468 = CARTESIAN_POINT ( 'NONE',  ( -336.3521761649654422, -64.73342574900661361, 5.491276508483657892 ) ) ;
#25469 = ORIENTED_EDGE ( 'NONE', *, *, #27572, .F. ) ;
#25470 = ORIENTED_EDGE ( 'NONE', *, *, #12598, .T. ) ;
#25471 = VECTOR ( 'NONE', #1649, 1000.000000000000000 ) ;
#25472 = ORIENTED_EDGE ( 'NONE', *, *, #3742, .F. ) ;
#25473 = CARTESIAN_POINT ( 'NONE',  ( 75.67769207106684348, -177.1207230881787780, 14.49428645563876650 ) ) ;
#25474 = CIRCLE ( 'NONE', #20434, 125.0000000000000000 ) ;
#25475 = DIRECTION ( 'NONE',  ( -0.000000000000000000, 0.8854560256532093554, -0.4647231720437695057 ) ) ;
#25476 = FACE_OUTER_BOUND ( 'NONE', #15674, .T. ) ;
#25477 = FACE_OUTER_BOUND ( 'NONE', #12043, .T. ) ;
#25478 = LINE ( 'NONE', #33101, #608 ) ;
#25479 = ADVANCED_FACE ( 'NONE', ( #4073 ), #7497, .F. ) ;
#25480 = LINE ( 'NONE', #15470, #31092 ) ;
#25481 = EDGE_LOOP ( 'NONE', ( #38256, #42199, #25831, #34031 ) ) ;
#25482 = LINE ( 'NONE', #5530, #21451 ) ;
#25483 = VERTEX_POINT ( 'NONE', #12193 ) ;
#25484 = DIRECTION ( 'NONE',  ( 0.000000000000000000, 0.000000000000000000, 1.000000000000000000 ) ) ;
#25485 = ADVANCED_FACE ( 'NONE', ( #44272 ), #8263, .F. ) ;
#25486 = ORIENTED_EDGE ( 'NONE', *, *, #39814, .T. ) ;
#25487 = DIRECTION ( 'NONE',  ( 0.9564009842765202052, 0.000000000000000000, 0.2920567706369833760 ) ) ;
#25488 = AXIS2_PLACEMENT_3D ( 'NONE', #48342, #40433, #4452 ) ;
#25489 = ORIENTED_EDGE ( 'NONE', *, *, #41387, .F. ) ;
#25490 = AXIS2_PLACEMENT_3D ( 'NONE', #42515, #11487, #34381 ) ;
#25491 = FACE_OUTER_BOUND ( 'NONE', #9818, .T. ) ;
#25492 = CARTESIAN_POINT ( 'NONE',  ( 0.000000000000000000, -64.93017642821470758, 7.111664135063263892 ) ) ;
#25493 = ORIENTED_EDGE ( 'NONE', *, *, #2802, .F. ) ;
#25496 = ORIENTED_EDGE ( 'NONE', *, *, #23840, .F. ) ;
#25495 = CARTESIAN_POINT ( 'NONE',  ( -365.0000000000001137, -168.5000000000000284, -5.000000000000001776 ) ) ;
#25494 = CARTESIAN_POINT ( 'NONE',  ( 8.448131207122518305, -175.3837268820161057, 111.2847127925100352 ) ) ;
#25497 = EDGE_CURVE ( 'NONE', #11938, #22244, #40303, .T. ) ;
#25498 = LINE ( 'NONE', #41515, #45770 ) ;
#25499 = ORIENTED_EDGE ( 'NONE', *, *, #40643, .F. ) ;
#25500 = LINE ( 'NONE', #17879, #19695 ) ;
#25501 = ORIENTED_EDGE ( 'NONE', *, *, #47229, .F. ) ;
#25502 = DIRECTION ( 'NONE',  ( -0.000000000000000000, 1.000000000000000000, -0.000000000000000000 ) ) ;
#25505 = ORIENTED_EDGE ( 'NONE', *, *, #29462, .T. ) ;
#25504 = LINE ( 'NONE', #41522, #655 ) ;
#25503 = DIRECTION ( 'NONE',  ( -1.000000000000000000, -4.850383327711889945E-15, 9.241633304753590273E-15 ) ) ;
#25506 = VECTOR ( 'NONE', #37647, 1000.000000000000114 ) ;
#25507 = ORIENTED_EDGE ( 'NONE', *, *, #42262, .T. ) ;
#25508 = LINE ( 'NONE', #12375, #10568 ) ;
#25509 = LINE ( 'NONE', #49454, #47999 ) ;
#25510 = CARTESIAN_POINT ( 'NONE',  ( -168.1386673294336163, -189.7472609257535510, 32.52067927015837512 ) ) ;
#25511 = ORIENTED_EDGE ( 'NONE', *, *, #7621, .T. ) ;
#25512 = DIRECTION ( 'NONE',  ( 0.8124868780056742068, 0.000000000000000000, 0.5829794791144820021 ) ) ;
#25513 = LINE ( 'NONE', #5560, #2245 ) ;
#25514 = DIRECTION ( 'NONE',  ( 0.000000000000000000, 0.000000000000000000, -1.000000000000000000 ) ) ;
#25515 = CARTESIAN_POINT ( 'NONE',  ( 55.35935253854127325, -177.1207230881787780, 69.58857822035042773 ) ) ;
#25516 = ORIENTED_EDGE ( 'NONE', *, *, #12422, .T. ) ;
#25517 = DIRECTION ( 'NONE',  ( 0.000000000000000000, 0.000000000000000000, -1.000000000000000000 ) ) ;
#25518 = CARTESIAN_POINT ( 'NONE',  ( 29.40217425202904167, -183.6283474603465606, -96.49160960477045990 ) ) ;
#25519 = DIRECTION ( 'NONE',  ( 0.000000000000000000, 0.5000000000000013323, -0.8660254037844380415 ) ) ;
#25520 = EDGE_LOOP ( 'NONE', ( #23654, #25217, #51544, #3948 ) ) ;
#25521 = LINE ( 'NONE', #5572, #37410 ) ;
#25522 = DIRECTION ( 'NONE',  ( 0.000000000000000000, 0.000000000000000000, 1.000000000000000000 ) ) ;
#25523 = VECTOR ( 'NONE', #36876, 1000.000000000000114 ) ;
#25524 = CARTESIAN_POINT ( 'NONE',  ( -170.0000000000000284, -113.5000000000000000, 60.00000000000000711 ) ) ;
#25525 = ADVANCED_FACE ( 'NONE', ( #16420 ), #32436, .F. ) ;
#25526 = FACE_OUTER_BOUND ( 'NONE', #3914, .T. ) ;
#25527 = CIRCLE ( 'NONE', #47334, 60.00000000000000000 ) ;
#25528 = LINE ( 'NONE', #33677, #2771 ) ;
#25529 = ADVANCED_FACE ( 'NONE', ( #19326 ), #47434, .F. ) ;
#25530 = DIRECTION ( 'NONE',  ( 0.000000000000000000, 0.000000000000000000, 1.000000000000000000 ) ) ;
#25531 = DIRECTION ( 'NONE',  ( -1.000000000000000000, 0.000000000000000000, 0.000000000000000000 ) ) ;
#25533 = VERTEX_POINT ( 'NONE', #48735 ) ;
#25532 = LINE ( 'NONE', #29727, #32918 ) ;
#25534 = ORIENTED_EDGE ( 'NONE', *, *, #4956, .F. ) ;
#25535 = LINE ( 'NONE', #40777, #24111 ) ;
#25536 = EDGE_CURVE ( 'NONE', #33118, #7989, #16465, .T. ) ;
#25537 = AXIS2_PLACEMENT_3D ( 'NONE', #17754, #40598, #32979 ) ;
#25538 = ADVANCED_FACE ( 'NONE', ( #5369 ), #17194, .T. ) ;
#25539 = DIRECTION ( 'NONE',  ( -0.7378332790417285736, 0.000000000000000000, 0.6749830015182091136 ) ) ;
#25541 = EDGE_LOOP ( 'NONE', ( #10806, #24016 ) ) ;
#25540 = LINE ( 'NONE', #37365, #42123 ) ;
#25542 = ORIENTED_EDGE ( 'NONE', *, *, #4735, .T. ) ;
#25543 = ADVANCED_FACE ( 'NONE', ( #1681 ), #4857, .T. ) ;
#25544 = ORIENTED_EDGE ( 'NONE', *, *, #30356, .T. ) ;
#25545 = CARTESIAN_POINT ( 'NONE',  ( -48.47912675150885065, -183.6283474603465606, 6.938893903907228378E-15 ) ) ;
#25546 = LINE ( 'NONE', #49995, #23591 ) ;
#25547 = CARTESIAN_POINT ( 'NONE',  ( -48.47912675150885065, -177.1207230881787780, 6.938893903907228378E-15 ) ) ;
#25548 = ORIENTED_EDGE ( 'NONE', *, *, #13327, .T. ) ;
#25549 = FACE_OUTER_BOUND ( 'NONE', #29952, .T. ) ;
#25551 = EDGE_LOOP ( 'NONE', ( #48770, #1523, #5981, #25639 ) ) ;
#25550 = FACE_OUTER_BOUND ( 'NONE', #34779, .T. ) ;
#25552 = CARTESIAN_POINT ( 'NONE',  ( 63.31225588004632243, -177.1207230881787780, 55.92572546981597981 ) ) ;
#25553 = CIRCLE ( 'NONE', #5429, 125.0000000000000000 ) ;
#25554 = ORIENTED_EDGE ( 'NONE', *, *, #40415, .F. ) ;
#25555 = CARTESIAN_POINT ( 'NONE',  ( 0.000000000000000000, 95.86090687668166765, -116.2794792057534607 ) ) ;
#25556 = ORIENTED_EDGE ( 'NONE', *, *, #41539, .F. ) ;
#25557 = CARTESIAN_POINT ( 'NONE',  ( -336.3521761649654422, -127.9985676343858501, 58.88711093124869222 ) ) ;
#25558 = CYLINDRICAL_SURFACE ( 'NONE', #22132, 125.0000000000000000 ) ;
#25559 = DIRECTION ( 'NONE',  ( 0.9646355819083576311, 0.000000000000000000, 0.2635871660690715101 ) ) ;
#25560 = AXIS2_PLACEMENT_3D ( 'NONE', #11102, #38451, #14290 ) ;
#25561 = VERTEX_POINT ( 'NONE', #32941 ) ;
#25562 = ORIENTED_EDGE ( 'NONE', *, *, #47853, .F. ) ;
#25563 = CARTESIAN_POINT ( 'NONE',  ( -160.0000000000000284, -123.5000000000000284, -41.63467731922663972 ) ) ;
#25564 = CARTESIAN_POINT ( 'NONE',  ( -148.6149069237406195, -183.6283474603465606, -74.81861753132353954 ) ) ;
#25565 = ORIENTED_EDGE ( 'NONE', *, *, #7644, .F. ) ;
#25566 = CARTESIAN_POINT ( 'NONE',  ( 27.23560471289044571, -193.5000000000000000, 99.45993886622845537 ) ) ;
#25567 = EDGE_LOOP ( 'NONE', ( #18028, #46191, #50131, #1281 ) ) ;
#25568 = DIRECTION ( 'NONE',  ( -0.9564009842765223146, 0.000000000000000000, -0.2920567706369764371 ) ) ;
#25569 = CIRCLE ( 'NONE', #16353, 125.0000000000000000 ) ;
#25570 = CARTESIAN_POINT ( 'NONE',  ( -160.0000000000000284, -123.5000000000000284, 41.63467731922665394 ) ) ;
#25571 = ORIENTED_EDGE ( 'NONE', *, *, #4283, .T. ) ;
#25572 = PLANE ( 'NONE',  #24083 ) ;
#25573 = ORIENTED_EDGE ( 'NONE', *, *, #8282, .F. ) ;
#25574 = DIRECTION ( 'NONE',  ( 0.000000000000000000, -0.000000000000000000, -1.000000000000000000 ) ) ;
#25575 = DIRECTION ( 'NONE',  ( 0.000000000000000000, 1.000000000000000000, -0.000000000000000000 ) ) ;
#25576 = ORIENTED_EDGE ( 'NONE', *, *, #13621, .T. ) ;
#25577 = DIRECTION ( 'NONE',  ( 0.000000000000000000, 0.000000000000000000, -1.000000000000000000 ) ) ;
#25578 = EDGE_CURVE ( 'NONE', #4233, #30593, #44524, .T. ) ;
#25579 = FACE_OUTER_BOUND ( 'NONE', #132, .T. ) ;
#25580 = LINE ( 'NONE', #1420, #7295 ) ;
#25581 = EDGE_CURVE ( 'NONE', #1746, #7213, #39916, .T. ) ;
#25582 = LINE ( 'NONE', #17725, #10628 ) ;
#25583 = ORIENTED_EDGE ( 'NONE', *, *, #9224, .F. ) ;
#25584 = DIRECTION ( 'NONE',  ( 0.000000000000000000, -1.000000000000000000, 0.000000000000000000 ) ) ;
#25585 = ORIENTED_EDGE ( 'NONE', *, *, #46229, .F. ) ;
#25586 = VECTOR ( 'NONE', #6259, 1000.000000000000000 ) ;
#25587 = CARTESIAN_POINT ( 'NONE',  ( -150.5816505765687623, -193.5000000000000000, 70.36529243996409377 ) ) ;
#25589 = EDGE_LOOP ( 'NONE', ( #37174, #419, #31646, #21359 ) ) ;
#25588 = LINE ( 'NONE', #5651, #40419 ) ;
#25590 = EDGE_CURVE ( 'NONE', #48757, #26725, #45020, .T. ) ;
#25591 = CIRCLE ( 'NONE', #45755, 125.0000000000000000 ) ;
#25592 = VECTOR ( 'NONE', #21781, 1000.000000000000000 ) ;
#25593 = ORIENTED_EDGE ( 'NONE', *, *, #30437, .F. ) ;
#25594 = DIRECTION ( 'NONE',  ( -0.000000000000000000, 1.000000000000000000, -0.000000000000000000 ) ) ;
#25595 = EDGE_CURVE ( 'NONE', #32525, #41934, #5640, .T. ) ;
#25596 = VECTOR ( 'NONE', #34883, 999.9999999999998863 ) ;
#25597 = EDGE_CURVE ( 'NONE', #5146, #39324, #37424, .T. ) ;
#25598 = DIRECTION ( 'NONE',  ( -0.000000000000000000, 1.000000000000000000, -0.000000000000000000 ) ) ;
#25599 = ORIENTED_EDGE ( 'NONE', *, *, #12541, .T. ) ;
#25600 = ADVANCED_FACE ( 'NONE', ( #16933 ), #5113, .T. ) ;
#25601 = CARTESIAN_POINT ( 'NONE',  ( -48.47912675150885065, -175.3837268820161057, 6.938893903907228378E-15 ) ) ;
#25602 = AXIS2_PLACEMENT_3D ( 'NONE', #4686, #20712, #36748 ) ;
#25603 = ORIENTED_EDGE ( 'NONE', *, *, #10816, .T. ) ;
#25604 = CARTESIAN_POINT ( 'NONE',  ( -12.10142301649613827, -193.5000000000000000, -118.5439281552630604 ) ) ;
#25605 = CARTESIAN_POINT ( 'NONE',  ( -336.3521761649653854, -171.9335100611925213, 35.41461708323791413 ) ) ;
#25606 = AXIS2_PLACEMENT_3D ( 'NONE', #910, #8532, #12482 ) ;
#25607 = EDGE_CURVE ( 'NONE', #39414, #4155, #48994, .T. ) ;
#25609 = CIRCLE ( 'NONE', #18081, 60.00000000000000000 ) ;
#25608 = CARTESIAN_POINT ( 'NONE',  ( -6.938893903907228378E-15, -63.50000000000000000, 0.000000000000000000 ) ) ;
#25610 = DIRECTION ( 'NONE',  ( -1.000000000000000000, -0.000000000000000000, -0.000000000000000000 ) ) ;
#25611 = ORIENTED_EDGE ( 'NONE', *, *, #4486, .F. ) ;
#25612 = VERTEX_POINT ( 'NONE', #49259 ) ;
#25613 = EDGE_LOOP ( 'NONE', ( #46791, #6013, #27040, #20023 ) ) ;
#25614 = VECTOR ( 'NONE', #26514, 1000.000000000000000 ) ;
#25615 = CARTESIAN_POINT ( 'NONE',  ( -330.4913330509368166, -131.2283041299249362, -59.50019592636134291 ) ) ;
#25616 = CARTESIAN_POINT ( 'NONE',  ( -48.47912675150885065, -177.1207230881787780, 6.938893903907228378E-15 ) ) ;
#25617 = DIRECTION ( 'NONE',  ( 0.000000000000000000, 0.000000000000000000, 1.000000000000000000 ) ) ;
#25618 = LINE ( 'NONE', #1711, #16307 ) ;
#25619 = VERTEX_POINT ( 'NONE', #21123 ) ;
#25620 = ORIENTED_EDGE ( 'NONE', *, *, #22210, .F. ) ;
#25622 = ORIENTED_EDGE ( 'NONE', *, *, #42303, .F. ) ;
#25621 = DIRECTION ( 'NONE',  ( 0.000000000000000000, 0.000000000000000000, 1.000000000000000000 ) ) ;
#25623 = ORIENTED_EDGE ( 'NONE', *, *, #16284, .F. ) ;
#25624 = AXIS2_PLACEMENT_3D ( 'NONE', #33426, #49705, #45260 ) ;
#25625 = CARTESIAN_POINT ( 'NONE',  ( -89.44307666693794090, -177.1207230881787780, -117.0391155081702266 ) ) ;
#25626 = DIRECTION ( 'NONE',  ( 0.000000000000000000, -0.3546048870425396182, -0.9350162426854132791 ) ) ;
#25627 = VECTOR ( 'NONE', #38935, 1000.000000000000000 ) ;
#25628 = VECTOR ( 'NONE', #32878, 1000.000000000000114 ) ;
#25629 = CARTESIAN_POINT ( 'NONE',  ( -59.28786813212838069, -177.1207230881787780, 124.5318076226587323 ) ) ;
#25630 = PLANE ( 'NONE',  #46904 ) ;
#25631 = VERTEX_POINT ( 'NONE', #17470 ) ;
#25632 = CARTESIAN_POINT ( 'NONE',  ( -336.3521761649654422, -123.5000000000000284, 0.000000000000000000 ) ) ;
#25633 = ORIENTED_EDGE ( 'NONE', *, *, #37390, .F. ) ;
#25634 = EDGE_CURVE ( 'NONE', #39414, #35024, #34897, .T. ) ;
#25635 = ORIENTED_EDGE ( 'NONE', *, *, #19626, .T. ) ;
#25636 = CARTESIAN_POINT ( 'NONE',  ( -111.3904503173946381, -189.7472609257535510, -106.8558168688113454 ) ) ;
#25637 = AXIS2_PLACEMENT_3D ( 'NONE', #31704, #8553, #151 ) ;
#25638 = LINE ( 'NONE', #34310, #13565 ) ;
#25639 = ORIENTED_EDGE ( 'NONE', *, *, #12198, .F. ) ;
#25640 = VECTOR ( 'NONE', #24705, 1000.000000000000000 ) ;
#25641 = ADVANCED_FACE ( 'NONE', ( #33489 ), #49526, .T. ) ;
#25642 = ADVANCED_FACE ( 'NONE', ( #45064 ), #1143, .F. ) ;
#25643 = CARTESIAN_POINT ( 'NONE',  ( -173.2419626162308646, -177.1207230881787780, 7.696413904698416353 ) ) ;
#25644 = ADVANCED_FACE ( 'NONE', ( #25332 ), #4579, .T. ) ;
#25645 = CARTESIAN_POINT ( 'NONE',  ( -129.4514457347087273, -175.3837268820161057, 95.22858582633115532 ) ) ;
#25646 = DIRECTION ( 'NONE',  ( 0.000000000000000000, 0.000000000000000000, 1.000000000000000000 ) ) ;
#25647 = EDGE_CURVE ( 'NONE', #46182, #42588, #9560, .T. ) ;
#25648 = AXIS2_PLACEMENT_3D ( 'NONE', #26675, #50592, #42705 ) ;
#25649 = PLANE ( 'NONE',  #28243 ) ;
#25650 = EDGE_CURVE ( 'NONE', #47079, #32649, #11416, .T. ) ;
#25652 = VECTOR ( 'NONE', #2742, 1000.000000000000000 ) ;
#25651 = CARTESIAN_POINT ( 'NONE',  ( 74.95461934957533856, -189.7472609257535510, -11.83705339977243121 ) ) ;
#25653 = DIRECTION ( 'NONE',  ( 0.000000000000000000, 1.000000000000000000, 0.000000000000000000 ) ) ;
#25654 = ORIENTED_EDGE ( 'NONE', *, *, #5272, .F. ) ;
#25655 = EDGE_CURVE ( 'NONE', #14417, #49807, #29777, .T. ) ;
#25656 = CARTESIAN_POINT ( 'NONE',  ( -29.73468717939733352, -177.1207230881787780, 123.5865930638410930 ) ) ;
#25657 = VERTEX_POINT ( 'NONE', #37935 ) ;
#25658 = VERTEX_POINT ( 'NONE', #42128 ) ;
#25659 = DIRECTION ( 'NONE',  ( 0.000000000000000000, 0.000000000000000000, -1.000000000000000000 ) ) ;
#25660 = EDGE_CURVE ( 'NONE', #21253, #33963, #38450, .T. ) ;
#25661 = ORIENTED_EDGE ( 'NONE', *, *, #25745, .T. ) ;
#25662 = EDGE_CURVE ( 'NONE', #6819, #39220, #42655, .T. ) ;
#25663 = CARTESIAN_POINT ( 'NONE',  ( -48.93575598890257794, -193.5000000000000000, 0.8896570909947506545 ) ) ;
#25664 = VECTOR ( 'NONE', #3408, 1000.000000000000000 ) ;
#25665 = EDGE_CURVE ( 'NONE', #32381, #20194, #2458, .T. ) ;
#25666 = LINE ( 'NONE', #25414, #23433 ) ;
#25668 = ORIENTED_EDGE ( 'NONE', *, *, #37092, .T. ) ;
#25667 = CARTESIAN_POINT ( 'NONE',  ( -305.0000000000000568, -67.22367097967905636, 20.80804632820150957 ) ) ;
#25669 = AXIS2_PLACEMENT_3D ( 'NONE', #13949, #29975, #34680 ) ;
#25670 = AXIS2_PLACEMENT_3D ( 'NONE', #36496, #32572, #776 ) ;
#25671 = EDGE_CURVE ( 'NONE', #12665, #20473, #2191, .T. ) ;
#25672 = DIRECTION ( 'NONE',  ( 1.000000000000000000, 0.000000000000000000, 0.000000000000000000 ) ) ;
#25673 = ORIENTED_EDGE ( 'NONE', *, *, #19483, .T. ) ;
#25674 = ORIENTED_EDGE ( 'NONE', *, *, #35426, .T. ) ;
#25675 = EDGE_CURVE ( 'NONE', #48486, #50678, #8915, .T. ) ;
#25676 = EDGE_LOOP ( 'NONE', ( #36503, #20835, #44817, #50326 ) ) ;
#25677 = CARTESIAN_POINT ( 'NONE',  ( -340.0000000000000568, -63.50000000000002842, 0.000000000000000000 ) ) ;
#25678 = PLANE ( 'NONE',  #31870 ) ;
#25679 = ORIENTED_EDGE ( 'NONE', *, *, #5091, .T. ) ;
#25680 = AXIS2_PLACEMENT_3D ( 'NONE', #51060, #31838, #39448 ) ;
#25681 = PLANE ( 'NONE',  #18403 ) ;
#25682 = AXIS2_PLACEMENT_3D ( 'NONE', #46936, #37986, #31138 ) ;
#25683 = DIRECTION ( 'NONE',  ( -0.000000000000000000, 1.000000000000000000, -0.000000000000000000 ) ) ;
#25684 = DIRECTION ( 'NONE',  ( 0.000000000000000000, 0.000000000000000000, 1.000000000000000000 ) ) ;
#25685 = ORIENTED_EDGE ( 'NONE', *, *, #43924, .F. ) ;
#25686 = VECTOR ( 'NONE', #47043, 1000.000000000000000 ) ;
#25687 = EDGE_CURVE ( 'NONE', #38237, #41833, #25853, .T. ) ;
#25688 = EDGE_CURVE ( 'NONE', #2579, #31941, #50551, .T. ) ;
#25689 = AXIS2_PLACEMENT_3D ( 'NONE', #45171, #10372, #29106 ) ;
#25690 = CARTESIAN_POINT ( 'NONE',  ( 0.000000000000000000, -89.98417994286123189, 48.55604808772534398 ) ) ;
#25691 = DIRECTION ( 'NONE',  ( -1.000000000000000000, -0.000000000000000000, -0.000000000000000000 ) ) ;
#25692 = ORIENTED_EDGE ( 'NONE', *, *, #20184, .T. ) ;
#25694 = EDGE_LOOP ( 'NONE', ( #12118, #3663, #22969, #49820 ) ) ;
#25693 = CARTESIAN_POINT ( 'NONE',  ( 76.21810084846656252, -193.5000000000000000, -8.694908215727984668 ) ) ;
#25695 = ORIENTED_EDGE ( 'NONE', *, *, #39109, .T. ) ;
#25696 = ORIENTED_EDGE ( 'NONE', *, *, #14835, .F. ) ;
#25697 = CARTESIAN_POINT ( 'NONE',  ( -336.3521761649654422, -81.78065195202964333, 43.12187378178631292 ) ) ;
#25698 = DIRECTION ( 'NONE',  ( 0.000000000000000000, 0.2393156642875685913, 0.9709418174260493473 ) ) ;
#25699 = ORIENTED_EDGE ( 'NONE', *, *, #41210, .T. ) ;
#25700 = DIRECTION ( 'NONE',  ( -0.000000000000000000, 1.000000000000000000, -0.000000000000000000 ) ) ;
#25701 = CARTESIAN_POINT ( 'NONE',  ( -330.4913330509368166, -66.33409060400670398, -14.60509510167892522 ) ) ;
#25702 = ORIENTED_EDGE ( 'NONE', *, *, #46223, .T. ) ;
#25703 = FACE_BOUND ( 'NONE', #24192, .T. ) ;
#25704 = VERTEX_POINT ( 'NONE', #38182 ) ;
#25705 = ORIENTED_EDGE ( 'NONE', *, *, #21373, .F. ) ;
#25706 = DIRECTION ( 'NONE',  ( 0.000000000000000000, 0.8229838658936633466, 0.5680647467311457088 ) ) ;
#25707 = CIRCLE ( 'NONE', #34916, 125.0000000000000000 ) ;
#25708 = LINE ( 'NONE', #4848, #7945 ) ;
#25709 = AXIS2_PLACEMENT_3D ( 'NONE', #4637, #20403, #36702 ) ;
#25710 = CARTESIAN_POINT ( 'NONE',  ( -336.3521761649653854, -181.3443148879387081, 15.93848283698911317 ) ) ;
#25711 = ORIENTED_EDGE ( 'NONE', *, *, #25078, .T. ) ;
#25712 = CARTESIAN_POINT ( 'NONE',  ( 46.40005841627163363, -183.6283474603465606, 81.38144888055276738 ) ) ;
#25713 = LINE ( 'NONE', #25459, #6287 ) ;
#25714 = AXIS2_PLACEMENT_3D ( 'NONE', #27317, #6074, #46973 ) ;
#25715 = EDGE_CURVE ( 'NONE', #10873, #76, #1936, .T. ) ;
#25716 = ADVANCED_FACE ( 'NONE', ( #5896 ), #17975, .T. ) ;
#25717 = CYLINDRICAL_SURFACE ( 'NONE', #27132, 124.9999999999999858 ) ;
#25718 = CARTESIAN_POINT ( 'NONE',  ( -127.4665351220365892, -193.5000000000000000, -96.88131563365291754 ) ) ;
#25719 = EDGE_LOOP ( 'NONE', ( #1744, #16059, #19588, #35067 ) ) ;
#25720 = DIRECTION ( 'NONE',  ( 0.000000000000000000, 0.9709418174260526779, 0.2393156642875547968 ) ) ;
#25721 = CARTESIAN_POINT ( 'NONE',  ( 49.38443399872257800, 28.88712326890130555, -45.87515662012453532 ) ) ;
#25722 = EDGE_CURVE ( 'NONE', #38994, #3778, #42902, .T. ) ;
#25723 = EDGE_CURVE ( 'NONE', #25303, #4861, #26056, .T. ) ;
#25724 = LINE ( 'NONE', #37559, #34130 ) ;
#25725 = ORIENTED_EDGE ( 'NONE', *, *, #20026, .F. ) ;
#25726 = AXIS2_PLACEMENT_3D ( 'NONE', #17178, #21111, #49243 ) ;
#25727 = AXIS2_PLACEMENT_3D ( 'NONE', #37336, #6071, #49458 ) ;
#25728 = AXIS2_PLACEMENT_3D ( 'NONE', #44766, #4830, #7971 ) ;
#25729 = CIRCLE ( 'NONE', #3061, 125.0000000000000000 ) ;
#25730 = FACE_BOUND ( 'NONE', #44458, .T. ) ;
#25731 = LINE ( 'NONE', #17599, #28638 ) ;
#25732 = VERTEX_POINT ( 'NONE', #33985 ) ;
#25733 = CARTESIAN_POINT ( 'NONE',  ( -48.93575598890255662, -193.5000000000000000, -0.8896570909947461026 ) ) ;
#25734 = AXIS2_PLACEMENT_3D ( 'NONE', #51672, #11190, #3565 ) ;
#25735 = ORIENTED_EDGE ( 'NONE', *, *, #31115, .F. ) ;
#25736 = AXIS2_PLACEMENT_3D ( 'NONE', #23443, #30285, #42883 ) ;
#25737 = CARTESIAN_POINT ( 'NONE',  ( -339.1964088526558498, -89.00580675195338642, -49.09328500076576773 ) ) ;
#25738 = AXIS2_PLACEMENT_3D ( 'NONE', #4228, #48373, #16589 ) ;
#25739 = DIRECTION ( 'NONE',  ( 0.000000000000000000, -1.000000000000000000, -0.000000000000000000 ) ) ;
#25740 = PRODUCT_DEFINITION ( 'UNKNOWN', '', #44360, #13804 ) ;
#25741 = DIRECTION ( 'NONE',  ( 1.000000000000000000, -0.000000000000000000, -0.000000000000000000 ) ) ;
#25742 = PLANE ( 'NONE',  #45954 ) ;
#25743 = DIRECTION ( 'NONE',  ( 0.2348860457809707758, 0.000000000000000000, 0.9720229140804138579 ) ) ;
#25744 = VERTEX_POINT ( 'NONE', #26869 ) ;
#25745 = EDGE_CURVE ( 'NONE', #33552, #16495, #50034, .T. ) ;
#25746 = LINE ( 'NONE', #17529, #47485 ) ;
#25747 = EDGE_LOOP ( 'NONE', ( #38561, #11788, #25811, #11335 ) ) ;
#25748 = DIRECTION ( 'NONE',  ( 0.000000000000000000, 0.000000000000000000, 1.000000000000000000 ) ) ;
#25749 = VECTOR ( 'NONE', #51019, 1000.000000000000000 ) ;
#25750 = VECTOR ( 'NONE', #42657, 1000.000000000000227 ) ;
#25751 = ORIENTED_EDGE ( 'NONE', *, *, #41069, .T. ) ;
#25752 = CARTESIAN_POINT ( 'NONE',  ( -70.75782287548091176, -193.5000000000000000, 122.9986166548864901 ) ) ;
#25753 = VECTOR ( 'NONE', #9517, 1000.000000000000114 ) ;
#25754 = ORIENTED_EDGE ( 'NONE', *, *, #31760, .T. ) ;
#25755 = CARTESIAN_POINT ( 'NONE',  ( -332.3517673607765914, -165.9166037625627439, 41.09453333279358134 ) ) ;
#25756 = CARTESIAN_POINT ( 'NONE',  ( -95.72791768350683128, -183.6283474603465606, -115.7261930397105232 ) ) ;
#25757 = ORIENTED_EDGE ( 'NONE', *, *, #25840, .T. ) ;
#25760 = ORIENTED_EDGE ( 'NONE', *, *, #50363, .T. ) ;
#25759 = FACE_OUTER_BOUND ( 'NONE', #25395, .T. ) ;
#25758 = CARTESIAN_POINT ( 'NONE',  ( -1.985634459154583364, 57.70970895460362726, -16.62426742705180871 ) ) ;
#25761 = AXIS2_PLACEMENT_3D ( 'NONE', #46794, #38377, #38630 ) ;
#25762 = AXIS2_PLACEMENT_3D ( 'NONE', #46328, #10314, #22145 ) ;
#25763 = CARTESIAN_POINT ( 'NONE',  ( 45.36094686508022988, -183.6283474603465606, -82.57748230379237953 ) ) ;
#25765 = ORIENTED_EDGE ( 'NONE', *, *, #8061, .T. ) ;
#25764 = AXIS2_PLACEMENT_3D ( 'NONE', #18736, #2182, #38445 ) ;
#25766 = DIRECTION ( 'NONE',  ( -0.9890401873221654760, 0.000000000000000000, 0.1476465640024710868 ) ) ;
#25767 = VERTEX_POINT ( 'NONE', #30051 ) ;
#25768 = LINE ( 'NONE', #49686, #17533 ) ;
#25771 = ORIENTED_EDGE ( 'NONE', *, *, #45474, .T. ) ;
#25770 = DIRECTION ( 'NONE',  ( 0.000000000000000000, 1.000000000000000000, 0.000000000000000000 ) ) ;
#25769 = DIRECTION ( 'NONE',  ( -0.000000000000000000, -0.9350162426854121689, 0.3546048870425426158 ) ) ;
#25772 = ORIENTED_EDGE ( 'NONE', *, *, #35486, .F. ) ;
#25773 = AXIS2_PLACEMENT_3D ( 'NONE', #17639, #41264, #12892 ) ;
#25774 = LINE ( 'NONE', #1846, #34091 ) ;
#25775 = PLANE ( 'NONE',  #18631 ) ;
#25776 = DIRECTION ( 'NONE',  ( 0.000000000000000000, 6.938893903907222461E-16, 1.000000000000000000 ) ) ;
#25777 = ORIENTED_EDGE ( 'NONE', *, *, #18250, .F. ) ;
#25778 = PLANE ( 'NONE',  #23298 ) ;
#25779 = DIRECTION ( 'NONE',  ( -0.000000000000000000, 1.000000000000000000, -0.000000000000000000 ) ) ;
#25780 = DIRECTION ( 'NONE',  ( 1.043714542225393381E-14, 0.5680647467311457088, -0.8229838658936634577 ) ) ;
#25781 = CARTESIAN_POINT ( 'NONE',  ( -37.08895481556041318, -193.5000000000000000, 124.4799742258550310 ) ) ;
#25782 = ORIENTED_EDGE ( 'NONE', *, *, #31710, .T. ) ;
#25783 = EDGE_CURVE ( 'NONE', #7329, #22006, #10084, .T. ) ;
#25784 = LINE ( 'NONE', #14226, #48979 ) ;
#25785 = CARTESIAN_POINT ( 'NONE',  ( -172.2804936848317823, -183.6283474603465606, -7.024906801078577345 ) ) ;
#25786 = DIRECTION ( 'NONE',  ( 0.000000000000000000, -0.7485107481710934207, 0.6631226582408039638 ) ) ;
#25787 = EDGE_LOOP ( 'NONE', ( #21027, #33697, #46677, #5058 ) ) ;
#25788 = VECTOR ( 'NONE', #5026, 1000.000000000000000 ) ;
#25789 = VECTOR ( 'NONE', #16036, 1000.000000000000114 ) ;
#25790 = DIRECTION ( 'NONE',  ( 0.000000000000000000, 1.000000000000000000, 0.000000000000000000 ) ) ;
#25791 = LINE ( 'NONE', #2642, #30291 ) ;
#25792 = AXIS2_PLACEMENT_3D ( 'NONE', #28629, #1036, #45220 ) ;
#25793 = DIRECTION ( 'NONE',  ( 0.000000000000000000, -1.000000000000000000, 0.000000000000000000 ) ) ;
#25794 = CARTESIAN_POINT ( 'NONE',  ( -336.3521761649654422, -123.5000000000000284, 0.000000000000000000 ) ) ;
#25795 = DIRECTION ( 'NONE',  ( 0.000000000000000000, 0.6631226582407989678, 0.7485107481710977506 ) ) ;
#25796 = VECTOR ( 'NONE', #36604, 999.9999999999998863 ) ;
#25797 = AXIS2_PLACEMENT_3D ( 'NONE', #29746, #18456, #29486 ) ;
#25798 = LINE ( 'NONE', #42076, #47153 ) ;
#25799 = EDGE_CURVE ( 'NONE', #31054, #28133, #38698, .T. ) ;
#25800 = DIRECTION ( 'NONE',  ( -0.6068001458186002006, 0.000000000000000000, 0.7948544414133481562 ) ) ;
#25802 = ORIENTED_EDGE ( 'NONE', *, *, #31001, .F. ) ;
#25801 = DIRECTION ( 'NONE',  ( 0.7175072570443249420, 0.000000000000000000, 0.6965510290630033685 ) ) ;
#25803 = VECTOR ( 'NONE', #46454, 1000.000000000000000 ) ;
#25804 = ORIENTED_EDGE ( 'NONE', *, *, #447, .F. ) ;
#25805 = DIRECTION ( 'NONE',  ( 0.000000000000000000, 0.000000000000000000, 1.000000000000000000 ) ) ;
#25806 = AXIS2_PLACEMENT_3D ( 'NONE', #24736, #40749, #293 ) ;
#25807 = DIRECTION ( 'NONE',  ( -0.9564009842765223146, 0.000000000000000000, -0.2920567706369764371 ) ) ;
#25809 = ORIENTED_EDGE ( 'NONE', *, *, #38153, .T. ) ;
#25808 = PLANE ( 'NONE',  #6052 ) ;
#25810 = ORIENTED_EDGE ( 'NONE', *, *, #11482, .T. ) ;
#25811 = ORIENTED_EDGE ( 'NONE', *, *, #40118, .F. ) ;
#25812 = LINE ( 'NONE', #49991, #32573 ) ;
#25813 = ADVANCED_FACE ( 'NONE', ( #34755 ), #50808, .T. ) ;
#25814 = DIRECTION ( 'NONE',  ( 0.000000000000000000, 1.323015771011644961E-13, 1.000000000000000000 ) ) ;
#25815 = LINE ( 'NONE', #21623, #38098 ) ;
#25816 = ORIENTED_EDGE ( 'NONE', *, *, #10936, .F. ) ;
#25817 = DIRECTION ( 'NONE',  ( -0.000000000000000000, -1.000000000000000000, 0.000000000000000000 ) ) ;
#25818 = AXIS2_PLACEMENT_3D ( 'NONE', #45876, #21429, #49038 ) ;
#25820 = ORIENTED_EDGE ( 'NONE', *, *, #30302, .F. ) ;
#25819 = DIRECTION ( 'NONE',  ( 1.000000000000000000, 0.000000000000000000, -0.000000000000000000 ) ) ;
#25821 = VECTOR ( 'NONE', #29378, 1000.000000000000227 ) ;
#25822 = CARTESIAN_POINT ( 'NONE',  ( -43.48323084606168720, -193.5000000000000000, 123.9001241957026167 ) ) ;
#25823 = ORIENTED_EDGE ( 'NONE', *, *, #3326, .T. ) ;
#25824 = CARTESIAN_POINT ( 'NONE',  ( -173.3968853974275817, -189.7472609257535510, 4.533605064404221174 ) ) ;
#25825 = VECTOR ( 'NONE', #24500, 1000.000000000000000 ) ;
#25826 = ORIENTED_EDGE ( 'NONE', *, *, #32288, .F. ) ;
#25827 = DIRECTION ( 'NONE',  ( 0.000000000000000000, -0.000000000000000000, 1.000000000000000000 ) ) ;
#25828 = LINE ( 'NONE', #33959, #14563 ) ;
#25829 = CARTESIAN_POINT ( 'NONE',  ( 15.80042947435468470, -189.7472609257535510, 107.2060569716377927 ) ) ;
#25830 = EDGE_CURVE ( 'NONE', #47918, #16064, #35283, .T. ) ;
#25831 = ORIENTED_EDGE ( 'NONE', *, *, #9165, .T. ) ;
#25832 = CIRCLE ( 'NONE', #3176, 11.92076361695220932 ) ;
#25833 = ORIENTED_EDGE ( 'NONE', *, *, #45658, .F. ) ;
#25834 = DIRECTION ( 'NONE',  ( 0.000000000000000000, -0.000000000000000000, -1.000000000000000000 ) ) ;
#25835 = DIRECTION ( 'NONE',  ( 0.000000000000000000, -0.6631226582407989678, -0.7485107481710977506 ) ) ;
#25836 = ORIENTED_EDGE ( 'NONE', *, *, #37765, .T. ) ;
#25837 = PLANE ( 'NONE',  #14938 ) ;
#25838 = AXIS2_PLACEMENT_3D ( 'NONE', #8498, #21646, #9548 ) ;
#25839 = ORIENTED_EDGE ( 'NONE', *, *, #11468, .F. ) ;
#25840 = EDGE_CURVE ( 'NONE', #32508, #27501, #7600, .T. ) ;
#25841 = LINE ( 'NONE', #14019, #41001 ) ;
#25842 = EDGE_CURVE ( 'NONE', #25744, #22228, #47895, .T. ) ;
#25843 = DIRECTION ( 'NONE',  ( 0.000000000000000000, -0.8854560256532157947, -0.4647231720437573488 ) ) ;
#25844 = CIRCLE ( 'NONE', #5716, 20.00000000000000000 ) ;
#25845 = ORIENTED_EDGE ( 'NONE', *, *, #16012, .T. ) ;
#25846 = CARTESIAN_POINT ( 'NONE',  ( -332.3517673607765914, -72.48138011061176655, -29.74944317415788930 ) ) ;
#25847 = ORIENTED_EDGE ( 'NONE', *, *, #32040, .T. ) ;
#25848 = ADVANCED_FACE ( 'NONE', ( #24236 ), #43684, .T. ) ;
#25849 = PLANE ( 'NONE',  #1915 ) ;
#25850 = LINE ( 'NONE', #41877, #15549 ) ;
#25851 = LINE ( 'NONE', #18229, #36137 ) ;
#25852 = ORIENTED_EDGE ( 'NONE', *, *, #36588, .F. ) ;
#25853 = LINE ( 'NONE', #41882, #6423 ) ;
#25854 = DIRECTION ( 'NONE',  ( -0.000000000000000000, -1.000000000000000000, 0.000000000000000000 ) ) ;
#25855 = DIRECTION ( 'NONE',  ( 0.000000000000000000, 0.000000000000000000, 1.000000000000000000 ) ) ;
#25856 = CARTESIAN_POINT ( 'NONE',  ( -170.8336150310145172, -175.3837268820161057, 25.58083653558494674 ) ) ;
#25857 = ORIENTED_EDGE ( 'NONE', *, *, #42697, .F. ) ;
#25858 = FACE_OUTER_BOUND ( 'NONE', #12579, .T. ) ;
#25859 = VERTEX_POINT ( 'NONE', #39717 ) ;
#25860 = VECTOR ( 'NONE', #23328, 1000.000000000000000 ) ;
#25861 = ADVANCED_FACE ( 'NONE', ( #15316 ), #27127, .F. ) ;
#25862 = DIRECTION ( 'NONE',  ( -0.000000000000000000, 1.000000000000000000, -0.000000000000000000 ) ) ;
#25864 = ORIENTED_EDGE ( 'NONE', *, *, #31877, .F. ) ;
#25863 = LINE ( 'NONE', #13776, #20284 ) ;
#25865 = AXIS2_PLACEMENT_3D ( 'NONE', #38206, #51871, #72 ) ;
#25866 = ORIENTED_EDGE ( 'NONE', *, *, #19784, .F. ) ;
#25867 = CARTESIAN_POINT ( 'NONE',  ( 141.7825277784304205, -213.5000000000000000, -41.45482488023466061 ) ) ;
#25868 = VECTOR ( 'NONE', #1044, 1000.000000000000227 ) ;
#25869 = VERTEX_POINT ( 'NONE', #43439 ) ;
#25870 = DIRECTION ( 'NONE',  ( -0.000000000000000000, 1.000000000000000000, -0.000000000000000000 ) ) ;
#25871 = ORIENTED_EDGE ( 'NONE', *, *, #23448, .F. ) ;
#25872 = LINE ( 'NONE', #2480, #35880 ) ;
#25873 = PLANE ( 'NONE',  #12416 ) ;
#25874 = PLANE ( 'NONE',  #39492 ) ;
#25875 = PLANE ( 'NONE',  #33304 ) ;
#25876 = VERTEX_POINT ( 'NONE', #55 ) ;
#25877 = ORIENTED_EDGE ( 'NONE', *, *, #7275, .T. ) ;
#25878 = EDGE_LOOP ( 'NONE', ( #35461, #3103, #15309, #28443 ) ) ;
#25879 = AXIS2_PLACEMENT_3D ( 'NONE', #4183, #41202, #28593 ) ;
#25880 = CARTESIAN_POINT ( 'NONE',  ( -330.4913330509368166, -89.57268800991514013, -48.27201571436026484 ) ) ;
#25881 = CARTESIAN_POINT ( 'NONE',  ( -14.28570516517293676, -177.1207230881787780, 120.2323164553486663 ) ) ;
#25882 = CARTESIAN_POINT ( 'NONE',  ( 36.10886851198521441, -193.5000000000000000, 92.03190238880813467 ) ) ;
#25883 = CARTESIAN_POINT ( 'NONE',  ( -12.76653800058364574, -193.5000000000000000, -119.7898618611244927 ) ) ;
#25884 = ORIENTED_EDGE ( 'NONE', *, *, #47801, .T. ) ;
#25885 = EDGE_CURVE ( 'NONE', #40042, #34277, #40244, .T. ) ;
#25886 = EDGE_CURVE ( 'NONE', #4967, #3140, #11629, .T. ) ;
#25887 = ORIENTED_EDGE ( 'NONE', *, *, #20635, .F. ) ;
#25889 = ORIENTED_EDGE ( 'NONE', *, *, #35313, .T. ) ;
#25888 = LINE ( 'NONE', #33255, #10527 ) ;
#25890 = PRODUCT_DEFINITION_FORMATION_WITH_SPECIFIED_SOURCE ( 'ANY', '', #5888, .NOT_KNOWN. ) ;
#25891 = EDGE_LOOP ( 'NONE', ( #48881, #7383, #27664, #34928 ) ) ;
#25892 = AXIS2_PLACEMENT_3D ( 'NONE', #35580, #20594, #36629 ) ;
#25894 = VECTOR ( 'NONE', #45416, 1000.000000000000000 ) ;
#25893 = DIRECTION ( 'NONE',  ( 0.000000000000000000, 0.000000000000000000, -1.000000000000000000 ) ) ;
#25895 = DIRECTION ( 'NONE',  ( -0.000000000000000000, -1.000000000000000000, -0.000000000000000000 ) ) ;
#25896 = VECTOR ( 'NONE', #40462, 1000.000000000000114 ) ;
#25897 = DIRECTION ( 'NONE',  ( -0.000000000000000000, 0.8229838658936556861, -0.5680647467311569221 ) ) ;
#25898 = PLANE ( 'NONE',  #40198 ) ;
#25899 = ORIENTED_EDGE ( 'NONE', *, *, #52010, .F. ) ;
#25900 = ADVANCED_FACE ( 'NONE', ( #36056 ), #39227, .F. ) ;
#25901 = DIRECTION ( 'NONE',  ( 0.000000000000000000, 0.000000000000000000, -1.000000000000000000 ) ) ;
#25902 = ORIENTED_EDGE ( 'NONE', *, *, #33047, .T. ) ;
#25903 = ADVANCED_FACE ( 'NONE', ( #51572 ), #48153, .T. ) ;
#25904 = ORIENTED_EDGE ( 'NONE', *, *, #51631, .F. ) ;
#25905 = PLANE ( 'NONE',  #16194 ) ;
#25906 = AXIS2_PLACEMENT_3D ( 'NONE', #47794, #40150, #11767 ) ;
#25907 = ADVANCED_FACE ( 'NONE', ( #35278 ), #15576, .T. ) ;
#25908 = LINE ( 'NONE', #41932, #25310 ) ;
#25909 = ORIENTED_EDGE ( 'NONE', *, *, #330, .T. ) ;
#25910 = EDGE_CURVE ( 'NONE', #23459, #34925, #11355, .T. ) ;
#25911 = DIRECTION ( 'NONE',  ( 0.000000000000000000, 0.000000000000000000, -1.000000000000000000 ) ) ;
#25912 = LINE ( 'NONE', #25645, #34747 ) ;
#25913 = CARTESIAN_POINT ( 'NONE',  ( -48.18706998087188254, -189.7472609257535510, 0.9564009842765313074 ) ) ;
#25914 = PLANE ( 'NONE',  #49236 ) ;
#25915 = CARTESIAN_POINT ( 'NONE',  ( 70.68712318874649725, -183.6283474603465606, -37.74128873232327663 ) ) ;
#25916 = CARTESIAN_POINT ( 'NONE',  ( -48.47912675150885065, -193.5000000000000000, 6.938893903907228378E-15 ) ) ;
#25917 = VERTEX_POINT ( 'NONE', #19758 ) ;
#25918 = CARTESIAN_POINT ( 'NONE',  ( -332.3517673607765914, -180.3949349376675855, 15.70448169564087770 ) ) ;
#25919 = ORIENTED_EDGE ( 'NONE', *, *, #43281, .T. ) ;
#25920 = VERTEX_POINT ( 'NONE', #7441 ) ;
#25921 = CARTESIAN_POINT ( 'NONE',  ( -48.47912675150885065, -175.3837268820161057, 6.938893903907228378E-15 ) ) ;
#25922 = ORIENTED_EDGE ( 'NONE', *, *, #30251, .F. ) ;
#25923 = DIRECTION ( 'NONE',  ( 0.000000000000000000, 0.000000000000000000, 1.000000000000000000 ) ) ;
#25924 = AXIS2_PLACEMENT_3D ( 'NONE', #4467, #28622, #5001 ) ;
#25925 = DIRECTION ( 'NONE',  ( -0.000000000000000000, 1.000000000000000000, -0.000000000000000000 ) ) ;
#25927 = VERTEX_POINT ( 'NONE', #39472 ) ;
#25926 = CARTESIAN_POINT ( 'NONE',  ( -162.7543581613524282, -177.1207230881787780, 50.65739320402010293 ) ) ;
#25928 = VECTOR ( 'NONE', #20972, 1000.000000000000000 ) ;
#25929 = CARTESIAN_POINT ( 'NONE',  ( 75.48400724637754422, -193.5000000000000000, -16.06677968424457248 ) ) ;
#25930 = DIRECTION ( 'NONE',  ( 0.000000000000000000, 1.000000000000000000, -0.000000000000000000 ) ) ;
#25931 = ORIENTED_EDGE ( 'NONE', *, *, #32725, .F. ) ;
#25932 = ORIENTED_EDGE ( 'NONE', *, *, #49816, .T. ) ;
#25933 = ORIENTED_EDGE ( 'NONE', *, *, #33376, .F. ) ;
#25934 = DIRECTION ( 'NONE',  ( 0.000000000000000000, 1.000000000000000000, 0.000000000000000000 ) ) ;
#25935 = VECTOR ( 'NONE', #17277, 1000.000000000000000 ) ;
#25936 = CARTESIAN_POINT ( 'NONE',  ( -330.4913330509368166, -79.00630452878421295, 38.74998146212088557 ) ) ;
#25937 = ADVANCED_FACE ( 'NONE', ( #35792 ), #7683, .T. ) ;
#25938 = PLANE ( 'NONE',  #28465 ) ;
#25939 = DIRECTION ( 'NONE',  ( 0.000000000000000000, 1.000000000000000000, -0.000000000000000000 ) ) ;
#25940 = CARTESIAN_POINT ( 'NONE',  ( -339.1964088526558498, -124.0000000000002700, -59.00000000000002132 ) ) ;
#25941 = EDGE_LOOP ( 'NONE', ( #22602, #8980, #23127, #17112 ) ) ;
#25942 = EDGE_CURVE ( 'NONE', #51701, #48674, #35525, .T. ) ;
#25943 = EDGE_CURVE ( 'NONE', #37599, #21989, #47862, .T. ) ;
#25944 = EDGE_CURVE ( 'NONE', #4655, #16559, #20029, .T. ) ;
#25945 = EDGE_CURVE ( 'NONE', #15564, #30781, #22691, .T. ) ;
#25946 = VECTOR ( 'NONE', #6714, 1000.000000000000000 ) ;
#25947 = CARTESIAN_POINT ( 'NONE',  ( -91.81555821786916738, -175.3837268820161057, 116.1806952091180563 ) ) ;
#25948 = EDGE_LOOP ( 'NONE', ( #17823, #47497, #24800, #84 ) ) ;
#25950 = ORIENTED_EDGE ( 'NONE', *, *, #4612, .F. ) ;
#25949 = PLANE ( 'NONE',  #29801 ) ;
#25951 = VERTEX_POINT ( 'NONE', #4260 ) ;
#25952 = EDGE_CURVE ( 'NONE', #24959, #25744, #20281, .T. ) ;
#25953 = ORIENTED_EDGE ( 'NONE', *, *, #32127, .F. ) ;
#25954 = LINE ( 'NONE', #10703, #36719 ) ;
#25955 = CARTESIAN_POINT ( 'NONE',  ( -37.14819544345410662, -183.6283474603465606, 123.4817304940907263 ) ) ;
#25956 = EDGE_LOOP ( 'NONE', ( #7557, #50882, #41650, #45332 ) ) ;
#25957 = CYLINDRICAL_SURFACE ( 'NONE', #22961, 125.0000000000000000 ) ;
#25958 = DIRECTION ( 'NONE',  ( 1.000000000000000000, -0.000000000000000000, -0.000000000000000000 ) ) ;
#25959 = ORIENTED_EDGE ( 'NONE', *, *, #23584, .F. ) ;
#25960 = EDGE_CURVE ( 'NONE', #3648, #17251, #37087, .T. ) ;
#25961 = DIRECTION ( 'NONE',  ( 0.000000000000000000, 0.000000000000000000, -1.000000000000000000 ) ) ;
#25962 = EDGE_LOOP ( 'NONE', ( #12236, #6693, #31388, #49648 ) ) ;
#25963 = EDGE_CURVE ( 'NONE', #20384, #51691, #13192, .T. ) ;
#25964 = EDGE_LOOP ( 'NONE', ( #47451, #22936, #42383, #42419 ) ) ;
#25965 = LINE ( 'NONE', #18849, #43823 ) ;
#25966 = LINE ( 'NONE', #30417, #44922 ) ;
#25967 = EDGE_CURVE ( 'NONE', #18737, #9242, #25024, .T. ) ;
#25968 = VECTOR ( 'NONE', #50118, 1000.000000000000000 ) ;
#25969 = CARTESIAN_POINT ( 'NONE',  ( -148.0127667507368585, -177.1207230881787780, -75.61781872352626976 ) ) ;
#25970 = CARTESIAN_POINT ( 'NONE',  ( -339.1964088526558498, -172.3400804610915600, -33.10432812419107051 ) ) ;
#25971 = VERTEX_POINT ( 'NONE', #40504 ) ;
#25972 = DIRECTION ( 'NONE',  ( -0.6300878435817203194, 0.000000000000000000, 0.7765238627180349740 ) ) ;
#25973 = DIRECTION ( 'NONE',  ( -0.000000000000000000, 1.000000000000000000, -0.000000000000000000 ) ) ;
#25974 = EDGE_CURVE ( 'NONE', #186, #40642, #28937, .T. ) ;
#25975 = DIRECTION ( 'NONE',  ( -1.000000000000000000, -0.000000000000000000, -0.000000000000000000 ) ) ;
#25976 = CARTESIAN_POINT ( 'NONE',  ( -339.1964088526558498, -180.6659093959934523, -14.60509510167853264 ) ) ;
#25977 = VERTEX_POINT ( 'NONE', #1087 ) ;
#25978 = PLANE ( 'NONE',  #36393 ) ;
#25979 = DIRECTION ( 'NONE',  ( 0.000000000000000000, 1.000000000000000000, 0.000000000000000000 ) ) ;
#25980 = EDGE_CURVE ( 'NONE', #34528, #47296, #44998, .T. ) ;
#25981 = DIRECTION ( 'NONE',  ( 0.9785564922995046988, 0.000000000000000000, -0.2059786187410953262 ) ) ;
#25982 = EDGE_LOOP ( 'NONE', ( #8810, #31992, #24617, #10095 ) ) ;
#25983 = FACE_OUTER_BOUND ( 'NONE', #45527, .T. ) ;
#25984 = DIRECTION ( 'NONE',  ( 1.000000000000000000, -0.000000000000000000, -0.000000000000000000 ) ) ;
#25985 = DIRECTION ( 'NONE',  ( 0.000000000000000000, 1.000000000000000000, 0.000000000000000000 ) ) ;
#25986 = ORIENTED_EDGE ( 'NONE', *, *, #2663, .T. ) ;
#25987 = DIRECTION ( 'NONE',  ( -0.000000000000000000, -1.000000000000000000, 0.000000000000000000 ) ) ;
#25988 = ORIENTED_EDGE ( 'NONE', *, *, #27237, .F. ) ;
#25989 = ADVANCED_FACE ( 'NONE', ( #44468 ), #41287, .T. ) ;
#25990 = VECTOR ( 'NONE', #44819, 1000.000000000000000 ) ;
#25991 =( REPRESENTATION_RELATIONSHIP ('NONE','NONE', #4578, #15324 ) REPRESENTATION_RELATIONSHIP_WITH_TRANSFORMATION ( #41474 )SHAPE_REPRESENTATION_RELATIONSHIP( ) );
#25992 = DIRECTION ( 'NONE',  ( 1.000000000000000000, -0.000000000000000000, -0.000000000000000000 ) ) ;
#25993 = PLANE ( 'NONE',  #32907 ) ;
#25994 = CARTESIAN_POINT ( 'NONE',  ( -169.9131040279660283, -177.1207230881787780, 29.64437826672835996 ) ) ;
#25995 = CARTESIAN_POINT ( 'NONE',  ( -339.1964088526558498, -150.4759391377552618, 52.47426709956155122 ) ) ;
#25996 = CARTESIAN_POINT ( 'NONE',  ( -339.1964088526558498, -71.49045607248255862, -27.86139516340906397 ) ) ;
#25997 = ORIENTED_EDGE ( 'NONE', *, *, #43094, .T. ) ;
#25998 = CARTESIAN_POINT ( 'NONE',  ( -339.1964088526558498, -84.00150778970699150, 43.83057281297409702 ) ) ;
#25999 = EDGE_LOOP ( 'NONE', ( #38219, #8120, #32700, #5276 ) ) ;
#26000 = EDGE_CURVE ( 'NONE', #12871, #25410, #32880, .T. ) ;
#26001 = PLANE ( 'NONE',  #25054 ) ;
#26002 = AXIS2_PLACEMENT_3D ( 'NONE', #9713, #34402, #50446 ) ;
#26003 = ORIENTED_EDGE ( 'NONE', *, *, #8520, .F. ) ;
#26004 = DIRECTION ( 'NONE',  ( -0.000000000000000000, 1.000000000000000000, -0.000000000000000000 ) ) ;
#26005 = EDGE_CURVE ( 'NONE', #22651, #19986, #28673, .T. ) ;
#26006 = ADVANCED_FACE ( 'NONE', ( #21067 ), #17137, .T. ) ;
#26007 = ADVANCED_FACE ( 'NONE', ( #36570 ), #13448, .F. ) ;
#26008 = ADVANCED_FACE ( 'NONE', ( #9254 ), #16349, .T. ) ;
#26009 = DIRECTION ( 'NONE',  ( 0.000000000000000000, -1.000000000000000000, 0.000000000000000000 ) ) ;
#26010 = CARTESIAN_POINT ( 'NONE',  ( -48.47912675150885065, -183.6283474603465606, 6.938893903907228378E-15 ) ) ;
#26011 = ORIENTED_EDGE ( 'NONE', *, *, #40464, .T. ) ;
#26014 = ORIENTED_EDGE ( 'NONE', *, *, #23924, .T. ) ;
#26013 = DIRECTION ( 'NONE',  ( -0.000000000000000000, 1.000000000000000000, -0.000000000000000000 ) ) ;
#26012 = CARTESIAN_POINT ( 'NONE',  ( -2.954493006721953030, 51.44106513229385769, -20.60687412731818213 ) ) ;
#26015 = PLANE ( 'NONE',  #15566 ) ;
#26016 = ORIENTED_EDGE ( 'NONE', *, *, #33719, .F. ) ;
#26017 = DIRECTION ( 'NONE',  ( 0.9890401873221644768, 0.000000000000000000, -0.1476465640024779702 ) ) ;
#26018 = ORIENTED_EDGE ( 'NONE', *, *, #21961, .T. ) ;
#26019 = LINE ( 'NONE', #2094, #713 ) ;
#26022 = ORIENTED_EDGE ( 'NONE', *, *, #46913, .F. ) ;
#26021 = CARTESIAN_POINT ( 'NONE',  ( -22.44626007086656472, -183.6283474603465606, 122.2591094863196872 ) ) ;
#26020 = DIRECTION ( 'NONE',  ( 0.000000000000000000, 0.000000000000000000, -1.000000000000000000 ) ) ;
#26023 = ORIENTED_EDGE ( 'NONE', *, *, #21957, .T. ) ;
#26024 = AXIS2_PLACEMENT_3D ( 'NONE', #35558, #80, #40268 ) ;
#26025 = AXIS2_PLACEMENT_3D ( 'NONE', #42398, #22694, #42911 ) ;
#26026 = CARTESIAN_POINT ( 'NONE',  ( -339.1964088526558498, -70.60684477890951882, 28.32515014536776832 ) ) ;
#26027 = EDGE_LOOP ( 'NONE', ( #42021, #49572, #21765, #40036 ) ) ;
#26028 = LINE ( 'NONE', #8970, #157 ) ;
#26029 = LINE ( 'NONE', #38372, #36583 ) ;
#26030 = EDGE_CURVE ( 'NONE', #10649, #7481, #23545, .T. ) ;
#26031 = ORIENTED_EDGE ( 'NONE', *, *, #48777, .F. ) ;
#26032 = DIRECTION ( 'NONE',  ( 0.6068001458185945385, 0.000000000000000000, -0.7948544414133523750 ) ) ;
#26033 = CARTESIAN_POINT ( 'NONE',  ( -154.6193097927903182, -189.7472609257535510, -66.02470404298124151 ) ) ;
#26034 = DIRECTION ( 'NONE',  ( 0.000000000000000000, 0.000000000000000000, 1.000000000000000000 ) ) ;
#26035 = LINE ( 'NONE', #42060, #44451 ) ;
#26036 = PLANE ( 'NONE',  #39126 ) ;
#26037 = EDGE_CURVE ( 'NONE', #14521, #3, #26874, .T. ) ;
#26038 = VERTEX_POINT ( 'NONE', #29463 ) ;
#26039 = LINE ( 'NONE', #49704, #46429 ) ;
#26040 = CARTESIAN_POINT ( 'NONE',  ( -339.1964088526558498, -172.5932850007659169, -34.49419324804647147 ) ) ;
#26041 = ADVANCED_FACE ( 'NONE', ( #8454 ), #45513, .F. ) ;
#26042 = CARTESIAN_POINT ( 'NONE',  ( -305.0000000000000568, -107.5615171630107056, 57.84431488793861575 ) ) ;
#26043 = VERTEX_POINT ( 'NONE', #25524 ) ;
#26044 = VECTOR ( 'NONE', #43315, 1000.000000000000000 ) ;
#26045 = DIRECTION ( 'NONE',  ( -0.9027978299657387629, 0.000000000000000000, -0.4300652022765304450 ) ) ;
#26046 = DIRECTION ( 'NONE',  ( 0.000000000000000000, 0.000000000000000000, 1.000000000000000000 ) ) ;
#26047 = DIRECTION ( 'NONE',  ( -0.000000000000000000, 1.000000000000000000, -0.000000000000000000 ) ) ;
#26048 = LINE ( 'NONE', #1088, #19889 ) ;
#26049 = CARTESIAN_POINT ( 'NONE',  ( -48.82732838694325750, -193.5000000000000000, 0.9374196611341252261 ) ) ;
#26050 = CARTESIAN_POINT ( 'NONE',  ( -102.5006284722404502, -193.5000000000000000, -112.7238987608084386 ) ) ;
#26051 = DIRECTION ( 'NONE',  ( 0.000000000000000000, 1.000000000000000000, 0.000000000000000000 ) ) ;
#26052 = LINE ( 'NONE', #42078, #11089 ) ;
#26053 = ORIENTED_EDGE ( 'NONE', *, *, #29452, .F. ) ;
#26054 = CARTESIAN_POINT ( 'NONE',  ( -305.0000000000000568, -83.33976666099019326, -44.57752413667995484 ) ) ;
#26055 = CIRCLE ( 'NONE', #11789, 125.0000000000000000 ) ;
#26056 = CIRCLE ( 'NONE', #45360, 125.0000000000000000 ) ;
#26057 = DIRECTION ( 'NONE',  ( 0.000000000000000000, -1.000000000000000000, -0.000000000000000000 ) ) ;
#26059 = ORIENTED_EDGE ( 'NONE', *, *, #6675, .T. ) ;
#26058 = DIRECTION ( 'NONE',  ( -1.000000000000000000, -1.013386094502322405E-14, 2.497772389992582658E-15 ) ) ;
#26060 = ORIENTED_EDGE ( 'NONE', *, *, #43803, .T. ) ;
#26061 = EDGE_LOOP ( 'NONE', ( #48596, #8531, #6106, #46946 ) ) ;
#26062 = CARTESIAN_POINT ( 'NONE',  ( -171.5592422664403216, -193.5000000000000000, -21.82395850507255730 ) ) ;
#26063 = ADVANCED_FACE ( 'NONE', ( #44727 ), #12395, .F. ) ;
#26064 = ADVANCED_FACE ( 'NONE', ( #4788 ), #20817, .F. ) ;
#26065 = CARTESIAN_POINT ( 'NONE',  ( 24.15597040328003331, -183.6283474603465606, -101.7307360698544159 ) ) ;
#26066 = CARTESIAN_POINT ( 'NONE',  ( 59.80284513346456521, -193.5000000000000000, 62.45009659481583952 ) ) ;
#26067 = VERTEX_POINT ( 'NONE', #1870 ) ;
#26068 = DIRECTION ( 'NONE',  ( 1.000000000000000000, 0.000000000000000000, 0.000000000000000000 ) ) ;
#26069 = LINE ( 'NONE', #26840, #25235 ) ;
#26071 = VERTEX_POINT ( 'NONE', #22364 ) ;
#26070 = DIRECTION ( 'NONE',  ( 0.000000000000000000, 1.000000000000000000, 0.000000000000000000 ) ) ;
#26072 = AXIS2_PLACEMENT_3D ( 'NONE', #30076, #21683, #25112 ) ;
#26073 = CARTESIAN_POINT ( 'NONE',  ( -172.9701362814535912, -175.3837268820161057, -11.26891947860193177 ) ) ;
#26074 = EDGE_LOOP ( 'NONE', ( #2205, #4549, #23725, #21551 ) ) ;
#26075 = DIRECTION ( 'NONE',  ( 1.000000000000000000, 0.000000000000000000, 0.000000000000000000 ) ) ;
#26076 = ORIENTED_EDGE ( 'NONE', *, *, #38827, .T. ) ;
#26077 = LINE ( 'NONE', #14006, #23260 ) ;
#26078 = CARTESIAN_POINT ( 'NONE',  ( 65.79610465833508215, -193.5000000000000000, -50.65739320401928580 ) ) ;
#26079 = CARTESIAN_POINT ( 'NONE',  ( 70.19984492582109681, -175.3837268820161057, 39.24667733211968823 ) ) ;
#26080 = EDGE_LOOP ( 'NONE', ( #27665, #4538, #36920, #18352 ) ) ;
#26081 = VERTEX_POINT ( 'NONE', #2124 ) ;
#26082 = CARTESIAN_POINT ( 'NONE',  ( -164.6246685127424882, -193.5000000000000000, -46.20836643930983456 ) ) ;
#26083 = DIRECTION ( 'NONE',  ( -0.000000000000000000, 1.000000000000000000, 0.000000000000000000 ) ) ;
#26084 = ORIENTED_EDGE ( 'NONE', *, *, #3814, .F. ) ;
#26085 = EDGE_CURVE ( 'NONE', #6100, #9931, #50748, .T. ) ;
#26086 = CARTESIAN_POINT ( 'NONE',  ( 17.44316424268010124, -193.5000000000000000, -105.0256126866231625 ) ) ;
#26087 = AXIS2_PLACEMENT_3D ( 'NONE', #9504, #14232, #26046 ) ;
#26088 = ORIENTED_EDGE ( 'NONE', *, *, #37666, .F. ) ;
#26089 = FACE_BOUND ( 'NONE', #38507, .T. ) ;
#26090 = DIRECTION ( 'NONE',  ( 0.000000000000000000, 0.3546048870425300148, -0.9350162426854169428 ) ) ;
#26091 = ADVANCED_FACE ( 'NONE', ( #17914 ), #46297, .T. ) ;
#26092 = VECTOR ( 'NONE', #21792, 1000.000000000000227 ) ;
#26093 = EDGE_LOOP ( 'NONE', ( #19176, #35622, #27976, #39543 ) ) ;
#26094 = LINE ( 'NONE', #18224, #17382 ) ;
#26095 = ORIENTED_EDGE ( 'NONE', *, *, #51045, .T. ) ;
#26096 = LINE ( 'NONE', #14026, #39011 ) ;
#26097 = CARTESIAN_POINT ( 'NONE',  ( 21.21056010634070432, -189.7472609257535510, 103.7706487676302061 ) ) ;
#26098 = VERTEX_POINT ( 'NONE', #2400 ) ;
#26099 = CARTESIAN_POINT ( 'NONE',  ( 76.51419089073348800, -193.5000000000000000, -1.292495564988658030 ) ) ;
#26100 = PLANE ( 'NONE',  #18847 ) ;
#26101 = FACE_OUTER_BOUND ( 'NONE', #17328, .T. ) ;
#26102 = EDGE_CURVE ( 'NONE', #27341, #7466, #9764, .T. ) ;
#26103 = ORIENTED_EDGE ( 'NONE', *, *, #3406, .F. ) ;
#26104 = LINE ( 'NONE', #6156, #30418 ) ;
#26105 = VERTEX_POINT ( 'NONE', #30499 ) ;
#26106 = AXIS2_PLACEMENT_3D ( 'NONE', #15277, #26833, #46568 ) ;
#26107 = DIRECTION ( 'NONE',  ( 0.000000000000000000, 0.000000000000000000, -1.000000000000000000 ) ) ;
#26108 = DIRECTION ( 'NONE',  ( 0.000000000000000000, 1.000000000000000000, 0.000000000000000000 ) ) ;
#26110 = ORIENTED_EDGE ( 'NONE', *, *, #32534, .F. ) ;
#26109 = DIRECTION ( 'NONE',  ( 0.5085311186492216251, 0.000000000000000000, -0.8610436117673548884 ) ) ;
#26111 = VERTEX_POINT ( 'NONE', #14744 ) ;
#26112 = CARTESIAN_POINT ( 'NONE',  ( -336.3521761649654422, -165.9166037625627439, 41.09453333279358134 ) ) ;
#26113 = EDGE_CURVE ( 'NONE', #39890, #8565, #4226, .T. ) ;
#26114 = CARTESIAN_POINT ( 'NONE',  ( -48.47912675150885065, -189.7472609257535510, 1.000000000000006883 ) ) ;
#26115 = ORIENTED_EDGE ( 'NONE', *, *, #13267, .F. ) ;
#26116 = FACE_OUTER_BOUND ( 'NONE', #39018, .T. ) ;
#26117 = VERTEX_POINT ( 'NONE', #29993 ) ;
#26118 = CARTESIAN_POINT ( 'NONE',  ( 46.00000000000000711, -43.50000000000000000, -46.00000000000000000 ) ) ;
#26119 = CARTESIAN_POINT ( 'NONE',  ( 76.52053249983501360, -183.6283474603465606, -0.2918682030015273265 ) ) ;
#26120 = AXIS2_PLACEMENT_3D ( 'NONE', #26420, #9896, #37992 ) ;
#26121 = EDGE_CURVE ( 'NONE', #32749, #5608, #14233, .T. ) ;
#26122 = DIRECTION ( 'NONE',  ( 0.8294056854502049880, 0.000000000000000000, -0.5586467658036476935 ) ) ;
#26123 = DIRECTION ( 'NONE',  ( 0.000000000000000000, 1.000000000000000000, -0.000000000000000000 ) ) ;
#26124 = ORIENTED_EDGE ( 'NONE', *, *, #34547, .F. ) ;
#26125 = EDGE_LOOP ( 'NONE', ( #30139, #10896, #1734, #51832 ) ) ;
#26127 = ORIENTED_EDGE ( 'NONE', *, *, #42303, .T. ) ;
#26126 = CIRCLE ( 'NONE', #15218, 60.00000000000000000 ) ;
#26128 = CARTESIAN_POINT ( 'NONE',  ( 39.18328161278951427, -175.3837268820161057, 89.10837311819236106 ) ) ;
#26129 = CARTESIAN_POINT ( 'NONE',  ( -47.70260288879080690, -189.7472609257535510, -0.6300878435817026668 ) ) ;
#26130 = EDGE_CURVE ( 'NONE', #19079, #3016, #11757, .T. ) ;
#26131 = CARTESIAN_POINT ( 'NONE',  ( -47.78257572244585560, -175.3837268820161057, -0.7175072570443230546 ) ) ;
#26132 = DIRECTION ( 'NONE',  ( 0.000000000000000000, 0.000000000000000000, 1.000000000000000000 ) ) ;
#26133 = EDGE_LOOP ( 'NONE', ( #25470, #6870, #25593, #51676 ) ) ;
#26134 = DIRECTION ( 'NONE',  ( 0.5829794791144762289, 0.000000000000000000, -0.8124868780056783146 ) ) ;
#26135 = CIRCLE ( 'NONE', #50506, 125.0000000000000000 ) ;
#26136 = EDGE_LOOP ( 'NONE', ( #27414, #551, #50396, #15806 ) ) ;
#26138 = ORIENTED_EDGE ( 'NONE', *, *, #47015, .F. ) ;
#26137 = DIRECTION ( 'NONE',  ( -0.000000000000000000, 1.000000000000000000, -0.000000000000000000 ) ) ;
#26139 = CIRCLE ( 'NONE', #14424, 60.00000000000000000 ) ;
#26140 = CARTESIAN_POINT ( 'NONE',  ( 58.48829670243886625, -193.5000000000000000, -64.67588669375805921 ) ) ;
#26141 = ADVANCED_FACE ( 'NONE', ( #2644 ), #6086, .T. ) ;
#26142 = CARTESIAN_POINT ( 'NONE',  ( -336.3521761649654422, -69.20050475944881896, 25.52576769896172237 ) ) ;
#26143 = PLANE ( 'NONE',  #33794 ) ;
#26144 = DIRECTION ( 'NONE',  ( 1.000000000000000000, -0.000000000000000000, -0.000000000000000000 ) ) ;
#26145 = VERTEX_POINT ( 'NONE', #30761 ) ;
#26146 = PLANE ( 'NONE',  #51092 ) ;
#26147 = ORIENTED_EDGE ( 'NONE', *, *, #47561, .T. ) ;
#26148 = ORIENTED_EDGE ( 'NONE', *, *, #11519, .F. ) ;
#26149 = DIRECTION ( 'NONE',  ( 0.000000000000000000, -0.000000000000000000, 1.000000000000000000 ) ) ;
#26150 = CARTESIAN_POINT ( 'NONE',  ( 32.99469856375239374, -189.7472609257535510, 94.79987230212019256 ) ) ;
#26151 = ORIENTED_EDGE ( 'NONE', *, *, #10877, .F. ) ;
#26152 = AXIS2_PLACEMENT_3D ( 'NONE', #25338, #13256, #29279 ) ;
#26153 = CARTESIAN_POINT ( 'NONE',  ( -180.0000000000000568, -155.0173647354142759, 14.76740078976490622 ) ) ;
#26154 = PLANE ( 'NONE',  #47369 ) ;
#26155 = DIRECTION ( 'NONE',  ( 0.000000000000000000, -1.000000000000000000, 0.000000000000000000 ) ) ;
#26156 = AXIS2_PLACEMENT_3D ( 'NONE', #9886, #6722, #21716 ) ;
#26157 = DIRECTION ( 'NONE',  ( -0.000000000000000000, 1.000000000000000000, 0.000000000000000000 ) ) ;
#26158 = VECTOR ( 'NONE', #46553, 1000.000000000000227 ) ;
#26159 = DIRECTION ( 'NONE',  ( -0.000000000000000000, 1.000000000000000000, 0.000000000000000000 ) ) ;
#26160 = ORIENTED_EDGE ( 'NONE', *, *, #19922, .T. ) ;
#26161 = FACE_OUTER_BOUND ( 'NONE', #38909, .T. ) ;
#26162 = ORIENTED_EDGE ( 'NONE', *, *, #48090, .F. ) ;
#26163 = ADVANCED_FACE ( 'NONE', ( #50494 ), #46545, .T. ) ;
#26164 = ORIENTED_EDGE ( 'NONE', *, *, #1395, .T. ) ;
#26165 = LINE ( 'NONE', #38769, #24609 ) ;
#26166 = EDGE_CURVE ( 'NONE', #32359, #15270, #33923, .T. ) ;
#26167 = ORIENTED_EDGE ( 'NONE', *, *, #46971, .T. ) ;
#26168 = VECTOR ( 'NONE', #8462, 1000.000000000000000 ) ;
#26169 = DIRECTION ( 'NONE',  ( -0.000000000000000000, -0.4647231720437604574, 0.8854560256532141294 ) ) ;
#26170 = VECTOR ( 'NONE', #29475, 1000.000000000000000 ) ;
#26171 = CIRCLE ( 'NONE', #38737, 125.0000000000000000 ) ;
#26172 = FACE_BOUND ( 'NONE', #46638, .T. ) ;
#26173 = CARTESIAN_POINT ( 'NONE',  ( 0.000000000000000000, -96.08133284941705199, 52.24190551353909484 ) ) ;
#26174 = ORIENTED_EDGE ( 'NONE', *, *, #32846, .T. ) ;
#26175 = DIRECTION ( 'NONE',  ( -0.000000000000000000, -0.000000000000000000, -1.000000000000000000 ) ) ;
#26176 = EDGE_CURVE ( 'NONE', #50211, #6218, #21859, .T. ) ;
#26177 = DIRECTION ( 'NONE',  ( 0.4566292373937200777, 0.000000000000000000, -0.8896570909947436601 ) ) ;
#26178 = FACE_OUTER_BOUND ( 'NONE', #42232, .T. ) ;
#26179 = EDGE_LOOP ( 'NONE', ( #30735, #6885, #32467, #12083 ) ) ;
#26180 = ORIENTED_EDGE ( 'NONE', *, *, #31105, .T. ) ;
#26181 = EDGE_CURVE ( 'NONE', #27368, #36071, #26814, .T. ) ;
#26182 = ORIENTED_EDGE ( 'NONE', *, *, #21305, .T. ) ;
#26183 = CARTESIAN_POINT ( 'NONE',  ( 9.518239912201957864, -213.5000000000000000, 110.7307791902283043 ) ) ;
#26184 = DIRECTION ( 'NONE',  ( -0.000000000000000000, 1.000000000000000000, -0.000000000000000000 ) ) ;
#26185 = ADVANCED_FACE ( 'NONE', ( #30252 ), #10277, .T. ) ;
#26186 = EDGE_CURVE ( 'NONE', #7641, #38149, #20206, .T. ) ;
#26187 = CARTESIAN_POINT ( 'NONE',  ( -330.4913330509368166, -102.1108035431471279, 54.98865587491800255 ) ) ;
#26188 = DIRECTION ( 'NONE',  ( -0.3482016354344059095, 0.000000000000000000, 0.9374196611341183427 ) ) ;
#26189 = DIRECTION ( 'NONE',  ( 0.000000000000000000, -1.000000000000000000, -0.000000000000000000 ) ) ;
#26190 = AXIS2_PLACEMENT_3D ( 'NONE', #5760, #9173, #41467 ) ;
#26191 = ORIENTED_EDGE ( 'NONE', *, *, #45245, .F. ) ;
#26192 = CIRCLE ( 'NONE', #48884, 60.00000000000000000 ) ;
#26193 = CYLINDRICAL_SURFACE ( 'NONE', #19001, 125.0000000000000000 ) ;
#26194 = ORIENTED_EDGE ( 'NONE', *, *, #1571, .F. ) ;
#26196 = ORIENTED_EDGE ( 'NONE', *, *, #24433, .T. ) ;
#26195 = DIRECTION ( 'NONE',  ( 0.000000000000000000, -1.000000000000000000, 0.000000000000000000 ) ) ;
#26197 = ORIENTED_EDGE ( 'NONE', *, *, #27386, .T. ) ;
#26198 = DIRECTION ( 'NONE',  ( 0.000000000000000000, 1.156482317317871232E-16, 1.000000000000000000 ) ) ;
#26199 = ORIENTED_EDGE ( 'NONE', *, *, #2699, .F. ) ;
#26200 = CARTESIAN_POINT ( 'NONE',  ( -19.92568551777506869, -189.7472609257535510, -121.6951149130962904 ) ) ;
#26201 = ORIENTED_EDGE ( 'NONE', *, *, #4550, .F. ) ;
#26202 = DIRECTION ( 'NONE',  ( -0.6068001458186002006, 0.000000000000000000, 0.7948544414133481562 ) ) ;
#26203 = CARTESIAN_POINT ( 'NONE',  ( -47.50057025920934706, -175.3837268820161057, 0.2059786187411091207 ) ) ;
#26204 = EDGE_LOOP ( 'NONE', ( #49611, #33862, #17746, #37945 ) ) ;
#26205 = CARTESIAN_POINT ( 'NONE',  ( -168.1141659785444915, -193.5000000000000000, -36.22785377503943494 ) ) ;
#26206 = ORIENTED_EDGE ( 'NONE', *, *, #45941, .F. ) ;
#26207 = CIRCLE ( 'NONE', #7758, 125.0000000000000000 ) ;
#26208 = CIRCLE ( 'NONE', #20357, 125.0000000000000000 ) ;
#26209 = EDGE_LOOP ( 'NONE', ( #40162, #16119, #24741, #50542 ) ) ;
#26210 = LINE ( 'NONE', #7032, #6924 ) ;
#26211 = AXIS2_PLACEMENT_3D ( 'NONE', #48802, #24357, #953 ) ;
#26213 = AXIS2_PLACEMENT_3D ( 'NONE', #34289, #45355, #9343 ) ;
#26212 = CARTESIAN_POINT ( 'NONE',  ( 73.32083127613157103, -183.6283474603465606, 28.10285082451656535 ) ) ;
#26214 = CARTESIAN_POINT ( 'NONE',  ( 0.000000000000000000, -144.4216883355091170, 55.16595831843969933 ) ) ;
#26215 = EDGE_LOOP ( 'NONE', ( #23557, #36469, #11309, #24009 ) ) ;
#26216 = DIRECTION ( 'NONE',  ( -1.000000000000000000, 0.000000000000000000, 0.000000000000000000 ) ) ;
#26217 = CARTESIAN_POINT ( 'NONE',  ( -172.4422607493951318, -193.5000000000000000, 16.06677968424543579 ) ) ;
#26218 = CARTESIAN_POINT ( 'NONE',  ( 24.15597040328006884, -177.1207230881787780, -101.7307360698544016 ) ) ;
#26219 = DIRECTION ( 'NONE',  ( -0.000000000000000000, 1.000000000000000000, -0.000000000000000000 ) ) ;
#26220 = ORIENTED_EDGE ( 'NONE', *, *, #37525, .T. ) ;
#26221 = DIRECTION ( 'NONE',  ( 0.000000000000000000, -0.9350162426854181641, -0.3546048870425267951 ) ) ;
#26222 = DIRECTION ( 'NONE',  ( 0.000000000000000000, 0.000000000000000000, 1.000000000000000000 ) ) ;
#26223 = DIRECTION ( 'NONE',  ( 0.000000000000000000, 0.000000000000000000, -1.000000000000000000 ) ) ;
#26224 = ORIENTED_EDGE ( 'NONE', *, *, #38374, .T. ) ;
#26225 = FACE_OUTER_BOUND ( 'NONE', #5, .T. ) ;
#26226 = AXIS2_PLACEMENT_3D ( 'NONE', #4634, #25140, #20938 ) ;
#26227 = EDGE_CURVE ( 'NONE', #24430, #12390, #38642, .T. ) ;
#26228 = DIRECTION ( 'NONE',  ( 0.000000000000000000, -1.000000000000000000, 0.000000000000000000 ) ) ;
#26229 = EDGE_CURVE ( 'NONE', #28974, #41796, #1627, .T. ) ;
#26230 = ORIENTED_EDGE ( 'NONE', *, *, #29141, .F. ) ;
#26231 = EDGE_CURVE ( 'NONE', #17577, #5759, #47063, .T. ) ;
#26232 = PLANE ( 'NONE',  #38001 ) ;
#26233 = ORIENTED_EDGE ( 'NONE', *, *, #15766, .F. ) ;
#26234 = EDGE_CURVE ( 'NONE', #34277, #50878, #47584, .T. ) ;
#26235 = CIRCLE ( 'NONE', #35459, 125.0000000000000000 ) ;
#26236 = CARTESIAN_POINT ( 'NONE',  ( -339.1964088526558498, -68.15673923803898049, 20.45418021416614351 ) ) ;
#26237 = CARTESIAN_POINT ( 'NONE',  ( -124.4642912599203726, -175.3837268820161057, 99.25348746834863789 ) ) ;
#26238 = DIRECTION ( 'NONE',  ( -1.000000000000000000, -0.000000000000000000, -0.000000000000000000 ) ) ;
#26239 = EDGE_CURVE ( 'NONE', #39687, #4324, #31017, .T. ) ;
#26240 = DIRECTION ( 'NONE',  ( -1.000000000000000000, 0.000000000000000000, -0.000000000000000000 ) ) ;
#26241 = EDGE_CURVE ( 'NONE', #6939, #10029, #11038, .T. ) ;
#26242 = CARTESIAN_POINT ( 'NONE',  ( 55.91309001144630031, -177.1207230881787780, 68.75510947788670535 ) ) ;
#26243 = VECTOR ( 'NONE', #10990, 1000.000000000000000 ) ;
#26244 = ORIENTED_EDGE ( 'NONE', *, *, #34796, .F. ) ;
#26245 = ADVANCED_FACE ( 'NONE', ( #7381 ), #1, .F. ) ;
#26246 = DIRECTION ( 'NONE',  ( 0.000000000000000000, -0.9350162426854121689, 0.3546048870425426158 ) ) ;
#26247 = ORIENTED_EDGE ( 'NONE', *, *, #15342, .F. ) ;
#26248 = CARTESIAN_POINT ( 'NONE',  ( 51.70113075622899856, 30.00000000000000355, -45.78969942005421956 ) ) ;
#26249 = VECTOR ( 'NONE', #5515, 1000.000000000000114 ) ;
#26250 = AXIS2_PLACEMENT_3D ( 'NONE', #47326, #11297, #19212 ) ;
#26251 = EDGE_CURVE ( 'NONE', #22171, #36591, #5145, .T. ) ;
#26252 = VERTEX_POINT ( 'NONE', #3169 ) ;
#26253 = CARTESIAN_POINT ( 'NONE',  ( 74.28166149629942083, -193.5000000000000000, 17.48697739784543614 ) ) ;
#26254 = EDGE_CURVE ( 'NONE', #20806, #14667, #27064, .T. ) ;
#26255 = VECTOR ( 'NONE', #27010, 1000.000000000000000 ) ;
#26256 = DIRECTION ( 'NONE',  ( -0.000000000000000000, 0.8854560256532141294, 0.4647231720437604574 ) ) ;
#26257 = LINE ( 'NONE', #5809, #31490 ) ;
#26258 = ORIENTED_EDGE ( 'NONE', *, *, #15943, .F. ) ;
#26261 = ORIENTED_EDGE ( 'NONE', *, *, #19145, .F. ) ;
#26260 = FACE_OUTER_BOUND ( 'NONE', #10506, .T. ) ;
#26259 = FACE_OUTER_BOUND ( 'NONE', #42211, .T. ) ;
#26262 = DIRECTION ( 'NONE',  ( -0.9929810960135185827, 0.000000000000000000, 0.1182731709213523247 ) ) ;
#26263 = ORIENTED_EDGE ( 'NONE', *, *, #8678, .T. ) ;
#26264 = CARTESIAN_POINT ( 'NONE',  ( -170.0000000000000284, -115.7896721143442278, 60.00000000000000711 ) ) ;
#26265 = AXIS2_PLACEMENT_3D ( 'NONE', #31196, #47247, #11218 ) ;
#26266 = ORIENTED_EDGE ( 'NONE', *, *, #41475, .F. ) ;
#26267 = DIRECTION ( 'NONE',  ( 0.000000000000000000, 0.000000000000000000, 1.000000000000000000 ) ) ;
#26270 = ORIENTED_EDGE ( 'NONE', *, *, #46913, .T. ) ;
#26269 = DIRECTION ( 'NONE',  ( 0.000000000000000000, 0.000000000000000000, -1.000000000000000000 ) ) ;
#26268 = CARTESIAN_POINT ( 'NONE',  ( -48.41988612361515010, -193.5000000000000000, 0.9982437317643287900 ) ) ;
#26271 = ADVANCED_FACE ( 'NONE', ( #7622 ), #23403, .T. ) ;
#26272 = ORIENTED_EDGE ( 'NONE', *, *, #34317, .T. ) ;
#26273 = AXIS2_PLACEMENT_3D ( 'NONE', #36326, #36070, #28170 ) ;
#26274 = PLANE ( 'NONE',  #3896 ) ;
#26275 = EDGE_LOOP ( 'NONE', ( #8298, #45072, #21912, #33256 ) ) ;
#26276 = CARTESIAN_POINT ( 'NONE',  ( -47.70260288879081401, -193.5000000000000000, 0.6300878435817218737 ) ) ;
#26277 = DIRECTION ( 'NONE',  ( -0.7765238627180482966, 0.000000000000000000, 0.6300878435817038881 ) ) ;
#26278 = EDGE_LOOP ( 'NONE', ( #49564, #45555, #38734, #35672 ) ) ;
#26279 = LINE ( 'NONE', #34683, #39794 ) ;
#26280 = DIRECTION ( 'NONE',  ( -1.000000000000000000, 0.000000000000000000, 0.000000000000000000 ) ) ;
#26281 = DIRECTION ( 'NONE',  ( 0.000000000000000000, 0.9350162426854132791, -0.3546048870425396182 ) ) ;
#26282 = CARTESIAN_POINT ( 'NONE',  ( -339.1964088526558498, -74.65991953890826949, 33.10432812419072945 ) ) ;
#26283 = CARTESIAN_POINT ( 'NONE',  ( -330.4913330509368166, -183.4979166304964622, 0.4999999999999549249 ) ) ;
#26284 = VERTEX_POINT ( 'NONE', #19204 ) ;
#26285 = VECTOR ( 'NONE', #8979, 1000.000000000000000 ) ;
#26286 = CARTESIAN_POINT ( 'NONE',  ( 40.29886924377099433, 30.00000000000000355, -46.21030057994576623 ) ) ;
#26287 = LINE ( 'NONE', #38383, #7215 ) ;
#26288 = EDGE_CURVE ( 'NONE', #716, #39966, #19444, .T. ) ;
#26289 = FACE_OUTER_BOUND ( 'NONE', #47991, .T. ) ;
#26290 = VERTEX_POINT ( 'NONE', #51269 ) ;
#26291 = AXIS2_PLACEMENT_3D ( 'NONE', #35797, #51855, #27660 ) ;
#26292 = FACE_OUTER_BOUND ( 'NONE', #12570, .T. ) ;
#26293 = DIRECTION ( 'NONE',  ( -8.718379230999704661E-17, -0.5680647467311626952, -0.8229838658936516893 ) ) ;
#26294 = EDGE_CURVE ( 'NONE', #246, #48253, #32041, .T. ) ;
#26295 = DIRECTION ( 'NONE',  ( 0.000000000000000000, 0.000000000000000000, 1.000000000000000000 ) ) ;
#26296 = EDGE_CURVE ( 'NONE', #37376, #5960, #15255, .T. ) ;
#26297 = FACE_OUTER_BOUND ( 'NONE', #50602, .T. ) ;
#26298 = ADVANCED_FACE ( 'NONE', ( #47322 ), #2904, .T. ) ;
#26299 = ADVANCED_FACE ( 'NONE', ( #31269 ), #11291, .T. ) ;
#26300 = VECTOR ( 'NONE', #37232, 1000.000000000000000 ) ;
#26301 = VERTEX_POINT ( 'NONE', #38899 ) ;
#26302 = EDGE_CURVE ( 'NONE', #18571, #23872, #6852, .T. ) ;
#26303 = CYLINDRICAL_SURFACE ( 'NONE', #40533, 124.9999999999999858 ) ;
#26304 = ADVANCED_FACE ( 'NONE', ( #31528 ), #11569, .T. ) ;
#26305 = PLANE ( 'NONE',  #50531 ) ;
#26306 = FACE_OUTER_BOUND ( 'NONE', #4128, .T. ) ;
#26307 = DIRECTION ( 'NONE',  ( 0.000000000000000000, 0.000000000000000000, 1.000000000000000000 ) ) ;
#26308 = VECTOR ( 'NONE', #8648, 1000.000000000000000 ) ;
#26309 = VERTEX_POINT ( 'NONE', #31805 ) ;
#26310 = EDGE_CURVE ( 'NONE', #51040, #27425, #12654, .T. ) ;
#26311 = CARTESIAN_POINT ( 'NONE',  ( 42.89728982752370001, -193.5000000000000000, 83.82333043185313670 ) ) ;
#26312 = VECTOR ( 'NONE', #2657, 1000.000000000000000 ) ;
#26313 = EDGE_CURVE ( 'NONE', #17026, #37409, #43875, .T. ) ;
#26314 = DIRECTION ( 'NONE',  ( -0.000000000000000000, 1.000000000000000000, -0.000000000000000000 ) ) ;
#26316 = ORIENTED_EDGE ( 'NONE', *, *, #49430, .T. ) ;
#26315 = DIRECTION ( 'NONE',  ( 0.1182731709213730997, 0.000000000000000000, -0.9929810960135161402 ) ) ;
#26317 = VERTEX_POINT ( 'NONE', #17345 ) ;
#26318 = EDGE_CURVE ( 'NONE', #36451, #48105, #12853, .T. ) ;
#26319 = VERTEX_POINT ( 'NONE', #36245 ) ;
#26320 = DIRECTION ( 'NONE',  ( -0.000000000000000000, -0.9927088740980544168, -0.1205366802553199251 ) ) ;
#26321 = ADVANCED_FACE ( 'NONE', ( #8918 ), #1286, .T. ) ;
#26322 = CARTESIAN_POINT ( 'NONE',  ( -332.3517673607765914, -70.03480886230919111, 25.08789112700620194 ) ) ;
#26323 = DIRECTION ( 'NONE',  ( 0.000000000000000000, -1.000000000000000000, 0.000000000000000000 ) ) ;
#26325 = ORIENTED_EDGE ( 'NONE', *, *, #16012, .F. ) ;
#26324 = VECTOR ( 'NONE', #30030, 1000.000000000000000 ) ;
#26326 = EDGE_CURVE ( 'NONE', #6390, #29097, #4721, .T. ) ;
#26327 = CARTESIAN_POINT ( 'NONE',  ( -48.77118352214581876, -175.3837268820161057, -0.9564009842765195391 ) ) ;
#26328 = LINE ( 'NONE', #10558, #42859 ) ;
#26331 = EDGE_LOOP ( 'NONE', ( #17510, #26258, #31374, #20382 ) ) ;
#26330 = CARTESIAN_POINT ( 'NONE',  ( 25.43954814678888710, -183.6283474603465606, 100.8019320314832754 ) ) ;
#26329 = DIRECTION ( 'NONE',  ( -0.000000000000000000, -0.9350162426854158326, -0.3546048870425331234 ) ) ;
#26332 = VECTOR ( 'NONE', #24659, 1000.000000000000227 ) ;
#26333 = FACE_OUTER_BOUND ( 'NONE', #44566, .T. ) ;
#26334 = ORIENTED_EDGE ( 'NONE', *, *, #45334, .F. ) ;
#26335 = CARTESIAN_POINT ( 'NONE',  ( -60.86541030502398542, -183.6283474603465606, -124.3848060646151623 ) ) ;
#26336 = EDGE_LOOP ( 'NONE', ( #909, #37780, #29056, #48141 ) ) ;
#26337 = CARTESIAN_POINT ( 'NONE',  ( -165.2002711502080672, -177.1207230881787780, 44.73448837594995098 ) ) ;
#26338 = CARTESIAN_POINT ( 'NONE',  ( -52.47502265695599988, -183.6283474603465606, -124.9361149384469485 ) ) ;
#26339 = FACE_OUTER_BOUND ( 'NONE', #39187, .T. ) ;
#26340 = EDGE_CURVE ( 'NONE', #22344, #24544, #11826, .T. ) ;
#26341 = CARTESIAN_POINT ( 'NONE',  ( -180.0000000000000568, -130.6726371812771959, 60.00000000000000711 ) ) ;
#26342 = ORIENTED_EDGE ( 'NONE', *, *, #45897, .F. ) ;
#26343 = DIRECTION ( 'NONE',  ( -0.000000000000000000, 1.000000000000000000, -0.000000000000000000 ) ) ;
#26344 = DIRECTION ( 'NONE',  ( 0.000000000000000000, -0.3546048870425235200, 0.9350162426854194964 ) ) ;
#26345 = ORIENTED_EDGE ( 'NONE', *, *, #50042, .T. ) ;
#26346 = DIRECTION ( 'NONE',  ( -0.7175072570443299380, 0.000000000000000000, -0.6965510290629983725 ) ) ;
#26347 = VECTOR ( 'NONE', #37286, 1000.000000000000000 ) ;
#26348 = FACE_OUTER_BOUND ( 'NONE', #28017, .T. ) ;
#26349 = AXIS2_PLACEMENT_3D ( 'NONE', #50109, #37486, #1743 ) ;
#26350 = ORIENTED_EDGE ( 'NONE', *, *, #13724, .T. ) ;
#26351 = FACE_BOUND ( 'NONE', #15880, .T. ) ;
#26353 = AXIS2_PLACEMENT_3D ( 'NONE', #36174, #36427, #24112 ) ;
#26352 = DIRECTION ( 'NONE',  ( 0.000000000000000000, -1.000000000000000000, 0.000000000000000000 ) ) ;
#26354 = ORIENTED_EDGE ( 'NONE', *, *, #14279, .F. ) ;
#26355 = DIRECTION ( 'NONE',  ( -0.000000000000000000, 1.000000000000000000, -0.000000000000000000 ) ) ;
#26356 = ORIENTED_EDGE ( 'NONE', *, *, #933, .F. ) ;
#26357 = CARTESIAN_POINT ( 'NONE',  ( -332.3517673607765914, -179.0013928959018301, 22.79463504017430253 ) ) ;
#26358 = DIRECTION ( 'NONE',  ( 0.000000000000000000, -0.000000000000000000, 1.000000000000000000 ) ) ;
#26359 = ORIENTED_EDGE ( 'NONE', *, *, #38055, .F. ) ;
#26360 = ADVANCED_FACE ( 'NONE', ( #9193 ), #36500, .T. ) ;
#26361 = CARTESIAN_POINT ( 'NONE',  ( -305.0000000000000568, -114.6500883362968892, 59.34373651485599055 ) ) ;
#26362 = CARTESIAN_POINT ( 'NONE',  ( -339.1964088526558498, -123.0000000000002700, -59.00000000000002132 ) ) ;
#26363 = CARTESIAN_POINT ( 'NONE',  ( -161.4019114581580823, -175.3837268820161057, 53.60452120946281696 ) ) ;
#26364 = EDGE_CURVE ( 'NONE', #19097, #14965, #41206, .T. ) ;
#26365 = AXIS2_PLACEMENT_3D ( 'NONE', #41965, #45413, #33045 ) ;
#26366 = VERTEX_POINT ( 'NONE', #21269 ) ;
#26367 = DIRECTION ( 'NONE',  ( 0.000000000000000000, 1.000000000000000000, -0.000000000000000000 ) ) ;
#26368 =( REPRESENTATION_RELATIONSHIP ('NONE','NONE', #4578, #11639 ) REPRESENTATION_RELATIONSHIP_WITH_TRANSFORMATION ( #14414 )SHAPE_REPRESENTATION_RELATIONSHIP( ) );
#26369 = VERTEX_POINT ( 'NONE', #44413 ) ;
#26370 = CARTESIAN_POINT ( 'NONE',  ( -339.1964088526558498, -123.5000000000000284, 0.000000000000000000 ) ) ;
#26371 = CARTESIAN_POINT ( 'NONE',  ( -15.24927435600541692, -193.5000000000000000, 120.5021863277719234 ) ) ;
#26373 = EDGE_LOOP ( 'NONE', ( #30405, #50381, #49213, #3066 ) ) ;
#26372 = DIRECTION ( 'NONE',  ( -1.000000000000000000, 0.000000000000000000, 0.000000000000000000 ) ) ;
#26374 = ORIENTED_EDGE ( 'NONE', *, *, #36631, .T. ) ;
#26375 = CARTESIAN_POINT ( 'NONE',  ( -73.94077438226446475, -183.6283474603465606, 122.3793467049372481 ) ) ;
#26376 = DIRECTION ( 'NONE',  ( 0.000000000000000000, -0.6631226582407911962, 0.7485107481711046340 ) ) ;
#26377 = ORIENTED_EDGE ( 'NONE', *, *, #8283, .T. ) ;
#26378 = DIRECTION ( 'NONE',  ( 0.3482016354343866471, 0.000000000000000000, 0.9374196611341253371 ) ) ;
#26379 = ADVANCED_FACE ( 'NONE', ( #8656 ), #40976, .F. ) ;
#26380 = ORIENTED_EDGE ( 'NONE', *, *, #51421, .F. ) ;
#26381 = LINE ( 'NONE', #50321, #11575 ) ;
#26382 = CARTESIAN_POINT ( 'NONE',  ( -336.3521761649654422, -69.26746417191145611, -23.38292116578723068 ) ) ;
#26383 = AXIS2_PLACEMENT_3D ( 'NONE', #46581, #50273, #22914 ) ;
#26384 = VECTOR ( 'NONE', #42578, 1000.000000000000000 ) ;
#26385 = PLANE ( 'NONE',  #49606 ) ;
#26386 = DIRECTION ( 'NONE',  ( -0.000000000000000000, 1.000000000000000000, -0.000000000000000000 ) ) ;
#26387 = EDGE_LOOP ( 'NONE', ( #15234, #29531 ) ) ;
#26388 = ORIENTED_EDGE ( 'NONE', *, *, #38951, .F. ) ;
#26389 = AXIS2_PLACEMENT_3D ( 'NONE', #43742, #31392, #4580 ) ;
#26390 = EDGE_CURVE ( 'NONE', #5817, #13416, #37028, .T. ) ;
#26391 = EDGE_LOOP ( 'NONE', ( #22835, #50290, #21088, #22964 ) ) ;
#26392 = DIRECTION ( 'NONE',  ( -1.000000000000000000, 0.000000000000000000, 4.884776371667510679E-16 ) ) ;
#26393 = DIRECTION ( 'NONE',  ( -0.2348860457809707758, 0.000000000000000000, -0.9720229140804138579 ) ) ;
#26394 = DIRECTION ( 'NONE',  ( 0.8124868780056783146, 0.000000000000000000, 0.5829794791144762289 ) ) ;
#26395 = DIRECTION ( 'NONE',  ( 0.000000000000000000, 0.000000000000000000, 1.000000000000000000 ) ) ;
#26396 = VERTEX_POINT ( 'NONE', #40440 ) ;
#26397 = VECTOR ( 'NONE', #50912, 1000.000000000000000 ) ;
#26398 = DIRECTION ( 'NONE',  ( 0.000000000000000000, 0.000000000000000000, 1.000000000000000000 ) ) ;
#26399 = ORIENTED_EDGE ( 'NONE', *, *, #34059, .T. ) ;
#26400 = ORIENTED_EDGE ( 'NONE', *, *, #33665, .F. ) ;
#26401 = CARTESIAN_POINT ( 'NONE',  ( -332.3517673607765914, -182.3303666475049170, -11.78931550685388707 ) ) ;
#26402 = DIRECTION ( 'NONE',  ( 0.2348860457809842095, 0.000000000000000000, -0.9720229140804107493 ) ) ;
#26403 = DIRECTION ( 'NONE',  ( 0.000000000000000000, -0.8660254037844354880, -0.5000000000000054401 ) ) ;
#26404 = CARTESIAN_POINT ( 'NONE',  ( -158.9435005891547803, -183.6283474603465606, -56.33604425924762182 ) ) ;
#26405 = ORIENTED_EDGE ( 'NONE', *, *, #27279, .F. ) ;
#26406 = CARTESIAN_POINT ( 'NONE',  ( -305.0000000000000568, -179.4217241332782464, 21.74306257088749206 ) ) ;
#26407 = VERTEX_POINT ( 'NONE', #13385 ) ;
#26408 = DIRECTION ( 'NONE',  ( 1.000000000000000000, 0.000000000000000000, -0.000000000000000000 ) ) ;
#26409 = VECTOR ( 'NONE', #42775, 1000.000000000000000 ) ;
#26410 = CARTESIAN_POINT ( 'NONE',  ( 68.24201764719070695, -193.5000000000000000, -44.73448837594909833 ) ) ;
#26411 = ORIENTED_EDGE ( 'NONE', *, *, #28260, .F. ) ;
#26412 = AXIS2_PLACEMENT_3D ( 'NONE', #14263, #22402, #38426 ) ;
#26413 = VECTOR ( 'NONE', #19510, 1000.000000000000000 ) ;
#26414 = FACE_OUTER_BOUND ( 'NONE', #12748, .T. ) ;
#26415 = DIRECTION ( 'NONE',  ( 0.000000000000000000, 0.000000000000000000, -1.000000000000000000 ) ) ;
#26416 = DIRECTION ( 'NONE',  ( 0.9027978299657446470, 0.000000000000000000, -0.4300652022765183435 ) ) ;
#26417 = EDGE_CURVE ( 'NONE', #22639, #1324, #18523, .T. ) ;
#26418 = DIRECTION ( 'NONE',  ( -1.000000000000000000, 0.000000000000000000, 0.000000000000000000 ) ) ;
#26419 = AXIS2_PLACEMENT_3D ( 'NONE', #34390, #2060, #18102 ) ;
#26420 = CARTESIAN_POINT ( 'NONE',  ( -48.47912675150885065, -189.7472609257535510, 6.938893903907228378E-15 ) ) ;
#26421 = VERTEX_POINT ( 'NONE', #48350 ) ;
#26422 = CIRCLE ( 'NONE', #2946, 4.999999999999997335 ) ;
#26423 = DIRECTION ( 'NONE',  ( -0.9473263538541899509, 0.000000000000000000, -0.3202698538628415692 ) ) ;
#26424 = ORIENTED_EDGE ( 'NONE', *, *, #9365, .T. ) ;
#26425 = CIRCLE ( 'NONE', #32310, 125.0000000000000000 ) ;
#26426 = ORIENTED_EDGE ( 'NONE', *, *, #43822, .T. ) ;
#26427 = DIRECTION ( 'NONE',  ( -0.000000000000000000, -0.5000000000000013323, 0.8660254037844380415 ) ) ;
#26428 = CIRCLE ( 'NONE', #14668, 125.0000000000000000 ) ;
#26429 = EDGE_LOOP ( 'NONE', ( #48434, #8911, #6438, #42213 ) ) ;
#26430 = PRODUCT ( 'MAS-325', 'MAS-325', '', ( #28866 ) ) ;
#26431 = CARTESIAN_POINT ( 'NONE',  ( -170.7635349987907034, -189.7472609257535510, -25.91377046305883169 ) ) ;
#26432 = ORIENTED_EDGE ( 'NONE', *, *, #41548, .T. ) ;
#26433 = CYLINDRICAL_SURFACE ( 'NONE', #20045, 125.0000000000000000 ) ;
#26434 = LINE ( 'NONE', #14363, #42222 ) ;
#26435 = EDGE_CURVE ( 'NONE', #32675, #41833, #16019, .T. ) ;
#26436 = ORIENTED_EDGE ( 'NONE', *, *, #29434, .F. ) ;
#26437 = CARTESIAN_POINT ( 'NONE',  ( -172.9701362814535912, -175.3837268820161057, -11.26891947860193177 ) ) ;
#26438 = CARTESIAN_POINT ( 'NONE',  ( -48.47912675150885065, -175.3837268820161057, 6.938893903907228378E-15 ) ) ;
#26439 = CARTESIAN_POINT ( 'NONE',  ( -332.3517673607765914, -72.01665693856799066, -28.86398714850468039 ) ) ;
#26440 = ORIENTED_EDGE ( 'NONE', *, *, #49031, .F. ) ;
#26441 = EDGE_LOOP ( 'NONE', ( #8346, #3912, #20074, #14711 ) ) ;
#26442 = VERTEX_POINT ( 'NONE', #4994 ) ;
#26443 = LINE ( 'NONE', #42478, #734 ) ;
#26444 = CARTESIAN_POINT ( 'NONE',  ( 76.28370911321322012, -177.1207230881787780, -7.696413904697510411 ) ) ;
#26445 = VECTOR ( 'NONE', #27118, 1000.000000000000000 ) ;
#26446 = CARTESIAN_POINT ( 'NONE',  ( -336.3521761649654422, -149.4733471526596134, 53.00046796564699036 ) ) ;
#26447 = VECTOR ( 'NONE', #35323, 1000.000000000000000 ) ;
#26448 = DIRECTION ( 'NONE',  ( -1.000000000000000000, 0.000000000000000000, 0.000000000000000000 ) ) ;
#26449 = CARTESIAN_POINT ( 'NONE',  ( -49.35486169370448550, -193.5000000000000000, -0.4827922027307481878 ) ) ;
#26450 = VERTEX_POINT ( 'NONE', #29142 ) ;
#26451 = CIRCLE ( 'NONE', #35679, 60.00000000000000000 ) ;
#26452 = VECTOR ( 'NONE', #18801, 1000.000000000000000 ) ;
#26453 = DIRECTION ( 'NONE',  ( -0.000000000000000000, 1.000000000000000000, 0.000000000000000000 ) ) ;
#26454 = VERTEX_POINT ( 'NONE', #16823 ) ;
#26456 = ORIENTED_EDGE ( 'NONE', *, *, #45897, .T. ) ;
#26455 = CARTESIAN_POINT ( 'NONE',  ( -339.1964088526558498, -151.3613951634092700, -52.00954392751739164 ) ) ;
#26457 = VERTEX_POINT ( 'NONE', #12595 ) ;
#26458 = CARTESIAN_POINT ( 'NONE',  ( 36.84288420123323249, -183.6283474603465606, 91.35181687837503262 ) ) ;
#26459 = AXIS2_PLACEMENT_3D ( 'NONE', #3852, #35637, #19876 ) ;
#26460 = ORIENTED_EDGE ( 'NONE', *, *, #7952, .F. ) ;
#26461 = CARTESIAN_POINT ( 'NONE',  ( -330.4913330509368166, -66.09477493971897388, 13.63415328425216622 ) ) ;
#26462 = AXIS2_PLACEMENT_3D ( 'NONE', #21190, #29584, #29328 ) ;
#26463 = EDGE_CURVE ( 'NONE', #18846, #16398, #25236, .T. ) ;
#26464 = LINE ( 'NONE', #21767, #51513 ) ;
#26465 = LINE ( 'NONE', #1780, #20901 ) ;
#26466 = ORIENTED_EDGE ( 'NONE', *, *, #32224, .F. ) ;
#26467 = CARTESIAN_POINT ( 'NONE',  ( 18.49541618049843095, -177.1207230881787780, 105.5434062319798159 ) ) ;
#26468 = VECTOR ( 'NONE', #42814, 1000.000000000000000 ) ;
#26469 = ORIENTED_EDGE ( 'NONE', *, *, #29929, .T. ) ;
#26470 = EDGE_CURVE ( 'NONE', #40253, #11142, #20225, .T. ) ;
#26471 = CIRCLE ( 'NONE', #6348, 4.999999999999997335 ) ;
#26472 = ORIENTED_EDGE ( 'NONE', *, *, #36863, .T. ) ;
#26473 = CARTESIAN_POINT ( 'NONE',  ( -332.3517673607765914, -123.5000000000000284, 0.000000000000000000 ) ) ;
#26474 = CARTESIAN_POINT ( 'NONE',  ( 71.44208735029287993, -183.6283474603465606, 35.26900067126700833 ) ) ;
#26475 = PLANE ( 'NONE',  #36640 ) ;
#26476 = EDGE_LOOP ( 'NONE', ( #26244, #14023, #15742, #43902 ) ) ;
#26477 = CARTESIAN_POINT ( 'NONE',  ( 3.686287386450715076E-15, 20.00000000000000000, -46.00000000000000711 ) ) ;
#26478 = DIRECTION ( 'NONE',  ( 0.000000000000000000, 0.000000000000000000, -1.000000000000000000 ) ) ;
#26479 = PLANE ( 'NONE',  #17923 ) ;
#26480 = CARTESIAN_POINT ( 'NONE',  ( -173.2419626162308361, -177.1207230881787780, 7.696413904698415465 ) ) ;
#26481 = EDGE_CURVE ( 'NONE', #51204, #10929, #17081, .T. ) ;
#26482 = VERTEX_POINT ( 'NONE', #49134 ) ;
#26483 = LINE ( 'NONE', #34384, #10399 ) ;
#26484 = CARTESIAN_POINT ( 'NONE',  ( 58.95724912996274725, -183.6283474603465606, 61.91627321685103169 ) ) ;
#26485 = EDGE_CURVE ( 'NONE', #35874, #39674, #49594, .T. ) ;
#26486 = FACE_BOUND ( 'NONE', #24166, .T. ) ;
#26487 = EDGE_LOOP ( 'NONE', ( #41947, #37323, #31894, #7938 ) ) ;
#26488 = ADVANCED_FACE ( 'NONE', ( #241 ), #29659, .F. ) ;
#26489 = AXIS2_PLACEMENT_3D ( 'NONE', #38054, #10457, #22567 ) ;
#26490 = DIRECTION ( 'NONE',  ( -0.8124868780056742068, 0.000000000000000000, -0.5829794791144820021 ) ) ;
#26491 = CIRCLE ( 'NONE', #17280, 125.0000000000000000 ) ;
#26492 = VECTOR ( 'NONE', #18681, 1000.000000000000000 ) ;
#26493 = CARTESIAN_POINT ( 'NONE',  ( 76.46082103836693022, -193.5000000000000000, 3.874202661595785191 ) ) ;
#26494 = EDGE_LOOP ( 'NONE', ( #51385, #37640, #2614, #6247 ) ) ;
#26495 = PLANE ( 'NONE',  #43037 ) ;
#26496 = ORIENTED_EDGE ( 'NONE', *, *, #38224, .F. ) ;
#26497 = DIRECTION ( 'NONE',  ( 0.000000000000000000, 0.000000000000000000, -1.000000000000000000 ) ) ;
#26498 = PLANE ( 'NONE',  #35420 ) ;
#26499 = VECTOR ( 'NONE', #11330, 1000.000000000000000 ) ;
#26500 = DIRECTION ( 'NONE',  ( 0.000000000000000000, -0.000000000000000000, 1.000000000000000000 ) ) ;
#26501 = EDGE_CURVE ( 'NONE', #10308, #27859, #4264, .T. ) ;
#26502 = AXIS2_PLACEMENT_3D ( 'NONE', #35859, #47952, #51917 ) ;
#26503 = DIRECTION ( 'NONE',  ( -0.000000000000000000, 0.7485107481711069655, 0.6631226582407885317 ) ) ;
#26504 = AXIS2_PLACEMENT_3D ( 'NONE', #32268, #17053, #40666 ) ;
#26505 = DIRECTION ( 'NONE',  ( -0.000000000000000000, 0.000000000000000000, 1.000000000000000000 ) ) ;
#26506 = VERTEX_POINT ( 'NONE', #25467 ) ;
#26507 = PLANE ( 'NONE',  #33179 ) ;
#26508 = ORIENTED_EDGE ( 'NONE', *, *, #23081, .F. ) ;
#26509 = AXIS2_PLACEMENT_3D ( 'NONE', #35589, #51640, #31661 ) ;
#26510 = LINE ( 'NONE', #42541, #11609 ) ;
#26511 = EDGE_LOOP ( 'NONE', ( #26224, #10491, #23916, #23488 ) ) ;
#26512 = DIRECTION ( 'NONE',  ( -0.2348860457809707758, 0.000000000000000000, -0.9720229140804138579 ) ) ;
#26513 = CARTESIAN_POINT ( 'NONE',  ( -133.1483155860611021, -193.5000000000000000, -90.59430563621275212 ) ) ;
#26514 = DIRECTION ( 'NONE',  ( -0.000000000000000000, 1.000000000000000000, -0.000000000000000000 ) ) ;
#26515 = ORIENTED_EDGE ( 'NONE', *, *, #47534, .F. ) ;
#26518 = EDGE_LOOP ( 'NONE', ( #45134, #10238, #43079, #9311 ) ) ;
#26517 = CYLINDRICAL_SURFACE ( 'NONE', #19706, 125.0000000000000000 ) ;
#26516 = CARTESIAN_POINT ( 'NONE',  ( -3.547000324993504261, 51.93490815224947710, -20.18691131683817730 ) ) ;
#26519 = AXIS2_PLACEMENT_3D ( 'NONE', #13041, #25147, #432 ) ;
#26520 = AXIS2_PLACEMENT_3D ( 'NONE', #30946, #22805, #23065 ) ;
#26521 = CARTESIAN_POINT ( 'NONE',  ( -77.67449977936063021, -175.3837268820161057, -121.5427093402339267 ) ) ;
#26522 = AXIS2_PLACEMENT_3D ( 'NONE', #19954, #7604, #226 ) ;
#26523 = VERTEX_POINT ( 'NONE', #42527 ) ;
#26524 = LINE ( 'NONE', #22850, #14650 ) ;
#26525 = VERTEX_POINT ( 'NONE', #30432 ) ;
#26526 = VECTOR ( 'NONE', #42319, 1000.000000000000000 ) ;
#26527 = ADVANCED_FACE ( 'NONE', ( #1558 ), #34132, .T. ) ;
#26528 = EDGE_CURVE ( 'NONE', #11646, #5101, #48769, .T. ) ;
#26529 = DIRECTION ( 'NONE',  ( 0.000000000000000000, 0.000000000000000000, -1.000000000000000000 ) ) ;
#26532 = ORIENTED_EDGE ( 'NONE', *, *, #31124, .T. ) ;
#26531 = DIRECTION ( 'NONE',  ( -0.000000000000000000, 1.000000000000000000, -0.000000000000000000 ) ) ;
#26530 = PLANE ( 'NONE',  #28271 ) ;
#26533 = ORIENTED_EDGE ( 'NONE', *, *, #13134, .T. ) ;
#26534 = CARTESIAN_POINT ( 'NONE',  ( 57.31108707223381771, -189.7472609257535510, -66.58401203837752291 ) ) ;
#26535 = ORIENTED_EDGE ( 'NONE', *, *, #37206, .T. ) ;
#26536 = DIRECTION ( 'NONE',  ( 0.000000000000000000, 0.000000000000000000, 1.000000000000000000 ) ) ;
#26537 = DIRECTION ( 'NONE',  ( -0.000000000000000000, 1.000000000000000000, -0.000000000000000000 ) ) ;
#26538 = ORIENTED_EDGE ( 'NONE', *, *, #51045, .F. ) ;
#26539 = CIRCLE ( 'NONE', #32430, 125.0000000000000000 ) ;
#26540 = DIRECTION ( 'NONE',  ( -0.05924062789371441901, 0.000000000000000000, 0.9982437317643214625 ) ) ;
#26541 = DIRECTION ( 'NONE',  ( 0.000000000000000000, -0.1205366802553233113, -0.9927088740980539727 ) ) ;
#26542 = CARTESIAN_POINT ( 'NONE',  ( -60.86541030502395699, -177.1207230881787780, -124.3848060646151481 ) ) ;
#26543 = CARTESIAN_POINT ( 'NONE',  ( 34.98161733638499271, -177.1207230881787780, -91.70840728318313495 ) ) ;
#26544 = VECTOR ( 'NONE', #30608, 1000.000000000000000 ) ;
#26545 = AXIS2_PLACEMENT_3D ( 'NONE', #36233, #4446, #40427 ) ;
#26546 = DIRECTION ( 'NONE',  ( 0.000000000000000000, -0.000000000000000000, 1.000000000000000000 ) ) ;
#26547 = ORIENTED_EDGE ( 'NONE', *, *, #42310, .F. ) ;
#26548 = ADVANCED_FACE ( 'NONE', ( #29925 ), #22297, .F. ) ;
#26549 = VECTOR ( 'NONE', #17121, 1000.000000000000000 ) ;
#26550 = LINE ( 'NONE', #6601, #13712 ) ;
#26551 = CARTESIAN_POINT ( 'NONE',  ( -150.1390659022305840, -189.7472609257535510, 72.73415134496008250 ) ) ;
#26552 = ADVANCED_FACE ( 'NONE', ( #6547 ), #17598, .T. ) ;
#26553 = VECTOR ( 'NONE', #7657, 1000.000000000000000 ) ;
#26554 = DIRECTION ( 'NONE',  ( 0.7378332790417189146, 0.000000000000000000, 0.6749830015182196608 ) ) ;
#26555 = ORIENTED_EDGE ( 'NONE', *, *, #23986, .F. ) ;
#26556 = ADVANCED_FACE ( 'NONE', ( #49905, #22575, #25730, #37561, #45985, #22040, #38585, #33610, #5784, #30193 ), #49652, .T. ) ;
#26557 = DIRECTION ( 'NONE',  ( 0.9995608365087944591, 0.000000000000000000, -0.02963332782255633305 ) ) ;
#26558 = DIRECTION ( 'NONE',  ( 0.000000000000000000, -0.000000000000000000, 1.000000000000000000 ) ) ;
#26559 = EDGE_CURVE ( 'NONE', #37732, #37490, #46235, .T. ) ;
#26560 = DIRECTION ( 'NONE',  ( 0.000000000000000000, -0.000000000000000000, 1.000000000000000000 ) ) ;
#26561 = CARTESIAN_POINT ( 'NONE',  ( -139.0630283577175987, -183.6283474603465606, -86.13684908212448477 ) ) ;
#26562 = ORIENTED_EDGE ( 'NONE', *, *, #39768, .F. ) ;
#26563 = VECTOR ( 'NONE', #43441, 1000.000000000000000 ) ;
#26564 = DIRECTION ( 'NONE',  ( -0.000000000000000000, 1.000000000000000000, -0.000000000000000000 ) ) ;
#26565 = CARTESIAN_POINT ( 'NONE',  ( -137.6740394605055826, -177.1207230881787780, -86.14171647324863557 ) ) ;
#26566 = CARTESIAN_POINT ( 'NONE',  ( 40.26790151320558664, -177.1207230881787780, -86.60307583628353711 ) ) ;
#26567 = VECTOR ( 'NONE', #11203, 1000.000000000000000 ) ;
#26568 = ORIENTED_EDGE ( 'NONE', *, *, #37914, .T. ) ;
#26569 = LINE ( 'NONE', #14760, #28535 ) ;
#26570 = DIRECTION ( 'NONE',  ( 0.000000000000000000, 0.000000000000000000, -1.000000000000000000 ) ) ;
#26571 = VERTEX_POINT ( 'NONE', #18621 ) ;
#26572 = CIRCLE ( 'NONE', #29080, 125.0000000000000000 ) ;
#26573 = ORIENTED_EDGE ( 'NONE', *, *, #47196, .F. ) ;
#26574 = AXIS2_PLACEMENT_3D ( 'NONE', #30486, #23130, #27315 ) ;
#26575 = ORIENTED_EDGE ( 'NONE', *, *, #46958, .F. ) ;
#26576 = DIRECTION ( 'NONE',  ( 0.000000000000000000, 0.000000000000000000, -1.000000000000000000 ) ) ;
#26577 = VECTOR ( 'NONE', #32915, 1000.000000000000000 ) ;
#26578 = VECTOR ( 'NONE', #32935, 1000.000000000000114 ) ;
#26580 = CIRCLE ( 'NONE', #1421, 125.0000000000000000 ) ;
#26579 = FACE_OUTER_BOUND ( 'NONE', #1104, .T. ) ;
#26581 = CARTESIAN_POINT ( 'NONE',  ( -63.09433862318517328, -175.3837268820161057, -124.1426420773539689 ) ) ;
#26582 = ORIENTED_EDGE ( 'NONE', *, *, #7502, .T. ) ;
#26583 = VECTOR ( 'NONE', #48389, 1000.000000000000000 ) ;
#26584 = EDGE_CURVE ( 'NONE', #48562, #38308, #42005, .T. ) ;
#26585 = CARTESIAN_POINT ( 'NONE',  ( -305.0000000000000568, -131.2283041299246520, -59.50019592636137844 ) ) ;
#26586 = DIRECTION ( 'NONE',  ( -0.000000000000000000, 1.000000000000000000, -0.000000000000000000 ) ) ;
#26589 = ORIENTED_EDGE ( 'NONE', *, *, #28824, .T. ) ;
#26588 = FACE_OUTER_BOUND ( 'NONE', #25423, .T. ) ;
#26587 = DIRECTION ( 'NONE',  ( 0.000000000000000000, -1.000000000000000000, 0.000000000000000000 ) ) ;
#26590 = DIRECTION ( 'NONE',  ( 0.000000000000000000, 0.000000000000000000, 1.000000000000000000 ) ) ;
#26591 = ORIENTED_EDGE ( 'NONE', *, *, #44358, .T. ) ;
#26592 = CARTESIAN_POINT ( 'NONE',  ( -305.0000000000000568, -169.4764303083190384, -38.55084767037274673 ) ) ;
#26593 = ORIENTED_EDGE ( 'NONE', *, *, #18951, .F. ) ;
#26594 = EDGE_CURVE ( 'NONE', #14763, #30653, #46258, .T. ) ;
#26595 = EDGE_CURVE ( 'NONE', #46596, #16650, #42032, .T. ) ;
#26596 = EDGE_CURVE ( 'NONE', #6882, #14387, #922, .T. ) ;
#26597 = DIRECTION ( 'NONE',  ( -0.000000000000000000, 0.9709418174260492362, -0.2393156642875685636 ) ) ;
#26598 = CARTESIAN_POINT ( 'NONE',  ( 69.99104047056317768, -193.5000000000000000, -39.87254040532513244 ) ) ;
#26599 = CARTESIAN_POINT ( 'NONE',  ( -158.0280232639029236, -189.7472609257535510, 60.19999396110247858 ) ) ;
#26600 = ADVANCED_FACE ( 'NONE', ( #38062 ), #34635, .F. ) ;
#26601 = AXIS2_PLACEMENT_3D ( 'NONE', #1148, #4582, #48490 ) ;
#26602 = VERTEX_POINT ( 'NONE', #35408 ) ;
#26603 = DIRECTION ( 'NONE',  ( 0.000000000000000000, 1.000000000000000000, -0.000000000000000000 ) ) ;
#26604 = VECTOR ( 'NONE', #18431, 1000.000000000000000 ) ;
#26605 = PLANE ( 'NONE',  #51909 ) ;
#26606 = VERTEX_POINT ( 'NONE', #30688 ) ;
#26607 = ADVANCED_FACE ( 'NONE', ( #7053 ), #6797, .F. ) ;
#26608 = DIRECTION ( 'NONE',  ( 0.000000000000000000, 1.000000000000000000, 0.000000000000000000 ) ) ;
#26609 = AXIS2_PLACEMENT_3D ( 'NONE', #65, #47658, #44219 ) ;
#26610 = DIRECTION ( 'NONE',  ( 0.000000000000000000, -1.000000000000000000, 0.000000000000000000 ) ) ;
#26611 = VERTEX_POINT ( 'NONE', #19140 ) ;
#26612 = FACE_BOUND ( 'NONE', #11308, .T. ) ;
#26613 = EDGE_CURVE ( 'NONE', #45175, #3688, #43303, .T. ) ;
#26614 = DIRECTION ( 'NONE',  ( 0.000000000000000000, 0.000000000000000000, -1.000000000000000000 ) ) ;
#26615 = EDGE_CURVE ( 'NONE', #15638, #1527, #26126, .T. ) ;
#26616 = ORIENTED_EDGE ( 'NONE', *, *, #36879, .F. ) ;
#26617 = CARTESIAN_POINT ( 'NONE',  ( 33.25242634436024503, -193.5000000000000000, -94.57776286494160445 ) ) ;
#26618 = ORIENTED_EDGE ( 'NONE', *, *, #17028, .T. ) ;
#26619 = VECTOR ( 'NONE', #26175, 1000.000000000000000 ) ;
#26620 = EDGE_CURVE ( 'NONE', #50992, #3704, #7312, .T. ) ;
#26621 = DIRECTION ( 'NONE',  ( -0.000000000000000000, 1.000000000000000000, -0.000000000000000000 ) ) ;
#26622 = AXIS2_PLACEMENT_3D ( 'NONE', #31829, #47866, #12087 ) ;
#26623 = DIRECTION ( 'NONE',  ( 0.000000000000000000, 0.000000000000000000, -1.000000000000000000 ) ) ;
#26624 = ORIENTED_EDGE ( 'NONE', *, *, #46503, .F. ) ;
#26625 = AXIS2_PLACEMENT_3D ( 'NONE', #32612, #11846, #281 ) ;
#26626 = EDGE_CURVE ( 'NONE', #1404, #8692, #2840, .T. ) ;
#26627 = CARTESIAN_POINT ( 'NONE',  ( -48.47912675150885065, -177.1207230881787780, 6.938893903907228378E-15 ) ) ;
#26628 = DIRECTION ( 'NONE',  ( -0.000000000000000000, 1.000000000000000000, -0.000000000000000000 ) ) ;
#26629 = LINE ( 'NONE', #47123, #26563 ) ;
#26630 = AXIS2_PLACEMENT_3D ( 'NONE', #553, #24223, #37073 ) ;
#26631 = EDGE_CURVE ( 'NONE', #12833, #46014, #23077, .T. ) ;
#26632 = ORIENTED_EDGE ( 'NONE', *, *, #26631, .F. ) ;
#26634 = AXIS2_PLACEMENT_3D ( 'NONE', #42621, #51048, #14778 ) ;
#26633 = CARTESIAN_POINT ( 'NONE',  ( -23.99795575808070325, -177.1207230881787780, -122.5792489240757561 ) ) ;
#26635 = ADVANCED_FACE ( 'NONE', ( #47264 ), #35158, .F. ) ;
#26636 = CARTESIAN_POINT ( 'NONE',  ( -330.4913330509368166, -123.5000000000000284, 0.000000000000000000 ) ) ;
#26637 = CARTESIAN_POINT ( 'NONE',  ( 2.347046875550483230E-15, 20.00000000000000000, 51.00000000000000711 ) ) ;
#26639 = EDGE_LOOP ( 'NONE', ( #45372, #31720, #15474, #6315 ) ) ;
#26638 = CARTESIAN_POINT ( 'NONE',  ( -164.6246685127424882, -189.7472609257535510, -46.20836643930983456 ) ) ;
#26640 = VERTEX_POINT ( 'NONE', #43814 ) ;
#26641 = DIRECTION ( 'NONE',  ( -1.000000000000000000, -0.000000000000000000, -0.000000000000000000 ) ) ;
#26642 = ADVANCED_FACE ( 'NONE', ( #15727 ), #3360, .T. ) ;
#26643 = DIRECTION ( 'NONE',  ( 0.000000000000000000, -1.000000000000000000, 0.000000000000000000 ) ) ;
#26644 = VECTOR ( 'NONE', #8961, 1000.000000000000000 ) ;
#26645 = CIRCLE ( 'NONE', #3988, 125.0000000000000000 ) ;
#26646 = VERTEX_POINT ( 'NONE', #3101 ) ;
#26647 = CARTESIAN_POINT ( 'NONE',  ( -169.3144491972411458, -183.6283474603465606, -27.83926365844663664 ) ) ;
#26648 = ORIENTED_EDGE ( 'NONE', *, *, #264, .T. ) ;
#26649 = CARTESIAN_POINT ( 'NONE',  ( -305.0000000000000568, -149.0257676989619142, 54.29949524055110999 ) ) ;
#26650 = CARTESIAN_POINT ( 'NONE',  ( -172.7479958471414250, -193.5000000000000000, -13.49993235881364129 ) ) ;
#26651 = VECTOR ( 'NONE', #42272, 1000.000000000000000 ) ;
#26652 = LINE ( 'NONE', #51351, #40379 ) ;
#26653 = CARTESIAN_POINT ( 'NONE',  ( -339.1964088526558498, -71.02573290043838483, 26.97593913775504504 ) ) ;
#26654 = ORIENTED_EDGE ( 'NONE', *, *, #41683, .F. ) ;
#26655 = ORIENTED_EDGE ( 'NONE', *, *, #30676, .T. ) ;
#26656 = ORIENTED_EDGE ( 'NONE', *, *, #14951, .F. ) ;
#26657 = PLANE ( 'NONE',  #35020 ) ;
#26658 = CARTESIAN_POINT ( 'NONE',  ( 56.81546028627039391, -175.3837268820161057, 65.49088066501711580 ) ) ;
#26659 = VECTOR ( 'NONE', #7519, 1000.000000000000000 ) ;
#26660 = VECTOR ( 'NONE', #20251, 1000.000000000000000 ) ;
#26661 = VECTOR ( 'NONE', #25895, 1000.000000000000000 ) ;
#26662 = DIRECTION ( 'NONE',  ( 0.000000000000000000, 1.000000000000000000, 0.000000000000000000 ) ) ;
#26663 = DIRECTION ( 'NONE',  ( -0.000000000000000000, 1.000000000000000000, -0.000000000000000000 ) ) ;
#26664 = ORIENTED_EDGE ( 'NONE', *, *, #9108, .F. ) ;
#26665 = EDGE_CURVE ( 'NONE', #15769, #3536, #24443, .T. ) ;
#26666 = ADVANCED_FACE ( 'NONE', ( #39355 ), #19390, .T. ) ;
#26667 = VECTOR ( 'NONE', #16810, 1000.000000000000000 ) ;
#26668 = CARTESIAN_POINT ( 'NONE',  ( -48.30901192927175458, -175.3837268820161057, -124.9998842437354227 ) ) ;
#26669 = LINE ( 'NONE', #22723, #2208 ) ;
#26670 = ADVANCED_FACE ( 'NONE', ( #14953 ), #47003, .T. ) ;
#26671 = CIRCLE ( 'NONE', #35934, 125.0000000000000000 ) ;
#26672 = ADVANCED_FACE ( 'NONE', ( #7563 ), #43047, .F. ) ;
#26673 = ORIENTED_EDGE ( 'NONE', *, *, #35426, .F. ) ;
#26674 = ORIENTED_EDGE ( 'NONE', *, *, #11042, .F. ) ;
#26675 = CARTESIAN_POINT ( 'NONE',  ( 0.000000000000000000, -130.6116641350643022, -58.56982357178517873 ) ) ;
#26676 = LINE ( 'NONE', #18527, #4025 ) ;
#26677 = CARTESIAN_POINT ( 'NONE',  ( -48.47912675150885065, -183.6283474603465606, 6.938893903907228378E-15 ) ) ;
#26678 = DIRECTION ( 'NONE',  ( -0.9008942672012966169, 0.4327645661435913227, -0.03323175611351236042 ) ) ;
#26679 = PLANE ( 'NONE',  #45293 ) ;
#26680 = ORIENTED_EDGE ( 'NONE', *, *, #27543, .F. ) ;
#26681 = CARTESIAN_POINT ( 'NONE',  ( -48.47912675150885065, -177.1207230881787780, 6.938893903907228378E-15 ) ) ;
#26682 = VERTEX_POINT ( 'NONE', #3613 ) ;
#26683 = DIRECTION ( 'NONE',  ( 0.2348860457809911206, 0.000000000000000000, -0.9720229140804089729 ) ) ;
#26684 = VECTOR ( 'NONE', #16206, 1000.000000000000000 ) ;
#26685 = EDGE_CURVE ( 'NONE', #51763, #32514, #31153, .T. ) ;
#26686 = CARTESIAN_POINT ( 'NONE',  ( -336.3521761649654422, -123.5000000000000284, 0.000000000000000000 ) ) ;
#26687 = ORIENTED_EDGE ( 'NONE', *, *, #42248, .T. ) ;
#26688 = VECTOR ( 'NONE', #42678, 1000.000000000000114 ) ;
#26689 = PLANE ( 'NONE',  #27358 ) ;
#26690 = DIRECTION ( 'NONE',  ( 0.000000000000000000, 0.8229838658936634577, 0.5680647467311457088 ) ) ;
#26691 = DIRECTION ( 'NONE',  ( 0.8124868780056742068, 0.000000000000000000, 0.5829794791144820021 ) ) ;
#26692 = FACE_OUTER_BOUND ( 'NONE', #34526, .T. ) ;
#26693 = ADVANCED_FACE ( 'NONE', ( #27776 ), #3883, .F. ) ;
#26694 = CYLINDRICAL_SURFACE ( 'NONE', #8524, 125.0000000000000000 ) ;
#26695 = ORIENTED_EDGE ( 'NONE', *, *, #22467, .T. ) ;
#26696 = CIRCLE ( 'NONE', #19976, 125.0000000000000000 ) ;
#26697 = DIRECTION ( 'NONE',  ( 0.000000000000000000, 0.000000000000000000, 1.000000000000000000 ) ) ;
#26698 = ORIENTED_EDGE ( 'NONE', *, *, #29929, .F. ) ;
#26699 = ORIENTED_EDGE ( 'NONE', *, *, #5117, .T. ) ;
#26700 = CARTESIAN_POINT ( 'NONE',  ( -164.3791542526839464, -189.7472609257535510, 46.82076062204520639 ) ) ;
#26701 = VERTEX_POINT ( 'NONE', #10733 ) ;
#26702 = AXIS2_PLACEMENT_3D ( 'NONE', #7586, #32010, #39882 ) ;
#26703 = CARTESIAN_POINT ( 'NONE',  ( -145.6517069852672535, -175.3837268820161057, 78.62880929222943394 ) ) ;
#26704 = VERTEX_POINT ( 'NONE', #26758 ) ;
#26705 = DIRECTION ( 'NONE',  ( -1.000000000000000000, 0.000000000000000000, 0.000000000000000000 ) ) ;
#26706 = CARTESIAN_POINT ( 'NONE',  ( -332.3517673607765914, -113.7752393642576720, 58.25253621232167944 ) ) ;
#26707 = ORIENTED_EDGE ( 'NONE', *, *, #44293, .F. ) ;
#26708 = CARTESIAN_POINT ( 'NONE',  ( -129.9529520667707914, -175.3837268820161057, -94.79987230211960991 ) ) ;
#26709 = DIRECTION ( 'NONE',  ( 0.000000000000000000, 0.000000000000000000, 1.000000000000000000 ) ) ;
#26710 = FACE_OUTER_BOUND ( 'NONE', #515, .T. ) ;
#26711 = VERTEX_POINT ( 'NONE', #45140 ) ;
#26712 = ORIENTED_EDGE ( 'NONE', *, *, #49729, .T. ) ;
#26713 = EDGE_LOOP ( 'NONE', ( #2999, #18662, #24148, #28802 ) ) ;
#26714 = LINE ( 'NONE', #50903, #33458 ) ;
#26715 = CIRCLE ( 'NONE', #32569, 125.0000000000000000 ) ;
#26716 = DIRECTION ( 'NONE',  ( -0.1476465640024779702, 0.000000000000000000, -0.9890401873221644768 ) ) ;
#26717 = CARTESIAN_POINT ( 'NONE',  ( -336.3521761649654422, -118.0087234915157381, -58.76657425099333665 ) ) ;
#26718 = FACE_OUTER_BOUND ( 'NONE', #17235, .T. ) ;
#26719 = VERTEX_POINT ( 'NONE', #16492 ) ;
#26720 = VECTOR ( 'NONE', #18959, 1000.000000000000114 ) ;
#26721 = EDGE_CURVE ( 'NONE', #48670, #2027, #20955, .T. ) ;
#26722 = CARTESIAN_POINT ( 'NONE',  ( -332.3517673607765914, -87.81784868886214213, 47.06073758877343494 ) ) ;
#26723 = VERTEX_POINT ( 'NONE', #36438 ) ;
#26725 = VERTEX_POINT ( 'NONE', #32769 ) ;
#26724 = CYLINDRICAL_SURFACE ( 'NONE', #41576, 125.0000000000000000 ) ;
#26726 = AXIS2_PLACEMENT_3D ( 'NONE', #9649, #980, #5974 ) ;
#26727 = ORIENTED_EDGE ( 'NONE', *, *, #21803, .T. ) ;
#26728 = DIRECTION ( 'NONE',  ( 0.08879589532293853671, 0.000000000000000000, -0.9960498426152166740 ) ) ;
#26729 = CARTESIAN_POINT ( 'NONE',  ( -336.3521761649654422, -165.9166037625627439, 41.09453333279358134 ) ) ;
#26730 = CARTESIAN_POINT ( 'NONE',  ( -48.47912675150885065, -213.5000000000000000, 6.938893903907228378E-15 ) ) ;
#26731 = DIRECTION ( 'NONE',  ( 0.000000000000000000, 0.000000000000000000, 1.000000000000000000 ) ) ;
#26732 = VERTEX_POINT ( 'NONE', #438 ) ;
#26733 = PLANE ( 'NONE',  #27534 ) ;
#26734 = ORIENTED_EDGE ( 'NONE', *, *, #20922, .T. ) ;
#26735 = CIRCLE ( 'NONE', #23367, 125.0000000000000000 ) ;
#26736 = ORIENTED_EDGE ( 'NONE', *, *, #17617, .T. ) ;
#26737 = CARTESIAN_POINT ( 'NONE',  ( 20.93410174202488250, -193.5000000000000000, -102.7511748916624725 ) ) ;
#26738 = CARTESIAN_POINT ( 'NONE',  ( 68.79964045138289919, -193.5000000000000000, 43.25148278810711133 ) ) ;
#26739 = EDGE_CURVE ( 'NONE', #50099, #43619, #48815, .T. ) ;
#26740 = DIRECTION ( 'NONE',  ( -0.000000000000000000, 1.000000000000000000, 0.000000000000000000 ) ) ;
#26741 = DIRECTION ( 'NONE',  ( 1.000000000000000000, -0.000000000000000000, -0.000000000000000000 ) ) ;
#26742 = EDGE_LOOP ( 'NONE', ( #34432, #8010, #21497, #28975 ) ) ;
#26743 = DIRECTION ( 'NONE',  ( -0.000000000000000000, 0.8854560256532093554, -0.4647231720437695057 ) ) ;
#26744 = LINE ( 'NONE', #42780, #23087 ) ;
#26745 = PLANE ( 'NONE',  #50676 ) ;
#26746 = CARTESIAN_POINT ( 'NONE',  ( 68.59638248015002659, -183.6283474603465606, -43.79868877201407429 ) ) ;
#26747 = ORIENTED_EDGE ( 'NONE', *, *, #19919, .F. ) ;
#26748 = CARTESIAN_POINT ( 'NONE',  ( -114.9451385648676478, -193.5000000000000000, -104.6823626202119470 ) ) ;
#26749 = CARTESIAN_POINT ( 'NONE',  ( 46.00000000000000711, 35.00000000000000000, -56.99999999999999289 ) ) ;
#26750 = EDGE_CURVE ( 'NONE', #17878, #36957, #36179, .T. ) ;
#26751 = FACE_BOUND ( 'NONE', #31610, .T. ) ;
#26752 = AXIS2_PLACEMENT_3D ( 'NONE', #19962, #47054, #11558 ) ;
#26753 = ORIENTED_EDGE ( 'NONE', *, *, #8922, .T. ) ;
#26754 = AXIS2_PLACEMENT_3D ( 'NONE', #20529, #3997, #23695 ) ;
#26755 = VECTOR ( 'NONE', #12810, 1000.000000000000000 ) ;
#26756 = LINE ( 'NONE', #7562, #18881 ) ;
#26757 = AXIS2_PLACEMENT_3D ( 'NONE', #23096, #1827, #14445 ) ;
#26758 = CARTESIAN_POINT ( 'NONE',  ( 75.10200014432449223, -175.3837268820161057, 10.18383939837613639 ) ) ;
#26759 = ORIENTED_EDGE ( 'NONE', *, *, #36055, .F. ) ;
#26760 = CARTESIAN_POINT ( 'NONE',  ( 17.98688506184921465, -183.6283474603465606, 104.6823626202124444 ) ) ;
#26761 = EDGE_CURVE ( 'NONE', #34090, #1807, #24888, .T. ) ;
#26762 = ORIENTED_EDGE ( 'NONE', *, *, #8310, .T. ) ;
#26763 = VECTOR ( 'NONE', #13846, 1000.000000000000114 ) ;
#26764 = DIRECTION ( 'NONE',  ( -1.000000000000000000, -3.701062773504815647E-15, 9.758900497077172511E-15 ) ) ;
#26765 = FACE_OUTER_BOUND ( 'NONE', #51519, .T. ) ;
#26766 = DIRECTION ( 'NONE',  ( 0.000000000000000000, 0.000000000000000000, 1.000000000000000000 ) ) ;
#26767 = PLANE ( 'NONE',  #10704 ) ;
#26768 = PLANE ( 'NONE',  #10956 ) ;
#26769 = ORIENTED_EDGE ( 'NONE', *, *, #6763, .F. ) ;
#26770 = VECTOR ( 'NONE', #27238, 1000.000000000000000 ) ;
#26771 = DIRECTION ( 'NONE',  ( -1.000000000000000000, 0.000000000000000000, -0.000000000000000000 ) ) ;
#26772 = ADVANCED_FACE ( 'NONE', ( #49065 ), #28811, .T. ) ;
#26773 = VERTEX_POINT ( 'NONE', #25157 ) ;
#26774 = FACE_OUTER_BOUND ( 'NONE', #21316, .T. ) ;
#26775 = EDGE_LOOP ( 'NONE', ( #42760, #41243, #32972, #9159 ) ) ;
#26776 = CARTESIAN_POINT ( 'NONE',  ( -340.0000000000000568, -123.5000000000000284, 0.000000000000000000 ) ) ;
#26777 = EDGE_CURVE ( 'NONE', #40297, #12556, #48561, .T. ) ;
#26778 = CARTESIAN_POINT ( 'NONE',  ( -173.4190745413846457, -175.3837268820161057, -3.874202661594927211 ) ) ;
#26779 = ORIENTED_EDGE ( 'NONE', *, *, #40971, .T. ) ;
#26782 = ORIENTED_EDGE ( 'NONE', *, *, #40521, .F. ) ;
#26781 = DIRECTION ( 'NONE',  ( -0.000000000000000000, 1.000000000000000000, -0.000000000000000000 ) ) ;
#26780 = CARTESIAN_POINT ( 'NONE',  ( 36.84288420123323249, -183.6283474603465606, 91.35181687837503262 ) ) ;
#26783 = EDGE_CURVE ( 'NONE', #22586, #875, #42895, .T. ) ;
#26784 = CIRCLE ( 'NONE', #33518, 125.0000000000000000 ) ;
#26785 = LINE ( 'NONE', #11006, #22274 ) ;
#26786 = EDGE_LOOP ( 'NONE', ( #46788, #44500, #48325, #1844 ) ) ;
#26787 = DIRECTION ( 'NONE',  ( 0.000000000000000000, 0.000000000000000000, 1.000000000000000000 ) ) ;
#26788 = ORIENTED_EDGE ( 'NONE', *, *, #13377, .T. ) ;
#26789 = DIRECTION ( 'NONE',  ( 1.000000000000000000, -0.000000000000000000, -0.000000000000000000 ) ) ;
#26792 = ORIENTED_EDGE ( 'NONE', *, *, #25248, .F. ) ;
#26791 = FACE_OUTER_BOUND ( 'NONE', #2002, .T. ) ;
#26790 = DIRECTION ( 'NONE',  ( -1.000000000000000000, 0.000000000000000000, 0.000000000000000000 ) ) ;
#26793 = ORIENTED_EDGE ( 'NONE', *, *, #21336, .F. ) ;
#26794 = DIRECTION ( 'NONE',  ( 0.000000000000000000, 1.000000000000000000, -0.000000000000000000 ) ) ;
#26795 = ORIENTED_EDGE ( 'NONE', *, *, #16404, .F. ) ;
#26796 = PLANE ( 'NONE',  #47182 ) ;
#26797 = LINE ( 'NONE', #14724, #3009 ) ;
#26798 = EDGE_LOOP ( 'NONE', ( #9046, #27115 ) ) ;
#26799 = ADVANCED_FACE ( 'NONE', ( #9127 ), #16766, .T. ) ;
#26800 = LINE ( 'NONE', #50479, #16300 ) ;
#26801 = DIRECTION ( 'NONE',  ( 1.000000000000000000, -0.000000000000000000, 0.000000000000000000 ) ) ;
#26802 = DIRECTION ( 'NONE',  ( 0.000000000000000000, -1.000000000000000000, 0.000000000000000000 ) ) ;
#26803 = PLANE ( 'NONE',  #20095 ) ;
#26804 = CARTESIAN_POINT ( 'NONE',  ( -34.63763967761165929, -193.5000000000000000, -123.2250735253142864 ) ) ;
#26805 = VERTEX_POINT ( 'NONE', #15974 ) ;
#26806 = CARTESIAN_POINT ( 'NONE',  ( -41.24387117724851493, -175.3837268820161057, 124.7904286264581231 ) ) ;
#26807 = CARTESIAN_POINT ( 'NONE',  ( -336.3521761649654422, -113.7752393642576720, 58.25253621232167944 ) ) ;
#26808 = CIRCLE ( 'NONE', #22625, 60.00000000000000000 ) ;
#26809 = CARTESIAN_POINT ( 'NONE',  ( -48.02249751411514467, -175.3837268820161057, 0.8896570909947569827 ) ) ;
#26810 = ORIENTED_EDGE ( 'NONE', *, *, #14448, .F. ) ;
#26811 = CARTESIAN_POINT ( 'NONE',  ( 29.27398957514434130, -193.5000000000000000, -97.87467957287998388 ) ) ;
#26812 = CARTESIAN_POINT ( 'NONE',  ( -48.47912675150885065, -177.1207230881787780, 6.938893903907228378E-15 ) ) ;
#26813 = DIRECTION ( 'NONE',  ( 1.000000000000000000, -0.000000000000000000, -0.000000000000000000 ) ) ;
#26814 = LINE ( 'NONE', #50241, #36108 ) ;
#26815 = DIRECTION ( 'NONE',  ( -0.000000000000000000, 1.000000000000000000, -0.000000000000000000 ) ) ;
#26816 = ORIENTED_EDGE ( 'NONE', *, *, #27479, .F. ) ;
#26817 = CARTESIAN_POINT ( 'NONE',  ( -339.1964088526558498, -150.4759391377552618, 52.47426709956155122 ) ) ;
#26818 = CARTESIAN_POINT ( 'NONE',  ( -48.47912675150885065, -175.3837268820161057, 6.938893903907228378E-15 ) ) ;
#26819 = AXIS2_PLACEMENT_3D ( 'NONE', #8286, #47723, #24829 ) ;
#26820 = CARTESIAN_POINT ( 'NONE',  ( -80.17897391495031911, -183.6283474603465606, 120.9136869416132498 ) ) ;
#26821 = PLANE ( 'NONE',  #39652 ) ;
#26822 = FACE_OUTER_BOUND ( 'NONE', #24025, .T. ) ;
#26823 = ORIENTED_EDGE ( 'NONE', *, *, #28506, .T. ) ;
#26824 = ADVANCED_FACE ( 'NONE', ( #181 ), #36972, .T. ) ;
#26825 = ADVANCED_FACE ( 'NONE', ( #32513 ), #12007, .F. ) ;
#26826 = LINE ( 'NONE', #4875, #49545 ) ;
#26827 = CARTESIAN_POINT ( 'NONE',  ( -47.53180039765466347, -189.7472609257535510, 0.3202698538628485636 ) ) ;
#26828 = ORIENTED_EDGE ( 'NONE', *, *, #2209, .T. ) ;
#26829 = ORIENTED_EDGE ( 'NONE', *, *, #14564, .T. ) ;
#26830 = ORIENTED_EDGE ( 'NONE', *, *, #6738, .T. ) ;
#26831 = DIRECTION ( 'NONE',  ( -0.000000000000000000, 1.000000000000000000, -0.000000000000000000 ) ) ;
#26832 = EDGE_CURVE ( 'NONE', #48811, #15941, #11863, .T. ) ;
#26833 = DIRECTION ( 'NONE',  ( 0.000000000000000000, 1.000000000000000000, -0.000000000000000000 ) ) ;
#26834 = DIRECTION ( 'NONE',  ( 0.000000000000000000, -1.000000000000000000, -0.000000000000000000 ) ) ;
#26835 = ORIENTED_EDGE ( 'NONE', *, *, #29172, .T. ) ;
#26836 = EDGE_CURVE ( 'NONE', #6242, #20290, #24368, .T. ) ;
#26837 = VECTOR ( 'NONE', #45408, 1000.000000000000227 ) ;
#26838 = AXIS2_PLACEMENT_3D ( 'NONE', #40312, #39539, #28745 ) ;
#26839 = LINE ( 'NONE', #38920, #40973 ) ;
#26840 = CARTESIAN_POINT ( 'NONE',  ( 14.94072793302542124, -189.7472609257535510, 107.7168604805791574 ) ) ;
#26843 = ORIENTED_EDGE ( 'NONE', *, *, #7686, .F. ) ;
#26842 = DIRECTION ( 'NONE',  ( 0.9960498426152177842, 0.000000000000000000, -0.08879589532292482545 ) ) ;
#26841 = CARTESIAN_POINT ( 'NONE',  ( -332.3517673607765914, -64.61288906875131488, 4.498567634385603142 ) ) ;
#26844 = ADVANCED_FACE ( 'NONE', ( #40373 ), #4393, .F. ) ;
#26845 = CARTESIAN_POINT ( 'NONE',  ( -305.0000000000000568, -81.78065195202965754, 43.12187378178632002 ) ) ;
#26846 = VERTEX_POINT ( 'NONE', #40632 ) ;
#26847 = CARTESIAN_POINT ( 'NONE',  ( -173.3968853974275817, -189.7472609257535510, 4.533605064404221174 ) ) ;
#26848 = ORIENTED_EDGE ( 'NONE', *, *, #25364, .F. ) ;
#26849 = DIRECTION ( 'NONE',  ( 0.000000000000000000, -0.8660254037844354880, -0.5000000000000054401 ) ) ;
#26850 = DIRECTION ( 'NONE',  ( 0.000000000000000000, 0.000000000000000000, 1.000000000000000000 ) ) ;
#26851 = PLANE ( 'NONE',  #25736 ) ;
#26852 = VERTEX_POINT ( 'NONE', #4654 ) ;
#26853 = ORIENTED_EDGE ( 'NONE', *, *, #37505, .F. ) ;
#26854 = DIRECTION ( 'NONE',  ( 0.000000000000000000, 0.000000000000000000, 1.000000000000000000 ) ) ;
#26856 = VECTOR ( 'NONE', #18950, 1000.000000000000000 ) ;
#26855 = DIRECTION ( 'NONE',  ( 0.000000000000000000, 0.000000000000000000, 1.000000000000000000 ) ) ;
#26857 = ORIENTED_EDGE ( 'NONE', *, *, #35305, .F. ) ;
#26858 = CARTESIAN_POINT ( 'NONE',  ( -336.3521761649654422, -100.1170788342122080, 54.23253582808833073 ) ) ;
#26859 = CARTESIAN_POINT ( 'NONE',  ( -339.1964088526558498, -138.3439121830091665, 58.13482838284733845 ) ) ;
#26860 = VERTEX_POINT ( 'NONE', #20684 ) ;
#26861 = FACE_BOUND ( 'NONE', #32167, .T. ) ;
#26862 = FACE_OUTER_BOUND ( 'NONE', #35906, .T. ) ;
#26863 = ORIENTED_EDGE ( 'NONE', *, *, #47879, .T. ) ;
#26864 = DIRECTION ( 'NONE',  ( -0.000000000000000000, 1.000000000000000000, -0.000000000000000000 ) ) ;
#26865 = EDGE_LOOP ( 'NONE', ( #20519, #26654, #11026, #39760 ) ) ;
#26866 = PLANE ( 'NONE',  #13058 ) ;
#26867 = LINE ( 'NONE', #46872, #11075 ) ;
#26868 = ORIENTED_EDGE ( 'NONE', *, *, #44217, .F. ) ;
#26869 = CARTESIAN_POINT ( 'NONE',  ( -60.00000000000000000, 0.000000000000000000, -60.00000000000000711 ) ) ;
#26870 = LINE ( 'NONE', #27128, #2907 ) ;
#26871 = CARTESIAN_POINT ( 'NONE',  ( -336.3521761649654422, -133.2247606357419443, -58.25253621232173629 ) ) ;
#26872 = VECTOR ( 'NONE', #36605, 1000.000000000000227 ) ;
#26873 = ORIENTED_EDGE ( 'NONE', *, *, #27148, .T. ) ;
#26874 = CIRCLE ( 'NONE', #37800, 125.0000000000000000 ) ;
#26875 = FACE_OUTER_BOUND ( 'NONE', #49798, .T. ) ;
#26876 = CARTESIAN_POINT ( 'NONE',  ( 68.24201764719070695, -193.5000000000000000, -44.73448837594909833 ) ) ;
#26877 = DIRECTION ( 'NONE',  ( -1.000000000000000000, 0.000000000000000000, -0.000000000000000000 ) ) ;
#26879 = EDGE_LOOP ( 'NONE', ( #29327, #50636, #5915, #46533 ) ) ;
#26878 = CARTESIAN_POINT ( 'NONE',  ( -180.0000000000000568, -123.5000000000000284, 45.63467731922665394 ) ) ;
#26880 = EDGE_CURVE ( 'NONE', #13363, #40758, #36720, .T. ) ;
#26881 = EDGE_LOOP ( 'NONE', ( #12092, #3762, #35815, #45291 ) ) ;
#26882 = EDGE_CURVE ( 'NONE', #26711, #23372, #47113, .T. ) ;
#26883 = ADVANCED_FACE ( 'NONE', ( #10344 ), #34761, .T. ) ;
#26884 = FACE_OUTER_BOUND ( 'NONE', #30857, .T. ) ;
#26885 = EDGE_CURVE ( 'NONE', #42243, #29510, #38190, .T. ) ;
#26886 = FACE_OUTER_BOUND ( 'NONE', #29355, .T. ) ;
#26887 = ORIENTED_EDGE ( 'NONE', *, *, #14930, .F. ) ;
#26888 = ORIENTED_EDGE ( 'NONE', *, *, #37550, .F. ) ;
#26889 = AXIS2_PLACEMENT_3D ( 'NONE', #16506, #40146, #36194 ) ;
#26890 = CARTESIAN_POINT ( 'NONE',  ( -339.1964088526558498, -167.3305728129742249, 39.49849221029288060 ) ) ;
#26891 = EDGE_CURVE ( 'NONE', #39890, #21288, #42397, .T. ) ;
#26892 = ORIENTED_EDGE ( 'NONE', *, *, #42569, .F. ) ;
#26893 = DIRECTION ( 'NONE',  ( 0.6749830015182038956, 0.000000000000000000, 0.7378332790417333475 ) ) ;
#26894 = DIRECTION ( 'NONE',  ( 0.000000000000000000, 0.000000000000000000, -1.000000000000000000 ) ) ;
#26895 = EDGE_CURVE ( 'NONE', #11938, #17341, #38459, .T. ) ;
#26896 = EDGE_CURVE ( 'NONE', #27207, #33001, #49334, .T. ) ;
#26897 = DIRECTION ( 'NONE',  ( 0.000000000000000000, -0.5680647467311656929, -0.8229838658936495799 ) ) ;
#26898 = CARTESIAN_POINT ( 'NONE',  ( 19.33815737959698566, -183.6283474603465606, 105.0038855142078233 ) ) ;
#26899 = ORIENTED_EDGE ( 'NONE', *, *, #40119, .F. ) ;
#26900 = EDGE_LOOP ( 'NONE', ( #1989, #29728, #29569, #28364 ) ) ;
#26901 = ADVANCED_FACE ( 'NONE', ( #22175 ), #22951, .T. ) ;
#26902 = EDGE_LOOP ( 'NONE', ( #6525, #12923, #17616, #46576 ) ) ;
#26903 = ADVANCED_FACE ( 'NONE', ( #22443, #14822 ), #50309, .F. ) ;
#26904 = FACE_OUTER_BOUND ( 'NONE', #44707, .T. ) ;
#26905 = DIRECTION ( 'NONE',  ( -0.000000000000000000, -1.000000000000000000, 0.000000000000000000 ) ) ;
#26906 = DIRECTION ( 'NONE',  ( -0.8124868780056742068, 0.000000000000000000, -0.5829794791144820021 ) ) ;
#26907 = EDGE_CURVE ( 'NONE', #27896, #15221, #38708, .T. ) ;
#26908 = CARTESIAN_POINT ( 'NONE',  ( 72.68824389704326450, -189.7472609257535510, -26.35287080855459863 ) ) ;
#26909 = CARTESIAN_POINT ( 'NONE',  ( -87.28630321566649286, -183.6283474603465606, 118.8234112238818341 ) ) ;
#26910 = ORIENTED_EDGE ( 'NONE', *, *, #43159, .F. ) ;
#26911 = AXIS2_PLACEMENT_3D ( 'NONE', #39779, #3290, #19324 ) ;
#26912 = EDGE_CURVE ( 'NONE', #51763, #27930, #30311, .T. ) ;
#26913 = DIRECTION ( 'NONE',  ( -0.000000000000000000, 1.000000000000000000, 0.000000000000000000 ) ) ;
#26914 = DIRECTION ( 'NONE',  ( 0.000000000000000000, 1.000000000000000000, 0.000000000000000000 ) ) ;
#26915 = AXIS2_PLACEMENT_3D ( 'NONE', #49401, #44138, #24181 ) ;
#26916 = ORIENTED_EDGE ( 'NONE', *, *, #25885, .T. ) ;
#26917 = ORIENTED_EDGE ( 'NONE', *, *, #49994, .T. ) ;
#26918 = LINE ( 'NONE', #42947, #17299 ) ;
#26919 = CARTESIAN_POINT ( 'NONE',  ( -48.47912675150885065, -175.3837268820161057, 6.938893903907228378E-15 ) ) ;
#26920 = DIRECTION ( 'NONE',  ( 0.000000000000000000, 0.5000000000000012212, -0.8660254037844378194 ) ) ;
#26921 = PLANE ( 'NONE',  #24895 ) ;
#26922 = CARTESIAN_POINT ( 'NONE',  ( 38.71172987070728055, -193.5000000000000000, -89.56983042009262874 ) ) ;
#26923 = CARTESIAN_POINT ( 'NONE',  ( -336.3521761649654422, -172.9832938399466684, -32.17247266903247294 ) ) ;
#26924 = ORIENTED_EDGE ( 'NONE', *, *, #3173, .F. ) ;
#26925 = DIRECTION ( 'NONE',  ( 0.000000000000000000, -1.000000000000000000, -0.000000000000000000 ) ) ;
#26926 = EDGE_CURVE ( 'NONE', #29344, #28119, #46884, .T. ) ;
#26927 = ORIENTED_EDGE ( 'NONE', *, *, #16997, .F. ) ;
#26928 = LINE ( 'NONE', #9882, #36320 ) ;
#26929 = AXIS2_PLACEMENT_3D ( 'NONE', #2483, #22710, #50571 ) ;
#26930 = CARTESIAN_POINT ( 'NONE',  ( 38.01517884164424999, -175.3837268820161057, -88.85232316304831102 ) ) ;
#26931 = VERTEX_POINT ( 'NONE', #7175 ) ;
#26932 = CARTESIAN_POINT ( 'NONE',  ( -49.42645310536303782, -193.5000000000000000, -0.3202698538628417357 ) ) ;
#26933 = DIRECTION ( 'NONE',  ( -0.7175072570443395970, 0.000000000000000000, 0.6965510290629882695 ) ) ;
#26934 = DIRECTION ( 'NONE',  ( 1.000000000000000000, -0.000000000000000000, -0.000000000000000000 ) ) ;
#26935 = LINE ( 'NONE', #9057, #6481 ) ;
#26936 = DIRECTION ( 'NONE',  ( 1.000000000000000000, -7.175085443855040167E-17, 4.952603889764104279E-17 ) ) ;
#26937 = EDGE_CURVE ( 'NONE', #22804, #3919, #9339, .T. ) ;
#26938 = ORIENTED_EDGE ( 'NONE', *, *, #5649, .T. ) ;
#26939 = CARTESIAN_POINT ( 'NONE',  ( -330.4913330509368166, -130.1153096980145563, 58.63009191191294178 ) ) ;
#26941 = ORIENTED_EDGE ( 'NONE', *, *, #17013, .T. ) ;
#26940 = CARTESIAN_POINT ( 'NONE',  ( -336.3521761649654422, -179.5993808087905279, -18.46045550523168899 ) ) ;
#26942 = CIRCLE ( 'NONE', #35312, 125.0000000000000000 ) ;
#26943 = EDGE_CURVE ( 'NONE', #47521, #18519, #46299, .T. ) ;
#26944 = EDGE_LOOP ( 'NONE', ( #32060, #50715, #37632, #35725 ) ) ;
#26945 = EDGE_CURVE ( 'NONE', #21474, #20782, #30329, .T. ) ;
#26946 = PLANE ( 'NONE',  #21248 ) ;
#26947 = EDGE_CURVE ( 'NONE', #1492, #40253, #14403, .T. ) ;
#26948 = ORIENTED_EDGE ( 'NONE', *, *, #19209, .F. ) ;
#26949 = EDGE_CURVE ( 'NONE', #19447, #30532, #50557, .T. ) ;
#26950 = AXIS2_PLACEMENT_3D ( 'NONE', #11236, #42788, #46746 ) ;
#26951 = DIRECTION ( 'NONE',  ( -0.000000000000000000, -1.000000000000000000, 0.000000000000000000 ) ) ;
#26952 = EDGE_LOOP ( 'NONE', ( #47459, #7978, #24324, #1336, #28106, #17703, #28842, #32266, #31036, #35943, #32194, #10955, #21240, #21595, #35321, #13472 ) ) ;
#26953 = AXIS2_PLACEMENT_3D ( 'NONE', #119, #51651, #32703 ) ;
#26954 = FACE_OUTER_BOUND ( 'NONE', #41091, .T. ) ;
#26955 = CARTESIAN_POINT ( 'NONE',  ( 46.00000000000000711, 33.00000000000000000, -55.00000000000000000 ) ) ;
#26956 = VERTEX_POINT ( 'NONE', #27135 ) ;
#26957 = DIRECTION ( 'NONE',  ( -0.9646355819083614058, 0.000000000000000000, 0.2635871660690581320 ) ) ;
#26958 = ADVANCED_FACE ( 'NONE', ( #14557 ), #30562, .F. ) ;
#26959 = CARTESIAN_POINT ( 'NONE',  ( -330.4913330509368166, -95.17484985463171654, -52.89315522109019696 ) ) ;
#26960 = DIRECTION ( 'NONE',  ( 0.000000000000000000, 0.000000000000000000, 1.000000000000000000 ) ) ;
#26961 = ORIENTED_EDGE ( 'NONE', *, *, #8460, .T. ) ;
#26962 = VERTEX_POINT ( 'NONE', #17271 ) ;
#26963 = VERTEX_POINT ( 'NONE', #13322 ) ;
#26964 = FACE_OUTER_BOUND ( 'NONE', #11544, .T. ) ;
#26965 = DIRECTION ( 'NONE',  ( 0.000000000000000000, 0.000000000000000000, -1.000000000000000000 ) ) ;
#26966 = AXIS2_PLACEMENT_3D ( 'NONE', #43959, #48699, #7708 ) ;
#26967 = ADVANCED_FACE ( 'NONE', ( #29341 ), #45391, .T. ) ;
#26968 = DIRECTION ( 'NONE',  ( -0.2059786187411094538, 0.000000000000000000, 0.9785564922995017012 ) ) ;
#26969 = CARTESIAN_POINT ( 'NONE',  ( 0.000000000000000000, -84.37576316379256980, 44.16213414209452992 ) ) ;
#26970 = FACE_OUTER_BOUND ( 'NONE', #14429, .T. ) ;
#26971 = ORIENTED_EDGE ( 'NONE', *, *, #1293, .T. ) ;
#26972 = EDGE_CURVE ( 'NONE', #38711, #50590, #21970, .T. ) ;
#26973 = ADVANCED_FACE ( 'NONE', ( #31597 ), #43445, .T. ) ;
#26974 = DIRECTION ( 'NONE',  ( 0.000000000000000000, 1.000000000000000000, 0.000000000000000000 ) ) ;
#26975 = ORIENTED_EDGE ( 'NONE', *, *, #44287, .F. ) ;
#26976 =( REPRESENTATION_RELATIONSHIP ('NONE','NONE', #4578, #6277 ) REPRESENTATION_RELATIONSHIP_WITH_TRANSFORMATION ( #29649 )SHAPE_REPRESENTATION_RELATIONSHIP( ) );
#26978 = ORIENTED_EDGE ( 'NONE', *, *, #4657, .T. ) ;
#26977 = CARTESIAN_POINT ( 'NONE',  ( -330.4913330509368166, -178.8432607619609200, -20.45418021416661247 ) ) ;
#26979 = ORIENTED_EDGE ( 'NONE', *, *, #43271, .T. ) ;
#26980 = CARTESIAN_POINT ( 'NONE',  ( -280.0000000000000000, -153.5000000000000284, -59.99999999999999289 ) ) ;
#26981 = FACE_OUTER_BOUND ( 'NONE', #47269, .T. ) ;
#26982 = AXIS2_PLACEMENT_3D ( 'NONE', #48557, #958, #12532 ) ;
#26983 = PLANE ( 'NONE',  #1874 ) ;
#26984 = LINE ( 'NONE', #38807, #25104 ) ;
#26985 = ORIENTED_EDGE ( 'NONE', *, *, #2059, .T. ) ;
#26986 = FACE_OUTER_BOUND ( 'NONE', #46646, .T. ) ;
#26987 = ORIENTED_EDGE ( 'NONE', *, *, #46521, .T. ) ;
#26988 = CIRCLE ( 'NONE', #51357, 125.0000000000000000 ) ;
#26989 = EDGE_CURVE ( 'NONE', #38808, #51354, #11879, .T. ) ;
#26990 = ORIENTED_EDGE ( 'NONE', *, *, #4011, .F. ) ;
#26991 = DIRECTION ( 'NONE',  ( -0.000000000000000000, -0.9350162426854169428, -0.3546048870425300148 ) ) ;
#26992 = FACE_OUTER_BOUND ( 'NONE', #51315, .T. ) ;
#26993 = LINE ( 'NONE', #43029, #50087 ) ;
#26994 = ORIENTED_EDGE ( 'NONE', *, *, #1872, .F. ) ;
#26995 = DIRECTION ( 'NONE',  ( 0.9646355819083576311, 0.000000000000000000, 0.2635871660690715101 ) ) ;
#26996 = DIRECTION ( 'NONE',  ( -0.8455960035018199594, 0.000000000000000000, -0.5338233779648003940 ) ) ;
#26997 = CARTESIAN_POINT ( 'NONE',  ( -74.33510315702939408, -183.6283474603465606, -121.2748789083719032 ) ) ;
#26998 = CARTESIAN_POINT ( 'NONE',  ( -77.67449977936063021, -175.3837268820161057, -121.5427093402339267 ) ) ;
#26999 = ORIENTED_EDGE ( 'NONE', *, *, #16335, .T. ) ;
#27000 = FACE_OUTER_BOUND ( 'NONE', #50496, .T. ) ;
#27001 = DIRECTION ( 'NONE',  ( -0.000000000000000000, 0.9709418174260519008, -0.2393156642875582940 ) ) ;
#27002 = VECTOR ( 'NONE', #19511, 1000.000000000000000 ) ;
#27003 = CARTESIAN_POINT ( 'NONE',  ( -332.3517673607765914, -71.64707600775140861, -30.18731974611341684 ) ) ;
#27004 = EDGE_LOOP ( 'NONE', ( #29169, #41623, #34574, #50200 ) ) ;
#27005 = AXIS2_PLACEMENT_3D ( 'NONE', #33573, #45668, #2550 ) ;
#27006 = CARTESIAN_POINT ( 'NONE',  ( -59.86929868745820471, -177.1207230881787780, -124.4799742258549458 ) ) ;
#27007 = DIRECTION ( 'NONE',  ( 0.000000000000000000, 0.000000000000000000, 1.000000000000000000 ) ) ;
#27008 = ORIENTED_EDGE ( 'NONE', *, *, #41732, .F. ) ;
#27009 = EDGE_CURVE ( 'NONE', #16316, #7787, #7713, .T. ) ;
#27010 = DIRECTION ( 'NONE',  ( 1.000000000000000000, -0.000000000000000000, -0.000000000000000000 ) ) ;
#27011 = VERTEX_POINT ( 'NONE', #31338 ) ;
#27012 = PLANE ( 'NONE',  #24280 ) ;
#27013 = FACE_BOUND ( 'NONE', #25878, .T. ) ;
#27014 = DIRECTION ( 'NONE',  ( 0.000000000000000000, -1.346129392433909288E-16, 1.000000000000000000 ) ) ;
#27015 = AXIS2_PLACEMENT_3D ( 'NONE', #32865, #45748, #25004 ) ;
#27016 = AXIS2_PLACEMENT_3D ( 'NONE', #43937, #15575, #31589 ) ;
#27017 = DIRECTION ( 'NONE',  ( -0.05924062789371441901, 0.000000000000000000, 0.9982437317643214625 ) ) ;
#27018 = VERTEX_POINT ( 'NONE', #24245 ) ;
#27019 = VECTOR ( 'NONE', #12864, 1000.000000000000000 ) ;
#27020 = ORIENTED_EDGE ( 'NONE', *, *, #30115, .T. ) ;
#27021 = CARTESIAN_POINT ( 'NONE',  ( -332.3517673607765914, -167.3116148657362032, 40.99441916720375900 ) ) ;
#27022 = ORIENTED_EDGE ( 'NONE', *, *, #5754, .T. ) ;
#27023 = EDGE_CURVE ( 'NONE', #4313, #46169, #15320, .T. ) ;
#27024 = DIRECTION ( 'NONE',  ( 1.000000000000000000, -0.000000000000000000, -0.000000000000000000 ) ) ;
#27025 = VECTOR ( 'NONE', #25741, 1000.000000000000000 ) ;
#27026 = ADVANCED_FACE ( 'NONE', ( #43945 ), #11360, .T. ) ;
#27027 = DIRECTION ( 'NONE',  ( 0.000000000000000000, -0.000000000000000000, 1.000000000000000000 ) ) ;
#27028 = CARTESIAN_POINT ( 'NONE',  ( -330.4913330509368166, -172.5932850007659169, -34.49419324804648568 ) ) ;
#27029 = ORIENTED_EDGE ( 'NONE', *, *, #12136, .F. ) ;
#27032 = ORIENTED_EDGE ( 'NONE', *, *, #946, .T. ) ;
#27031 = DIRECTION ( 'NONE',  ( -0.000000000000000000, 1.000000000000000000, 0.000000000000000000 ) ) ;
#27030 = CARTESIAN_POINT ( 'NONE',  ( -4.322350346021930356, 55.11748258468679751, -17.91176154419416378 ) ) ;
#27033 = AXIS2_PLACEMENT_3D ( 'NONE', #22564, #14666, #38314 ) ;
#27034 = VECTOR ( 'NONE', #43195, 1000.000000000000000 ) ;
#27035 = DIRECTION ( 'NONE',  ( -0.000000000000000000, 1.000000000000000000, -0.000000000000000000 ) ) ;
#27036 = ORIENTED_EDGE ( 'NONE', *, *, #35633, .F. ) ;
#27037 = DIRECTION ( 'NONE',  ( 0.000000000000000000, 0.000000000000000000, 1.000000000000000000 ) ) ;
#27038 = ORIENTED_EDGE ( 'NONE', *, *, #3742, .T. ) ;
#27039 = DIRECTION ( 'NONE',  ( -0.000000000000000000, 1.000000000000000000, -0.000000000000000000 ) ) ;
#27040 = ORIENTED_EDGE ( 'NONE', *, *, #19825, .T. ) ;
#27042 = CARTESIAN_POINT ( 'NONE',  ( -339.1964088526558498, -103.0458197858324496, 55.34326076196052213 ) ) ;
#27041 = CARTESIAN_POINT ( 'NONE',  ( 67.42090074966655777, -189.7472609257535510, -46.82076062204440348 ) ) ;
#27043 = ORIENTED_EDGE ( 'NONE', *, *, #43033, .T. ) ;
#27044 = DIRECTION ( 'NONE',  ( 0.7378332790417239107, 0.000000000000000000, 0.6749830015182142207 ) ) ;
#27045 = VERTEX_POINT ( 'NONE', #51857 ) ;
#27046 = CARTESIAN_POINT ( 'NONE',  ( 71.44208735029287993, -177.1207230881787780, 35.26900067126700833 ) ) ;
#27047 = CARTESIAN_POINT ( 'NONE',  ( -105.8382074681672975, -189.7472609257535510, -109.9360785596604728 ) ) ;
#27048 = VERTEX_POINT ( 'NONE', #47653 ) ;
#27049 = PLANE ( 'NONE',  #33922 ) ;
#27050 = LINE ( 'NONE', #47050, #45021 ) ;
#27051 = FACE_OUTER_BOUND ( 'NONE', #22788, .T. ) ;
#27052 = VECTOR ( 'NONE', #18601, 999.9999999999998863 ) ;
#27053 = CARTESIAN_POINT ( 'NONE',  ( -336.3521761649654422, -119.0014323656137947, -58.88711093124865670 ) ) ;
#27054 = ORIENTED_EDGE ( 'NONE', *, *, #4126, .T. ) ;
#27055 = DIRECTION ( 'NONE',  ( 0.000000000000000000, 0.000000000000000000, 1.000000000000000000 ) ) ;
#27056 = DIRECTION ( 'NONE',  ( -0.000000000000000000, 1.000000000000000000, -0.000000000000000000 ) ) ;
#27057 = DIRECTION ( 'NONE',  ( 1.000000000000000000, 0.000000000000000000, 0.000000000000000000 ) ) ;
#27058 = AXIS2_PLACEMENT_3D ( 'NONE', #19707, #35740, #36012 ) ;
#27059 = DIRECTION ( 'NONE',  ( 0.000000000000000000, 1.000000000000000000, 0.000000000000000000 ) ) ;
#27060 = ORIENTED_EDGE ( 'NONE', *, *, #18619, .T. ) ;
#27061 = DIRECTION ( 'NONE',  ( 0.000000000000000000, -1.000000000000000000, 0.000000000000000000 ) ) ;
#27062 = DIRECTION ( 'NONE',  ( 0.000000000000000000, 1.000000000000000000, 0.000000000000000000 ) ) ;
#27063 = CARTESIAN_POINT ( 'NONE',  ( -164.0008810331606810, -189.7472609257535510, 47.74645837849822527 ) ) ;
#27064 = LINE ( 'NONE', #3417, #36145 ) ;
#27065 = CARTESIAN_POINT ( 'NONE',  ( -280.0000000000000000, -153.5000000000000284, 60.00000000000002132 ) ) ;
#27066 = ADVANCED_FACE ( 'NONE', ( #3245 ), #16102, .F. ) ;
#27067 = ORIENTED_EDGE ( 'NONE', *, *, #31193, .F. ) ;
#27068 = VECTOR ( 'NONE', #31474, 999.9999999999998863 ) ;
#27069 = VECTOR ( 'NONE', #22490, 1000.000000000000000 ) ;
#27070 = AXIS2_PLACEMENT_3D ( 'NONE', #23069, #43556, #39078 ) ;
#27071 = FACE_OUTER_BOUND ( 'NONE', #23312, .T. ) ;
#27072 = CIRCLE ( 'NONE', #9462, 15.24495751795539000 ) ;
#27073 = PLANE ( 'NONE',  #13971 ) ;
#27074 = FACE_OUTER_BOUND ( 'NONE', #20523, .T. ) ;
#27075 = LINE ( 'NONE', #30002, #14514 ) ;
#27076 = FACE_OUTER_BOUND ( 'NONE', #6981, .T. ) ;
#27077 = EDGE_LOOP ( 'NONE', ( #32824, #12636, #48716, #3551 ) ) ;
#27078 = CIRCLE ( 'NONE', #4436, 4.000000000000003553 ) ;
#27079 = CARTESIAN_POINT ( 'NONE',  ( 3.366759895602029928, 51.76293813683449230, -20.33144901513888314 ) ) ;
#27080 = PLANE ( 'NONE',  #21293 ) ;
#27081 = ORIENTED_EDGE ( 'NONE', *, *, #41028, .F. ) ;
#27082 = ORIENTED_EDGE ( 'NONE', *, *, #34887, .F. ) ;
#27083 = EDGE_LOOP ( 'NONE', ( #50722, #2872, #19419, #3051 ) ) ;
#27084 = EDGE_CURVE ( 'NONE', #23558, #21890, #39481, .T. ) ;
#27085 = CARTESIAN_POINT ( 'NONE',  ( -77.67449977936063021, -193.5000000000000000, -121.5427093402339267 ) ) ;
#27086 = AXIS2_PLACEMENT_3D ( 'NONE', #4912, #44580, #33274 ) ;
#27087 = CARTESIAN_POINT ( 'NONE',  ( -260.0000000000000000, -153.5000000000000284, 60.00000000000002132 ) ) ;
#27088 = ORIENTED_EDGE ( 'NONE', *, *, #25799, .F. ) ;
#27089 = VECTOR ( 'NONE', #24562, 1000.000000000000000 ) ;
#27090 = CARTESIAN_POINT ( 'NONE',  ( -305.0000000000000568, -84.94915232962709695, -45.97643030831888211 ) ) ;
#27091 = CARTESIAN_POINT ( 'NONE',  ( -48.02249751411514467, -189.7472609257535510, 0.8896570909947569827 ) ) ;
#27094 = ORIENTED_EDGE ( 'NONE', *, *, #48696, .T. ) ;
#27093 = LINE ( 'NONE', #43130, #45098 ) ;
#27092 = CARTESIAN_POINT ( 'NONE',  ( -48.47912675150885065, -175.3837268820161057, 6.938893903907228378E-15 ) ) ;
#27095 = FACE_OUTER_BOUND ( 'NONE', #46199, .T. ) ;
#27096 = EDGE_LOOP ( 'NONE', ( #606, #8729, #24541, #25322 ) ) ;
#27097 = LINE ( 'NONE', #43134, #46579 ) ;
#27098 = ORIENTED_EDGE ( 'NONE', *, *, #44869, .F. ) ;
#27099 = DIRECTION ( 'NONE',  ( 0.000000000000000000, 1.000000000000000000, 0.000000000000000000 ) ) ;
#27100 = PLANE ( 'NONE',  #27972 ) ;
#27102 = LINE ( 'NONE', #22205, #33219 ) ;
#27101 = DIRECTION ( 'NONE',  ( -0.000000000000000000, 1.000000000000000000, -0.000000000000000000 ) ) ;
#27103 = AXIS2_PLACEMENT_3D ( 'NONE', #16281, #9131, #48082 ) ;
#27104 = VECTOR ( 'NONE', #3310, 1000.000000000000000 ) ;
#27105 = ORIENTED_EDGE ( 'NONE', *, *, #8992, .T. ) ;
#27106 = CARTESIAN_POINT ( 'NONE',  ( -49.47868758801764955, -193.5000000000000000, 0.02963332782255607284 ) ) ;
#27107 = EDGE_LOOP ( 'NONE', ( #28786, #16185, #43994, #42667 ) ) ;
#27108 = AXIS2_PLACEMENT_3D ( 'NONE', #28592, #5487, #4968 ) ;
#27109 = DIRECTION ( 'NONE',  ( 0.000000000000000000, 0.000000000000000000, -1.000000000000000000 ) ) ;
#27110 = CARTESIAN_POINT ( 'NONE',  ( -49.47517659412406488, -183.6283474603465606, -0.08879589532293878651 ) ) ;
#27111 = ORIENTED_EDGE ( 'NONE', *, *, #4493, .F. ) ;
#27112 = CARTESIAN_POINT ( 'NONE',  ( 1.755575411425451593, -189.7472609257535510, 114.4616734920527108 ) ) ;
#27113 = FACE_OUTER_BOUND ( 'NONE', #37194, .T. ) ;
#27114 = EDGE_CURVE ( 'NONE', #12713, #14995, #51332, .T. ) ;
#27115 = ORIENTED_EDGE ( 'NONE', *, *, #45388, .F. ) ;
#27116 = CARTESIAN_POINT ( 'NONE',  ( -159.3947744408687868, -193.5000000000000000, -55.44293326708444880 ) ) ;
#27117 = AXIS2_PLACEMENT_3D ( 'NONE', #17786, #33027, #9906 ) ;
#27118 = DIRECTION ( 'NONE',  ( -1.000000000000000000, 0.000000000000000000, -0.000000000000000000 ) ) ;
#27119 = ADVANCED_FACE ( 'NONE', ( #31864 ), #4017, .T. ) ;
#27120 = VERTEX_POINT ( 'NONE', #60 ) ;
#27121 = CARTESIAN_POINT ( 'NONE',  ( -48.47912675150885065, -189.7472609257535510, 6.938893903907228378E-15 ) ) ;
#27122 = ORIENTED_EDGE ( 'NONE', *, *, #50685, .F. ) ;
#27123 = DIRECTION ( 'NONE',  ( -1.000000000000000000, 0.000000000000000000, -0.000000000000000000 ) ) ;
#27124 = DIRECTION ( 'NONE',  ( 0.9982437317643210184, 0.000000000000000000, 0.05924062789372143423 ) ) ;
#27125 = EDGE_LOOP ( 'NONE', ( #42491, #37292, #17236, #33580 ) ) ;
#27126 = AXIS2_PLACEMENT_3D ( 'NONE', #19567, #51628, #20087 ) ;
#27127 = PLANE ( 'NONE',  #34427 ) ;
#27128 = CARTESIAN_POINT ( 'NONE',  ( -305.0000000000000568, -172.5932850007659169, -34.49419324804647857 ) ) ;
#27129 = CARTESIAN_POINT ( 'NONE',  ( 66.42899531795131907, -193.5000000000000000, 49.20491319441622124 ) ) ;
#27130 = EDGE_CURVE ( 'NONE', #16977, #9440, #4266, .T. ) ;
#27131 = EDGE_CURVE ( 'NONE', #22206, #2579, #8210, .T. ) ;
#27132 = AXIS2_PLACEMENT_3D ( 'NONE', #9182, #41476, #45196 ) ;
#27133 = LINE ( 'NONE', #43168, #21241 ) ;
#27134 = ADVANCED_FACE ( 'NONE', ( #28161 ), #44210, .T. ) ;
#27135 = CARTESIAN_POINT ( 'NONE',  ( -102.5006284722403507, -183.6283474603465606, -112.7238987608084955 ) ) ;
#27136 = DIRECTION ( 'NONE',  ( 0.000000000000000000, -1.000000000000000000, 0.000000000000000000 ) ) ;
#27138 = EDGE_LOOP ( 'NONE', ( #47347, #28631, #44858, #11516 ) ) ;
#27137 = CARTESIAN_POINT ( 'NONE',  ( -336.3521761649654422, -101.0520950768976149, 54.58714071513087873 ) ) ;
#27139 = ORIENTED_EDGE ( 'NONE', *, *, #33069, .T. ) ;
#27140 = LINE ( 'NONE', #38713, #34151 ) ;
#27141 = CONICAL_SURFACE ( 'NONE', #43096, 10.00000000000000711, 0.03490658503988659789 ) ;
#27142 = DIRECTION ( 'NONE',  ( -0.1476465640024918202, 0.000000000000000000, 0.9890401873221624784 ) ) ;
#27143 = VERTEX_POINT ( 'NONE', #314 ) ;
#27144 = CIRCLE ( 'NONE', #16246, 125.0000000000000000 ) ;
#27145 = EDGE_LOOP ( 'NONE', ( #18256, #43072, #34462, #17570 ) ) ;
#27146 = LINE ( 'NONE', #43179, #44095 ) ;
#27147 = ORIENTED_EDGE ( 'NONE', *, *, #24585, .T. ) ;
#27148 = EDGE_CURVE ( 'NONE', #34929, #18995, #16357, .T. ) ;
#27149 = CARTESIAN_POINT ( 'NONE',  ( -339.1964088526558498, -144.8891964568517778, 54.98865587491845730 ) ) ;
#27150 = FACE_BOUND ( 'NONE', #51512, .T. ) ;
#27151 = FACE_OUTER_BOUND ( 'NONE', #23983, .T. ) ;
#27152 = CARTESIAN_POINT ( 'NONE',  ( -49.44376233341721161, -175.3837268820161057, 0.2635871660690650709 ) ) ;
#27153 = ORIENTED_EDGE ( 'NONE', *, *, #19960, .F. ) ;
#27154 = EDGE_LOOP ( 'NONE', ( #5352, #35467, #14, #3095 ) ) ;
#27155 = ORIENTED_EDGE ( 'NONE', *, *, #35903, .T. ) ;
#27156 = DIRECTION ( 'NONE',  ( -0.000000000000000000, -3.491481338843133355E-15, -1.000000000000000000 ) ) ;
#27157 = DIRECTION ( 'NONE',  ( -0.000000000000000000, 1.000000000000000000, -0.000000000000000000 ) ) ;
#27158 = LINE ( 'NONE', #51881, #40864 ) ;
#27159 = CARTESIAN_POINT ( 'NONE',  ( 69.04371411670898340, -175.3837268820161057, -39.55227055146230697 ) ) ;
#27160 = FACE_OUTER_BOUND ( 'NONE', #9058, .T. ) ;
#27161 = VECTOR ( 'NONE', #24115, 1000.000000000000000 ) ;
#27162 = EDGE_LOOP ( 'NONE', ( #46280, #17953, #1801, #29233 ) ) ;
#27163 = CARTESIAN_POINT ( 'NONE',  ( -48.47912675150885065, -189.7472609257535510, 6.938893903907228378E-15 ) ) ;
#27164 = DIRECTION ( 'NONE',  ( 0.3758275821142422202, 0.000000000000000000, -0.9266896074318318188 ) ) ;
#27165 = CIRCLE ( 'NONE', #33885, 125.0000000000000000 ) ;
#27166 = VERTEX_POINT ( 'NONE', #12400 ) ;
#27167 = ORIENTED_EDGE ( 'NONE', *, *, #45282, .F. ) ;
#27168 = DIRECTION ( 'NONE',  ( -0.000000000000000000, 0.000000000000000000, -1.000000000000000000 ) ) ;
#27169 = LINE ( 'NONE', #41978, #24769 ) ;
#27170 = LINE ( 'NONE', #10377, #2345 ) ;
#27171 = ORIENTED_EDGE ( 'NONE', *, *, #27175, .T. ) ;
#27172 = DIRECTION ( 'NONE',  ( -0.000000000000000000, 0.000000000000000000, 1.000000000000000000 ) ) ;
#27173 = DIRECTION ( 'NONE',  ( 0.000000000000000000, 0.000000000000000000, -1.000000000000000000 ) ) ;
#27174 = EDGE_CURVE ( 'NONE', #40951, #16523, #33436, .T. ) ;
#27175 = EDGE_CURVE ( 'NONE', #36591, #33846, #8720, .T. ) ;
#27176 = DIRECTION ( 'NONE',  ( -0.9995608365087942371, 0.000000000000000000, -0.02963332782256331357 ) ) ;
#27177 = VERTEX_POINT ( 'NONE', #5055 ) ;
#27178 = CARTESIAN_POINT ( 'NONE',  ( -330.4913330509368166, -162.9984922102926532, -43.83057281297441676 ) ) ;
#27179 = VECTOR ( 'NONE', #48308, 1000.000000000000114 ) ;
#27180 = ORIENTED_EDGE ( 'NONE', *, *, #20019, .F. ) ;
#27181 = DIRECTION ( 'NONE',  ( 0.000000000000000000, 0.000000000000000000, 1.000000000000000000 ) ) ;
#27182 = CARTESIAN_POINT ( 'NONE',  ( 61.69163308845453031, -193.5000000000000000, -56.90809649257490577 ) ) ;
#27183 = ORIENTED_EDGE ( 'NONE', *, *, #22807, .T. ) ;
#27184 = LINE ( 'NONE', #2262, #15640 ) ;
#27185 = CARTESIAN_POINT ( 'NONE',  ( -336.3521761649654422, -111.9361751271348879, -57.91551518289410438 ) ) ;
#27186 = PLANE ( 'NONE',  #13960 ) ;
#27187 = EDGE_CURVE ( 'NONE', #17378, #39607, #19450, .T. ) ;
#27188 = DIRECTION ( 'NONE',  ( 1.000000000000000000, -0.000000000000000000, -0.000000000000000000 ) ) ;
#27189 = EDGE_CURVE ( 'NONE', #8253, #18753, #9509, .T. ) ;
#27190 = CARTESIAN_POINT ( 'NONE',  ( 72.14504940832446778, -175.3837268820161057, -32.78426643622660208 ) ) ;
#27191 = ORIENTED_EDGE ( 'NONE', *, *, #46257, .T. ) ;
#27192 = EDGE_CURVE ( 'NONE', #7467, #39853, #40771, .T. ) ;
#27193 = DIRECTION ( 'NONE',  ( -0.000000000000000000, 1.000000000000000000, -0.000000000000000000 ) ) ;
#27195 = ORIENTED_EDGE ( 'NONE', *, *, #15951, .T. ) ;
#27194 = CYLINDRICAL_SURFACE ( 'NONE', #23741, 125.0000000000000000 ) ;
#27196 = VECTOR ( 'NONE', #20849, 1000.000000000000000 ) ;
#27197 = ADVANCED_FACE ( 'NONE', ( #16631 ), #32639, .T. ) ;
#27198 = AXIS2_PLACEMENT_3D ( 'NONE', #1271, #17326, #24940 ) ;
#27199 = ORIENTED_EDGE ( 'NONE', *, *, #35864, .F. ) ;
#27200 = CARTESIAN_POINT ( 'NONE',  ( -132.4142998968130769, -177.1207230881787780, -91.27439114664585418 ) ) ;
#27201 = VERTEX_POINT ( 'NONE', #37629 ) ;
#27202 = VECTOR ( 'NONE', #646, 1000.000000000000000 ) ;
#27203 = DIRECTION ( 'NONE',  ( 0.000000000000000000, -1.000000000000000000, 0.000000000000000000 ) ) ;
#27204 = VERTEX_POINT ( 'NONE', #5319 ) ;
#27205 = CARTESIAN_POINT ( 'NONE',  ( 46.31065297101394407, -177.1207230881787780, 79.94433946042836681 ) ) ;
#27206 = DIRECTION ( 'NONE',  ( 0.000000000000000000, 0.000000000000000000, -1.000000000000000000 ) ) ;
#27207 = VERTEX_POINT ( 'NONE', #48939 ) ;
#27208 = CARTESIAN_POINT ( 'NONE',  ( -7.223120065443615623, -183.6283474603465606, 117.9955164924470523 ) ) ;
#27210 = VECTOR ( 'NONE', #18827, 1000.000000000000000 ) ;
#27209 = DIRECTION ( 'NONE',  ( 0.1182731709213592358, 0.000000000000000000, 0.9929810960135178055 ) ) ;
#27211 = CARTESIAN_POINT ( 'NONE',  ( -172.9089226952081617, -189.7472609257535510, 11.92584929509620117 ) ) ;
#27212 = ORIENTED_EDGE ( 'NONE', *, *, #37874, .F. ) ;
#27213 = VERTEX_POINT ( 'NONE', #37357 ) ;
#27214 = ORIENTED_EDGE ( 'NONE', *, *, #25097, .T. ) ;
#27215 = DIRECTION ( 'NONE',  ( -0.000000000000000000, 1.000000000000000000, -0.000000000000000000 ) ) ;
#27216 = ADVANCED_FACE ( 'NONE', ( #12919 ), #45004, .F. ) ;
#27217 = FACE_OUTER_BOUND ( 'NONE', #536, .T. ) ;
#27218 = DIRECTION ( 'NONE',  ( -0.000000000000000000, 1.000000000000000000, -0.000000000000000000 ) ) ;
#27219 = PLANE ( 'NONE',  #48899 ) ;
#27220 = DIRECTION ( 'NONE',  ( -0.000000000000000000, -0.9709418174260534551, -0.2393156642875516327 ) ) ;
#27221 = ORIENTED_EDGE ( 'NONE', *, *, #49729, .F. ) ;
#27222 = LINE ( 'NONE', #43534, #31629 ) ;
#27223 = EDGE_CURVE ( 'NONE', #32514, #51763, #27845, .T. ) ;
#27224 = VERTEX_POINT ( 'NONE', #41040 ) ;
#27226 = ORIENTED_EDGE ( 'NONE', *, *, #27553, .T. ) ;
#27225 = DIRECTION ( 'NONE',  ( -0.000000000000000000, 1.000000000000000000, -0.000000000000000000 ) ) ;
#27227 = DIRECTION ( 'NONE',  ( -1.000000000000000000, -0.000000000000000000, 0.000000000000000000 ) ) ;
#27228 = VERTEX_POINT ( 'NONE', #33680 ) ;
#27229 = DIRECTION ( 'NONE',  ( 0.000000000000000000, 0.000000000000000000, -1.000000000000000000 ) ) ;
#27230 = DIRECTION ( 'NONE',  ( -0.000000000000000000, -0.6631226582407989678, -0.7485107481710977506 ) ) ;
#27231 = VECTOR ( 'NONE', #23113, 1000.000000000000000 ) ;
#27232 = VECTOR ( 'NONE', #1274, 1000.000000000000000 ) ;
#27233 = EDGE_CURVE ( 'NONE', #3300, #8154, #30363, .T. ) ;
#27234 = EDGE_CURVE ( 'NONE', #36520, #42349, #13197, .T. ) ;
#27235 = DIRECTION ( 'NONE',  ( -1.000000000000000000, -0.000000000000000000, -0.000000000000000000 ) ) ;
#27236 = EDGE_CURVE ( 'NONE', #26646, #23894, #8459, .T. ) ;
#27237 = EDGE_CURVE ( 'NONE', #38924, #8616, #45274, .T. ) ;
#27238 = DIRECTION ( 'NONE',  ( 0.9785564922995032555, 0.000000000000000000, 0.2059786187411021818 ) ) ;
#27239 = ORIENTED_EDGE ( 'NONE', *, *, #13435, .T. ) ;
#27240 = FACE_OUTER_BOUND ( 'NONE', #31613, .T. ) ;
#27241 = VERTEX_POINT ( 'NONE', #21608 ) ;
#27242 = AXIS2_PLACEMENT_3D ( 'NONE', #42004, #25025, #10208 ) ;
#27243 = EDGE_CURVE ( 'NONE', #14667, #11081, #42933, .T. ) ;
#27244 = ORIENTED_EDGE ( 'NONE', *, *, #45720, .F. ) ;
#27245 = FACE_OUTER_BOUND ( 'NONE', #42101, .T. ) ;
#27246 = DIRECTION ( 'NONE',  ( 0.000000000000000000, 0.000000000000000000, -1.000000000000000000 ) ) ;
#27247 = EDGE_CURVE ( 'NONE', #22244, #29772, #17417, .T. ) ;
#27248 = CIRCLE ( 'NONE', #40665, 125.0000000000000000 ) ;
#27249 = LINE ( 'NONE', #27762, #50889 ) ;
#27250 = FACE_OUTER_BOUND ( 'NONE', #32446, .T. ) ;
#27251 = PLANE ( 'NONE',  #8718 ) ;
#27252 = CARTESIAN_POINT ( 'NONE',  ( -330.0000000000000568, -123.5000000000000284, 31.65769145387501027 ) ) ;
#27253 = EDGE_CURVE ( 'NONE', #20455, #9382, #49478, .T. ) ;
#27254 = ORIENTED_EDGE ( 'NONE', *, *, #11751, .F. ) ;
#27255 = AXIS2_PLACEMENT_3D ( 'NONE', #42877, #15042, #27868 ) ;
#27256 = CARTESIAN_POINT ( 'NONE',  ( -9.070200226166589275, -177.1207230881787780, -117.5715283571803980 ) ) ;
#27257 = LINE ( 'NONE', #31205, #46679 ) ;
#27258 = ADVANCED_FACE ( 'NONE', ( #24756 ), #45519, .F. ) ;
#27259 = DIRECTION ( 'NONE',  ( 0.9995608365087944591, 0.000000000000000000, -0.02963332782255633305 ) ) ;
#27260 = ORIENTED_EDGE ( 'NONE', *, *, #10646, .F. ) ;
#27261 = ADVANCED_FACE ( 'NONE', ( #17670 ), #18174, .T. ) ;
#27262 = CARTESIAN_POINT ( 'NONE',  ( -336.3521761649654422, -182.3871109312487420, -4.498567634386014369 ) ) ;
#27263 = DIRECTION ( 'NONE',  ( 0.000000000000000000, 0.000000000000000000, 1.000000000000000000 ) ) ;
#27264 = ADVANCED_FACE ( 'NONE', ( #34201 ), #26305, .T. ) ;
#27265 = ORIENTED_EDGE ( 'NONE', *, *, #28367, .F. ) ;
#27266 = CARTESIAN_POINT ( 'NONE',  ( -170.0000000000000284, -123.5000000000000284, 41.63467731922665394 ) ) ;
#27267 = VERTEX_POINT ( 'NONE', #21862 ) ;
#27268 = ADVANCED_FACE ( 'NONE', ( #18944 ), #38647, .T. ) ;
#27269 = LINE ( 'NONE', #19147, #29305 ) ;
#27270 = VECTOR ( 'NONE', #43551, 1000.000000000000000 ) ;
#27271 = FACE_BOUND ( 'NONE', #51084, .T. ) ;
#27272 = DIRECTION ( 'NONE',  ( -1.000000000000000000, -0.000000000000000000, -0.000000000000000000 ) ) ;
#27273 = VECTOR ( 'NONE', #32016, 1000.000000000000000 ) ;
#27274 = VECTOR ( 'NONE', #42246, 999.9999999999998863 ) ;
#27275 = DIRECTION ( 'NONE',  ( 0.000000000000000000, 0.000000000000000000, -1.000000000000000000 ) ) ;
#27276 = EDGE_CURVE ( 'NONE', #9666, #31844, #10538, .T. ) ;
#27277 = ORIENTED_EDGE ( 'NONE', *, *, #11114, .F. ) ;
#27278 = AXIS2_PLACEMENT_3D ( 'NONE', #1490, #29854, #45647 ) ;
#27279 = EDGE_CURVE ( 'NONE', #50350, #22576, #14498, .T. ) ;
#27280 = ORIENTED_EDGE ( 'NONE', *, *, #44218, .T. ) ;
#27281 = DIRECTION ( 'NONE',  ( -0.000000000000000000, 1.000000000000000000, -0.000000000000000000 ) ) ;
#27282 = ORIENTED_EDGE ( 'NONE', *, *, #3815, .T. ) ;
#27283 = AXIS2_PLACEMENT_3D ( 'NONE', #46709, #31179, #42761 ) ;
#27284 = CARTESIAN_POINT ( 'NONE',  ( -48.47912675150885065, -177.1207230881787780, 6.938893903907228378E-15 ) ) ;
#27285 = VECTOR ( 'NONE', #19343, 1000.000000000000000 ) ;
#27286 = CIRCLE ( 'NONE', #35691, 125.0000000000000000 ) ;
#27287 = AXIS2_PLACEMENT_3D ( 'NONE', #19932, #22841, #30712 ) ;
#27288 = CARTESIAN_POINT ( 'NONE',  ( -305.0000000000000568, -123.5000000000000284, -20.00000000000000355 ) ) ;
#27289 = DIRECTION ( 'NONE',  ( -1.000000000000000000, 0.000000000000000000, 0.000000000000000000 ) ) ;
#27290 = ORIENTED_EDGE ( 'NONE', *, *, #24409, .T. ) ;
#27293 = VERTEX_POINT ( 'NONE', #9770 ) ;
#27292 = CARTESIAN_POINT ( 'NONE',  ( 41.41233698655024398, -183.6283474603465606, 86.85922373029363541 ) ) ;
#27291 = CARTESIAN_POINT ( 'NONE',  ( -305.0000000000000568, -85.72124494520284088, -46.61293454085073051 ) ) ;
#27294 = FACE_OUTER_BOUND ( 'NONE', #12172, .T. ) ;
#27295 = EDGE_LOOP ( 'NONE', ( #32269, #36131, #42360, #15471 ) ) ;
#27296 = DIRECTION ( 'NONE',  ( -0.9890401873221623674, 0.000000000000000000, -0.1476465640024917925 ) ) ;
#27297 = VERTEX_POINT ( 'NONE', #6612 ) ;
#27298 = EDGE_CURVE ( 'NONE', #34044, #31341, #10038, .T. ) ;
#27299 = EDGE_CURVE ( 'NONE', #26956, #2085, #34704, .T. ) ;
#27300 = DIRECTION ( 'NONE',  ( 0.000000000000000000, -0.9927088740980530845, 0.1205366802553303057 ) ) ;
#27301 = ORIENTED_EDGE ( 'NONE', *, *, #27192, .F. ) ;
#27303 = CARTESIAN_POINT ( 'NONE',  ( -336.3521761649654422, -114.7679482383557144, 58.37307289257701370 ) ) ;
#27302 = CARTESIAN_POINT ( 'NONE',  ( 76.31829002442924548, -193.5000000000000000, 7.113702696402420145 ) ) ;
#27304 = VERTEX_POINT ( 'NONE', #6096 ) ;
#27305 = EDGE_CURVE ( 'NONE', #8359, #8140, #26988, .T. ) ;
#27306 = ADVANCED_FACE ( 'NONE', ( #37880 ), #10284, .F. ) ;
#27307 = CARTESIAN_POINT ( 'NONE',  ( -330.4913330509368166, -168.0775241366795569, 40.16023333901030412 ) ) ;
#27308 = ORIENTED_EDGE ( 'NONE', *, *, #42716, .F. ) ;
#27309 = CARTESIAN_POINT ( 'NONE',  ( 25.00456841203572367, 20.00000000000000355, 3.062176466986057355E-15 ) ) ;
#27310 = AXIS2_PLACEMENT_3D ( 'NONE', #1346, #1620, #37344 ) ;
#27311 = CARTESIAN_POINT ( 'NONE',  ( 0.000000000000000000, -178.6659583184393796, 20.92168833551003004 ) ) ;
#27312 = ORIENTED_EDGE ( 'NONE', *, *, #4125, .T. ) ;
#27313 = CARTESIAN_POINT ( 'NONE',  ( -305.0000000000000568, -181.3443148879387081, 15.93848283698911317 ) ) ;
#27314 = CARTESIAN_POINT ( 'NONE',  ( -26.20043062753592977, -193.5000000000000000, -122.9986166548863196 ) ) ;
#27315 = DIRECTION ( 'NONE',  ( 0.000000000000000000, 0.3546048870425363986, 0.9350162426854146114 ) ) ;
#27316 = AXIS2_PLACEMENT_3D ( 'NONE', #21369, #9545, #33193 ) ;
#27317 = CARTESIAN_POINT ( 'NONE',  ( -170.0000000000000284, -113.5000000000000142, 39.99999999999998579 ) ) ;
#27318 = VECTOR ( 'NONE', #17409, 1000.000000000000000 ) ;
#27319 = ORIENTED_EDGE ( 'NONE', *, *, #37247, .F. ) ;
#27320 = FACE_OUTER_BOUND ( 'NONE', #45492, .T. ) ;
#27321 = CARTESIAN_POINT ( 'NONE',  ( -336.3521761649654422, -182.3303666475049170, -11.78931550685388707 ) ) ;
#27322 = DIRECTION ( 'NONE',  ( 0.000000000000000000, -1.000000000000000000, 0.000000000000000000 ) ) ;
#27323 = ORIENTED_EDGE ( 'NONE', *, *, #48895, .F. ) ;
#27324 = CARTESIAN_POINT ( 'NONE',  ( -173.4291566779743050, -175.3837268820161057, 3.534122433558352760 ) ) ;
#27325 = DIRECTION ( 'NONE',  ( 0.000000000000000000, 1.000000000000000000, 0.000000000000000000 ) ) ;
#27326 = VECTOR ( 'NONE', #20517, 1000.000000000000000 ) ;
#27327 = CIRCLE ( 'NONE', #4677, 125.0000000000000000 ) ;
#27328 = CARTESIAN_POINT ( 'NONE',  ( -45.06671089634843952, -177.1207230881787780, -124.9534129907280402 ) ) ;
#27330 = ORIENTED_EDGE ( 'NONE', *, *, #19922, .F. ) ;
#27329 = CARTESIAN_POINT ( 'NONE',  ( -339.1964088526558498, -96.06030588028407635, 53.35787839313353942 ) ) ;
#27331 = EDGE_LOOP ( 'NONE', ( #46838, #11003, #11811, #34046 ) ) ;
#27332 = VECTOR ( 'NONE', #24653, 1000.000000000000114 ) ;
#27333 = VERTEX_POINT ( 'NONE', #42333 ) ;
#27334 = EDGE_CURVE ( 'NONE', #32642, #28039, #25798, .T. ) ;
#27335 = VECTOR ( 'NONE', #27945, 1000.000000000000000 ) ;
#27336 = CARTESIAN_POINT ( 'NONE',  ( -332.3517673607765914, -179.2447759217480154, -19.39547174791710660 ) ) ;
#27337 = FACE_OUTER_BOUND ( 'NONE', #6650, .T. ) ;
#27338 = DIRECTION ( 'NONE',  ( 0.000000000000000000, 0.000000000000000000, -1.000000000000000000 ) ) ;
#27339 = PLANE ( 'NONE',  #49737 ) ;
#27340 = CARTESIAN_POINT ( 'NONE',  ( 55.03325008324586065, -177.1207230881787780, -70.07273251429356264 ) ) ;
#27341 = VERTEX_POINT ( 'NONE', #38126 ) ;
#27342 = DIRECTION ( 'NONE',  ( 0.000000000000000000, 0.000000000000000000, -1.000000000000000000 ) ) ;
#27343 = ORIENTED_EDGE ( 'NONE', *, *, #40946, .T. ) ;
#27344 = ORIENTED_EDGE ( 'NONE', *, *, #6085, .T. ) ;
#27345 = AXIS2_PLACEMENT_3D ( 'NONE', #42785, #41998, #30187 ) ;
#27346 = EDGE_LOOP ( 'NONE', ( #22719, #16635, #6352, #34003 ) ) ;
#27347 = LINE ( 'NONE', #31548, #28395 ) ;
#27348 = VECTOR ( 'NONE', #23625, 1000.000000000000000 ) ;
#27349 = AXIS2_PLACEMENT_3D ( 'NONE', #20526, #36296, #27885 ) ;
#27350 = CARTESIAN_POINT ( 'NONE',  ( -339.1964088526558498, -103.0458197858333165, -55.34326076196084188 ) ) ;
#27351 = ORIENTED_EDGE ( 'NONE', *, *, #37166, .T. ) ;
#27352 = DIRECTION ( 'NONE',  ( 0.000000000000000000, 0.000000000000000000, -1.000000000000000000 ) ) ;
#27353 = PLANE ( 'NONE',  #5931 ) ;
#27356 = ORIENTED_EDGE ( 'NONE', *, *, #19564, .F. ) ;
#27355 = DIRECTION ( 'NONE',  ( 0.000000000000000000, 1.000000000000000000, 0.000000000000000000 ) ) ;
#27354 = FACE_OUTER_BOUND ( 'NONE', #10443, .T. ) ;
#27357 = VECTOR ( 'NONE', #48390, 1000.000000000000000 ) ;
#27358 = AXIS2_PLACEMENT_3D ( 'NONE', #10915, #42963, #6972 ) ;
#27359 = CARTESIAN_POINT ( 'NONE',  ( -336.3521761649654422, -142.2945752170892035, 56.98038208374156710 ) ) ;
#27360 = EDGE_LOOP ( 'NONE', ( #9455, #26162, #51730, #26342 ) ) ;
#27361 = DIRECTION ( 'NONE',  ( 0.000000000000000000, 0.000000000000000000, 1.000000000000000000 ) ) ;
#27362 = ORIENTED_EDGE ( 'NONE', *, *, #28843, .T. ) ;
#27363 = EDGE_CURVE ( 'NONE', #7018, #232, #42851, .T. ) ;
#27364 = LINE ( 'NONE', #10831, #582 ) ;
#27365 = DIRECTION ( 'NONE',  ( 0.000000000000000000, -0.9927088740980526405, 0.1205366802553337890 ) ) ;
#27367 = CARTESIAN_POINT ( 'NONE',  ( -169.0136227435421006, -193.5000000000000000, -33.11246405730811659 ) ) ;
#27366 = DIRECTION ( 'NONE',  ( -0.000000000000000000, -1.000000000000000000, 0.000000000000000000 ) ) ;
#27368 = VERTEX_POINT ( 'NONE', #2911 ) ;
#27369 = AXIS2_PLACEMENT_3D ( 'NONE', #30869, #27164, #34790 ) ;
#27370 = DIRECTION ( 'NONE',  ( 0.000000000000000000, 0.000000000000000000, -1.000000000000000000 ) ) ;
#27371 = VERTEX_POINT ( 'NONE', #22370 ) ;
#27372 = DIRECTION ( 'NONE',  ( 0.000000000000000000, 0.000000000000000000, 1.000000000000000000 ) ) ;
#27373 = EDGE_LOOP ( 'NONE', ( #1097, #26194, #32396, #217 ) ) ;
#27374 = CARTESIAN_POINT ( 'NONE',  ( -280.0000000000000000, -63.50000000000000000, 60.00000000000000711 ) ) ;
#27375 = DIRECTION ( 'NONE',  ( 0.000000000000000000, 0.000000000000000000, -1.000000000000000000 ) ) ;
#27376 = ORIENTED_EDGE ( 'NONE', *, *, #33318, .F. ) ;
#27377 = CARTESIAN_POINT ( 'NONE',  ( 75.02564229359539638, -193.5000000000000000, -19.27620354518634826 ) ) ;
#27378 = LINE ( 'NONE', #14801, #26445 ) ;
#27379 = VERTEX_POINT ( 'NONE', #30503 ) ;
#27380 = CARTESIAN_POINT ( 'NONE',  ( -46.00000000000000711, 20.00000000000000000, 8.673617379884035472E-15 ) ) ;
#27381 = ORIENTED_EDGE ( 'NONE', *, *, #50907, .T. ) ;
#27382 = VECTOR ( 'NONE', #7559, 999.9999999999998863 ) ;
#27383 = VECTOR ( 'NONE', #35223, 999.9999999999998863 ) ;
#27384 = CARTESIAN_POINT ( 'NONE',  ( -114.1105527140175440, -177.1207230881787780, 106.3838142112217326 ) ) ;
#27385 = CARTESIAN_POINT ( 'NONE',  ( -173.3294908491238004, -183.6283474603465606, -6.114457023560960991 ) ) ;
#27386 = EDGE_CURVE ( 'NONE', #5683, #36042, #34966, .T. ) ;
#27387 = VECTOR ( 'NONE', #44715, 1000.000000000000227 ) ;
#27388 = CARTESIAN_POINT ( 'NONE',  ( -336.3521761649654422, -181.4155151828941825, -11.56382487286496463 ) ) ;
#27389 = CARTESIAN_POINT ( 'NONE',  ( 7.859956736328458149, -189.7472609257535510, -111.5836353223468649 ) ) ;
#27390 = DIRECTION ( 'NONE',  ( 0.000000000000000000, 1.000000000000000000, 0.000000000000000000 ) ) ;
#27391 = DIRECTION ( 'NONE',  ( 0.000000000000000000, -0.000000000000000000, -1.000000000000000000 ) ) ;
#27392 = AXIS2_PLACEMENT_3D ( 'NONE', #16402, #40287, #352 ) ;
#27393 = VECTOR ( 'NONE', #17734, 1000.000000000000000 ) ;
#27394 = DIRECTION ( 'NONE',  ( 1.000000000000000000, -0.000000000000000000, -0.000000000000000000 ) ) ;
#27396 = ORIENTED_EDGE ( 'NONE', *, *, #9893, .T. ) ;
#27395 = CARTESIAN_POINT ( 'NONE',  ( -339.1964088526558498, -162.9984922102920848, 43.83057281297495678 ) ) ;
#27397 = CIRCLE ( 'NONE', #42525, 125.0000000000000000 ) ;
#27398 = CIRCLE ( 'NONE', #13161, 125.0000000000000000 ) ;
#27399 = ORIENTED_EDGE ( 'NONE', *, *, #25248, .T. ) ;
#27400 = LINE ( 'NONE', #39995, #50972 ) ;
#27401 = EDGE_CURVE ( 'NONE', #28959, #3470, #1880, .T. ) ;
#27402 = AXIS2_PLACEMENT_3D ( 'NONE', #25113, #25610, #45091 ) ;
#27403 = AXIS2_PLACEMENT_3D ( 'NONE', #12947, #89, #40279 ) ;
#27404 = PLANE ( 'NONE',  #4455 ) ;
#27405 = EDGE_LOOP ( 'NONE', ( #42302, #28182, #43920, #12285 ) ) ;
#27406 = ORIENTED_EDGE ( 'NONE', *, *, #19844, .T. ) ;
#27407 = EDGE_CURVE ( 'NONE', #32388, #19412, #18437, .T. ) ;
#27408 = CARTESIAN_POINT ( 'NONE',  ( -165.2002711502080672, -193.5000000000000000, 44.73448837594998651 ) ) ;
#27409 = VERTEX_POINT ( 'NONE', #50501 ) ;
#27410 = LINE ( 'NONE', #37048, #40981 ) ;
#27411 = DIRECTION ( 'NONE',  ( 0.000000000000000000, 0.000000000000000000, 1.000000000000000000 ) ) ;
#27412 = CARTESIAN_POINT ( 'NONE',  ( -330.4913330509368166, -108.8949048983213004, -57.16590939599337418 ) ) ;
#27413 = CARTESIAN_POINT ( 'NONE',  ( 141.7825277784304205, -213.5000000000000000, 10.00000000000000178 ) ) ;
#27414 = ORIENTED_EDGE ( 'NONE', *, *, #17541, .F. ) ;
#27415 = ORIENTED_EDGE ( 'NONE', *, *, #43568, .T. ) ;
#27416 = ORIENTED_EDGE ( 'NONE', *, *, #4950, .F. ) ;
#27417 = EDGE_CURVE ( 'NONE', #49057, #4116, #10226, .T. ) ;
#27418 = CARTESIAN_POINT ( 'NONE',  ( -49.21696003055057389, -193.5000000000000000, -0.6749830015182127774 ) ) ;
#27419 = DIRECTION ( 'NONE',  ( 0.000000000000000000, 0.000000000000000000, -1.000000000000000000 ) ) ;
#27420 = AXIS2_PLACEMENT_3D ( 'NONE', #4323, #48740, #24549 ) ;
#27421 = FACE_OUTER_BOUND ( 'NONE', #11843, .T. ) ;
#27422 = VECTOR ( 'NONE', #43686, 1000.000000000000000 ) ;
#27423 = CARTESIAN_POINT ( 'NONE',  ( -330.4913330509368166, -131.1080185721132807, -58.50955523165751515 ) ) ;
#27424 = CARTESIAN_POINT ( 'NONE',  ( -21.46839590530488096, -177.1207230881787780, 122.0467960216650880 ) ) ;
#27425 = VERTEX_POINT ( 'NONE', #3677 ) ;
#27426 = AXIS2_PLACEMENT_3D ( 'NONE', #7535, #3580, #35635 ) ;
#27427 = UNCERTAINTY_MEASURE_WITH_UNIT (LENGTH_MEASURE( 1.000000000000000082E-05 ), #5171, 'distance_accuracy_value', 'NONE');
#27428 = EDGE_CURVE ( 'NONE', #37383, #6661, #32006, .T. ) ;
#27429 = DIRECTION ( 'NONE',  ( 0.000000000000000000, 0.000000000000000000, 1.000000000000000000 ) ) ;
#27430 = DIRECTION ( 'NONE',  ( 0.000000000000000000, -0.000000000000000000, 1.000000000000000000 ) ) ;
#27431 = EDGE_CURVE ( 'NONE', #27425, #3020, #39667, .T. ) ;
#27432 = ORIENTED_EDGE ( 'NONE', *, *, #50685, .T. ) ;
#27433 = ORIENTED_EDGE ( 'NONE', *, *, #41321, .F. ) ;
#27434 = VECTOR ( 'NONE', #48771, 1000.000000000000000 ) ;
#27435 = EDGE_CURVE ( 'NONE', #16290, #6723, #8151, .T. ) ;
#27436 = ORIENTED_EDGE ( 'NONE', *, *, #9303, .T. ) ;
#27437 = CARTESIAN_POINT ( 'NONE',  ( 75.21854001195777073, -193.5000000000000000, -8.665274887905434653 ) ) ;
#27438 = LINE ( 'NONE', #50856, #46835 ) ;
#27439 = ORIENTED_EDGE ( 'NONE', *, *, #12561, .T. ) ;
#27440 = DIRECTION ( 'NONE',  ( 0.000000000000000000, -1.000000000000000000, 0.000000000000000000 ) ) ;
#27441 = AXIS2_PLACEMENT_3D ( 'NONE', #42881, #23678, #39199 ) ;
#27442 = AXIS2_PLACEMENT_3D ( 'NONE', #28932, #44720, #564 ) ;
#27443 = CARTESIAN_POINT ( 'NONE',  ( 37.77106160267054236, -175.3837268820161057, 89.08931047202636933 ) ) ;
#27444 = CARTESIAN_POINT ( 'NONE',  ( -330.4913330509368166, -108.6560878169904640, -58.13482838284724608 ) ) ;
#27445 = ORIENTED_EDGE ( 'NONE', *, *, #6916, .F. ) ;
#27446 = CARTESIAN_POINT ( 'NONE',  ( 29.90148147319962391, -177.1207230881787780, 96.08646119224012239 ) ) ;
#27447 = MECHANICAL_DESIGN_GEOMETRIC_PRESENTATION_REPRESENTATION (  '', ( #14037 ), #11502 ) ;
#27448 = VECTOR ( 'NONE', #4502, 1000.000000000000114 ) ;
#27449 = VERTEX_POINT ( 'NONE', #254 ) ;
#27450 = CARTESIAN_POINT ( 'NONE',  ( -33.98218805075477178, -193.5000000000000000, 123.1496609813405314 ) ) ;
#27451 = CARTESIAN_POINT ( 'NONE',  ( -48.47912675150885065, -183.6283474603465606, 6.938893903907228378E-15 ) ) ;
#27452 = EDGE_CURVE ( 'NONE', #26525, #47039, #38725, .T. ) ;
#27453 = ORIENTED_EDGE ( 'NONE', *, *, #22489, .T. ) ;
#27454 = DIRECTION ( 'NONE',  ( 0.4285077258200430950, -0.8746197071393964073, -0.2267630851702529260 ) ) ;
#27455 = CARTESIAN_POINT ( 'NONE',  ( -48.59739992243022755, -189.7472609257535510, 0.9929810960135230236 ) ) ;
#27456 = CARTESIAN_POINT ( 'NONE',  ( 57.12946453413545100, -175.3837268820161057, 66.87170886602000053 ) ) ;
#27457 = LINE ( 'NONE', #23779, #30766 ) ;
#27458 = EDGE_CURVE ( 'NONE', #43120, #32812, #51523, .T. ) ;
#27459 = CARTESIAN_POINT ( 'NONE',  ( -48.47912675150885065, -177.1207230881787780, 6.938893903907228378E-15 ) ) ;
#27460 = ORIENTED_EDGE ( 'NONE', *, *, #50424, .T. ) ;
#27461 = ORIENTED_EDGE ( 'NONE', *, *, #15630, .T. ) ;
#27462 = VECTOR ( 'NONE', #6243, 1000.000000000000000 ) ;
#27463 = VECTOR ( 'NONE', #29213, 1000.000000000000000 ) ;
#27464 = FACE_OUTER_BOUND ( 'NONE', #26742, .T. ) ;
#27466 = ORIENTED_EDGE ( 'NONE', *, *, #9296, .F. ) ;
#27465 = CARTESIAN_POINT ( 'NONE',  ( -330.4913330509368166, -79.66942718702547666, -39.49849221029252533 ) ) ;
#27467 = VECTOR ( 'NONE', #24699, 1000.000000000000000 ) ;
#27468 = ORIENTED_EDGE ( 'NONE', *, *, #40386, .F. ) ;
#27469 = DIRECTION ( 'NONE',  ( -0.7575112421616284619, 0.000000000000000000, 0.6528221181905119463 ) ) ;
#27470 = CARTESIAN_POINT ( 'NONE',  ( -336.3521761649653854, -66.84097189748108292, 19.74220186498881091 ) ) ;
#27471 = AXIS2_PLACEMENT_3D ( 'NONE', #43191, #34022, #332 ) ;
#27472 = ORIENTED_EDGE ( 'NONE', *, *, #50183, .T. ) ;
#27473 = CARTESIAN_POINT ( 'NONE',  ( -49.47868758801764955, -193.5000000000000000, 0.02963332782255607284 ) ) ;
#27474 = CIRCLE ( 'NONE', #4838, 125.0000000000000000 ) ;
#27475 = FACE_OUTER_BOUND ( 'NONE', #11799, .T. ) ;
#27476 = VERTEX_POINT ( 'NONE', #47328 ) ;
#27477 = DIRECTION ( 'NONE',  ( 0.000000000000000000, 0.000000000000000000, 1.000000000000000000 ) ) ;
#27478 = VECTOR ( 'NONE', #409, 1000.000000000000000 ) ;
#27479 = EDGE_CURVE ( 'NONE', #41341, #7980, #26192, .T. ) ;
#27480 = EDGE_CURVE ( 'NONE', #21906, #5412, #31536, .T. ) ;
#27481 = VECTOR ( 'NONE', #17895, 1000.000000000000000 ) ;
#27482 = FACE_OUTER_BOUND ( 'NONE', #43235, .T. ) ;
#27483 = LINE ( 'NONE', #48243, #50956 ) ;
#27484 = ORIENTED_EDGE ( 'NONE', *, *, #21809, .F. ) ;
#27485 = ORIENTED_EDGE ( 'NONE', *, *, #41022, .T. ) ;
#27486 = ORIENTED_EDGE ( 'NONE', *, *, #13077, .T. ) ;
#27487 = AXIS2_PLACEMENT_3D ( 'NONE', #7407, #31555, #44167 ) ;
#27488 = CARTESIAN_POINT ( 'NONE',  ( -107.6930423737362190, -177.1207230881787780, 110.0850225811110761 ) ) ;
#27489 = CARTESIAN_POINT ( 'NONE',  ( 3.686287386450715076E-15, 20.00000000000000000, -51.00000000000000711 ) ) ;
#27490 = CARTESIAN_POINT ( 'NONE',  ( -332.3517673607765914, -164.4944191672036311, -43.81161486573635244 ) ) ;
#27491 = DIRECTION ( 'NONE',  ( 0.000000000000000000, 0.000000000000000000, 1.000000000000000000 ) ) ;
#27492 = DIRECTION ( 'NONE',  ( 0.000000000000000000, 0.000000000000000000, -1.000000000000000000 ) ) ;
#27493 = ORIENTED_EDGE ( 'NONE', *, *, #49783, .F. ) ;
#27494 = EDGE_CURVE ( 'NONE', #13896, #47167, #21185, .T. ) ;
#27495 = ADVANCED_FACE ( 'NONE', ( #16042 ), #3179, .F. ) ;
#27496 = CARTESIAN_POINT ( 'NONE',  ( -8.169009709621407822, -177.1207230881787780, 118.3219948448695504 ) ) ;
#27497 = ORIENTED_EDGE ( 'NONE', *, *, #45971, .F. ) ;
#27499 = ORIENTED_EDGE ( 'NONE', *, *, #2462, .T. ) ;
#27498 = CARTESIAN_POINT ( 'NONE',  ( -332.3517673607765914, -170.5607375887735770, 35.68215131113770155 ) ) ;
#27500 = VECTOR ( 'NONE', #33474, 1000.000000000000000 ) ;
#27501 = VERTEX_POINT ( 'NONE', #11577 ) ;
#27502 = VECTOR ( 'NONE', #16264, 1000.000000000000000 ) ;
#27503 = EDGE_CURVE ( 'NONE', #4690, #19065, #47593, .T. ) ;
#27504 = LINE ( 'NONE', #30932, #50147 ) ;
#27505 = FACE_OUTER_BOUND ( 'NONE', #11983, .T. ) ;
#27506 = AXIS2_PLACEMENT_3D ( 'NONE', #8731, #20836, #29234 ) ;
#27507 = EDGE_CURVE ( 'NONE', #19466, #19179, #51274, .T. ) ;
#27508 = CARTESIAN_POINT ( 'NONE',  ( -154.2693405752510500, -193.5000000000000000, 66.58401203837830451 ) ) ;
#27509 = CARTESIAN_POINT ( 'NONE',  ( -91.22542124915045747, -189.7472609257535510, 117.4638425504669783 ) ) ;
#27510 = ORIENTED_EDGE ( 'NONE', *, *, #17172, .F. ) ;
#27511 = CARTESIAN_POINT ( 'NONE',  ( 75.52097166332625022, -193.5000000000000000, -0.3215015308241103709 ) ) ;
#27512 = VERTEX_POINT ( 'NONE', #4214 ) ;
#27513 = VERTEX_POINT ( 'NONE', #15263 ) ;
#27514 = PLANE ( 'NONE',  #37147 ) ;
#27515 = AXIS2_PLACEMENT_3D ( 'NONE', #29020, #1439, #41375 ) ;
#27516 = CARTESIAN_POINT ( 'NONE',  ( 25.43954814678887644, -177.1207230881787780, 100.8019320314832754 ) ) ;
#27517 = CARTESIAN_POINT ( 'NONE',  ( -48.41988612361515010, -177.1207230881787780, 0.9982437317643287900 ) ) ;
#27518 = CARTESIAN_POINT ( 'NONE',  ( 72.95485052494852596, -183.6283474603465606, -29.64437826672758192 ) ) ;
#27519 = DIRECTION ( 'NONE',  ( -0.9151456172430237901, 0.000000000000000000, 0.4031234292879600778 ) ) ;
#27520 = DIRECTION ( 'NONE',  ( -0.3482016354343866471, 0.000000000000000000, -0.9374196611341253371 ) ) ;
#27521 = ORIENTED_EDGE ( 'NONE', *, *, #16992, .F. ) ;
#27522 = LINE ( 'NONE', #40365, #27161 ) ;
#27523 = PLANE ( 'NONE',  #18996 ) ;
#27524 = AXIS2_PLACEMENT_3D ( 'NONE', #33124, #25502, #28913 ) ;
#27525 = LINE ( 'NONE', #14949, #37460 ) ;
#27526 = VERTEX_POINT ( 'NONE', #23155 ) ;
#27527 = LINE ( 'NONE', #40130, #16378 ) ;
#27528 = CARTESIAN_POINT ( 'NONE',  ( -49.44376233341721161, -193.5000000000000000, 0.2635871660690650709 ) ) ;
#27529 = EDGE_LOOP ( 'NONE', ( #49631, #7240, #3510, #19353 ) ) ;
#27530 = PLANE ( 'NONE',  #18696 ) ;
#27531 = ORIENTED_EDGE ( 'NONE', *, *, #48642, .F. ) ;
#27532 = VECTOR ( 'NONE', #21370, 1000.000000000000000 ) ;
#27533 = DIRECTION ( 'NONE',  ( 0.000000000000000000, 0.000000000000000000, 1.000000000000000000 ) ) ;
#27534 = AXIS2_PLACEMENT_3D ( 'NONE', #22796, #38809, #51442 ) ;
#27535 = AXIS2_PLACEMENT_3D ( 'NONE', #23431, #39436, #18198 ) ;
#27536 = FACE_BOUND ( 'NONE', #2886, .T. ) ;
#27537 = ADVANCED_FACE ( 'NONE', ( #43110 ), #19452, .T. ) ;
#27539 = ORIENTED_EDGE ( 'NONE', *, *, #32224, .T. ) ;
#27538 = LINE ( 'NONE', #7822, #28750 ) ;
#27540 = VECTOR ( 'NONE', #29170, 1000.000000000000000 ) ;
#27541 = EDGE_CURVE ( 'NONE', #31431, #40613, #12069, .T. ) ;
#27542 = ADVANCED_FACE ( 'NONE', ( #27074 ), #36011, .F. ) ;
#27543 = EDGE_CURVE ( 'NONE', #2344, #28891, #32306, .T. ) ;
#27544 = DIRECTION ( 'NONE',  ( 0.000000000000000000, 0.000000000000000000, 1.000000000000000000 ) ) ;
#27545 = EDGE_LOOP ( 'NONE', ( #39238, #376, #8516, #49614 ) ) ;
#27546 = ADVANCED_FACE ( 'NONE', ( #49142 ), #20485, .T. ) ;
#27547 = VERTEX_POINT ( 'NONE', #40983 ) ;
#27548 = PLANE ( 'NONE',  #38471 ) ;
#27549 = VECTOR ( 'NONE', #7330, 1000.000000000000114 ) ;
#27550 = ORIENTED_EDGE ( 'NONE', *, *, #28475, .F. ) ;
#27551 = EDGE_CURVE ( 'NONE', #41331, #23075, #1030, .T. ) ;
#27552 = CARTESIAN_POINT ( 'NONE',  ( -48.53836737940257251, -183.6283474603465606, 0.9982437317643279018 ) ) ;
#27553 = EDGE_CURVE ( 'NONE', #12201, #6494, #29408, .T. ) ;
#27554 = EDGE_CURVE ( 'NONE', #14631, #18737, #1032, .T. ) ;
#27555 = VECTOR ( 'NONE', #27810, 1000.000000000000114 ) ;
#27556 = CARTESIAN_POINT ( 'NONE',  ( -336.3521761649654422, -72.01665693856799066, -28.86398714850468039 ) ) ;
#27557 = DIRECTION ( 'NONE',  ( 0.000000000000000000, 1.000000000000000000, -0.000000000000000000 ) ) ;
#27558 = ORIENTED_EDGE ( 'NONE', *, *, #22709, .T. ) ;
#27560 = EDGE_LOOP ( 'NONE', ( #9733, #31265 ) ) ;
#27559 = LINE ( 'NONE', #43590, #42648 ) ;
#27561 = EDGE_CURVE ( 'NONE', #1527, #51496, #17354, .T. ) ;
#27562 = CARTESIAN_POINT ( 'NONE',  ( -48.47912675150885065, -183.6283474603465606, 6.938893903907228378E-15 ) ) ;
#27563 = EDGE_LOOP ( 'NONE', ( #12214, #17796, #37464, #5957 ) ) ;
#27564 = CARTESIAN_POINT ( 'NONE',  ( 40.29886924377099433, 30.00000000000000355, -46.21030057994576623 ) ) ;
#27565 = ORIENTED_EDGE ( 'NONE', *, *, #41081, .F. ) ;
#27566 = EDGE_CURVE ( 'NONE', #653, #16210, #11079, .T. ) ;
#27567 = FACE_OUTER_BOUND ( 'NONE', #1409, .T. ) ;
#27568 = ORIENTED_EDGE ( 'NONE', *, *, #13135, .F. ) ;
#27570 = DIRECTION ( 'NONE',  ( 0.2920567706369764371, 0.000000000000000000, -0.9564009842765223146 ) ) ;
#27569 = PLANE ( 'NONE',  #30789 ) ;
#27571 = EDGE_LOOP ( 'NONE', ( #13430, #51841, #46472, #48025 ) ) ;
#27572 = EDGE_CURVE ( 'NONE', #2420, #37889, #32089, .T. ) ;
#27573 = LINE ( 'NONE', #35709, #12282 ) ;
#27574 = ORIENTED_EDGE ( 'NONE', *, *, #28184, .T. ) ;
#27575 = CARTESIAN_POINT ( 'NONE',  ( -173.2419626162308646, -193.5000000000000000, 7.696413904698416353 ) ) ;
#27576 = AXIS2_PLACEMENT_3D ( 'NONE', #18536, #11151, #42441 ) ;
#27577 = CARTESIAN_POINT ( 'NONE',  ( -49.38192458147459973, -183.6283474603465606, 0.4300652022765185656 ) ) ;
#27578 = AXIS2_PLACEMENT_3D ( 'NONE', #35176, #50973, #27027 ) ;
#27579 = LINE ( 'NONE', #43608, #18805 ) ;
#27580 = CARTESIAN_POINT ( 'NONE',  ( -339.1964088526558498, -157.4273119900845757, 48.27201571436049932 ) ) ;
#27581 = CARTESIAN_POINT ( 'NONE',  ( -172.4295958414655274, -189.7472609257535510, 3.504489105735757892 ) ) ;
#27582 = VECTOR ( 'NONE', #42545, 1000.000000000000000 ) ;
#27583 = LINE ( 'NONE', #43362, #29755 ) ;
#27584 = ORIENTED_EDGE ( 'NONE', *, *, #14614, .T. ) ;
#27585 = DIRECTION ( 'NONE',  ( -0.7031628666216435120, -1.263457945442559552E-17, 0.7110288200941177195 ) ) ;
#27586 = DIRECTION ( 'NONE',  ( -0.000000000000000000, 1.000000000000000000, -0.000000000000000000 ) ) ;
#27587 = ADVANCED_FACE ( 'NONE', ( #45215 ), #49413, .T. ) ;
#27588 = CARTESIAN_POINT ( 'NONE',  ( -332.3517673607765914, -123.5000000000000284, 0.000000000000000000 ) ) ;
#27589 = DIRECTION ( 'NONE',  ( -0.000000000000000000, -1.000000000000000000, 0.000000000000000000 ) ) ;
#27590 = ORIENTED_EDGE ( 'NONE', *, *, #1500, .T. ) ;
#27591 = AXIS2_PLACEMENT_3D ( 'NONE', #47466, #7264, #15420 ) ;
#27592 = CARTESIAN_POINT ( 'NONE',  ( 0.000000000000000000, -109.3803758070342838, -57.28556722813713975 ) ) ;
#27593 = LINE ( 'NONE', #18682, #40360 ) ;
#27594 = CARTESIAN_POINT ( 'NONE',  ( 32.49319223169170812, -193.5000000000000000, -95.22858582633060109 ) ) ;
#27596 = VERTEX_POINT ( 'NONE', #13130 ) ;
#27595 = CARTESIAN_POINT ( 'NONE',  ( 0.000000000000000000, -96.08133284941705199, 52.24190551353909484 ) ) ;
#27597 = ORIENTED_EDGE ( 'NONE', *, *, #17945, .F. ) ;
#27598 = ORIENTED_EDGE ( 'NONE', *, *, #37635, .F. ) ;
#27599 = AXIS2_PLACEMENT_3D ( 'NONE', #16468, #24861, #24098 ) ;
#27600 = EDGE_CURVE ( 'NONE', #13819, #3616, #9450, .T. ) ;
#27601 = FACE_BOUND ( 'NONE', #19141, .T. ) ;
#27602 = DIRECTION ( 'NONE',  ( 0.000000000000000000, -1.000000000000000000, -0.000000000000000000 ) ) ;
#27603 = DIRECTION ( 'NONE',  ( -0.000000000000000000, 1.000000000000000000, -0.000000000000000000 ) ) ;
#27604 = DIRECTION ( 'NONE',  ( 0.000000000000000000, 0.000000000000000000, 1.000000000000000000 ) ) ;
#27605 = ORIENTED_EDGE ( 'NONE', *, *, #17231, .F. ) ;
#27606 = EDGE_CURVE ( 'NONE', #33402, #3342, #6891, .T. ) ;
#27607 = EDGE_CURVE ( 'NONE', #19447, #45420, #29153, .T. ) ;
#27608 = EDGE_CURVE ( 'NONE', #48860, #17312, #40707, .T. ) ;
#27609 = CARTESIAN_POINT ( 'NONE',  ( 46.00000000000000711, -57.64213562373095101, -41.00000000000000000 ) ) ;
#27610 = EDGE_CURVE ( 'NONE', #47197, #51691, #5259, .T. ) ;
#27611 = ORIENTED_EDGE ( 'NONE', *, *, #42612, .F. ) ;
#27612 = EDGE_LOOP ( 'NONE', ( #36399, #45250, #36378, #9647 ) ) ;
#27613 = VECTOR ( 'NONE', #22580, 1000.000000000000000 ) ;
#27614 = ORIENTED_EDGE ( 'NONE', *, *, #8758, .F. ) ;
#27615 = LINE ( 'NONE', #39938, #35952 ) ;
#27616 = AXIS2_PLACEMENT_3D ( 'NONE', #10947, #26968, #8807 ) ;
#27617 = CARTESIAN_POINT ( 'NONE',  ( -336.3521761649654422, -181.4155151828941825, -11.56382487286496463 ) ) ;
#27618 = VERTEX_POINT ( 'NONE', #16831 ) ;
#27619 = CARTESIAN_POINT ( 'NONE',  ( -339.1964088526558498, -182.1300919119129560, -6.615309698014600670 ) ) ;
#27620 = CARTESIAN_POINT ( 'NONE',  ( -336.3521761649654422, -106.8245764869328980, 56.65561927337994064 ) ) ;
#27621 = VECTOR ( 'NONE', #8768, 1000.000000000000000 ) ;
#27624 = VERTEX_POINT ( 'NONE', #32834 ) ;
#27623 = DIRECTION ( 'NONE',  ( 1.000000000000000000, 7.175085443855077145E-17, -4.952603889764050661E-17 ) ) ;
#27622 = CARTESIAN_POINT ( 'NONE',  ( 3.499092996509686644E-32, 65.00000000000000000, 0.000000000000000000 ) ) ;
#27625 = ADVANCED_FACE ( 'NONE', ( #48886 ), #8930, .T. ) ;
#27626 = FACE_OUTER_BOUND ( 'NONE', #16014, .T. ) ;
#27627 = ORIENTED_EDGE ( 'NONE', *, *, #39058, .F. ) ;
#27628 = LINE ( 'NONE', #43658, #50746 ) ;
#27629 = EDGE_LOOP ( 'NONE', ( #21131, #19681, #31502, #19903 ) ) ;
#27630 = ADVANCED_FACE ( 'NONE', ( #21017 ), #37035, .T. ) ;
#27631 = CIRCLE ( 'NONE', #4996, 125.0000000000000000 ) ;
#27632 = DIRECTION ( 'NONE',  ( -0.4300652022765183435, 0.000000000000000000, -0.9027978299657446470 ) ) ;
#27633 = CARTESIAN_POINT ( 'NONE',  ( 0.000000000000000000, -162.6242368362065918, 44.16213414209531862 ) ) ;
#27635 = DIRECTION ( 'NONE',  ( 1.043714542225393539E-14, 0.4647231720437573488, -0.8854560256532157947 ) ) ;
#27634 = DIRECTION ( 'NONE',  ( 0.000000000000000000, 0.000000000000000000, -1.000000000000000000 ) ) ;
#27636 = EDGE_LOOP ( 'NONE', ( #13069, #51735, #849, #2818 ) ) ;
#27637 = ADVANCED_FACE ( 'NONE', ( #21278 ), #37296, .F. ) ;
#27638 = VECTOR ( 'NONE', #26144, 1000.000000000000000 ) ;
#27639 = DIRECTION ( 'NONE',  ( -0.000000000000000000, -1.000000000000000000, -0.000000000000000000 ) ) ;
#27640 = DIRECTION ( 'NONE',  ( -1.000000000000000000, 0.000000000000000000, -0.000000000000000000 ) ) ;
#27641 =( NAMED_UNIT ( * ) SI_UNIT ( $, .STERADIAN. ) SOLID_ANGLE_UNIT ( ) );
#27642 = ORIENTED_EDGE ( 'NONE', *, *, #28276, .T. ) ;
#27643 = CARTESIAN_POINT ( 'NONE',  ( -48.47912675150885065, -183.6283474603465606, 6.938893903907228378E-15 ) ) ;
#27644 = DIRECTION ( 'NONE',  ( -1.000000000000000000, -0.000000000000000000, 0.000000000000000000 ) ) ;
#27645 = PLANE ( 'NONE',  #33289 ) ;
#27646 = VERTEX_POINT ( 'NONE', #26237 ) ;
#27647 = PLANE ( 'NONE',  #28423 ) ;
#27648 = FACE_OUTER_BOUND ( 'NONE', #12175, .T. ) ;
#27649 = CARTESIAN_POINT ( 'NONE',  ( -339.1964088526558498, -178.4886558749180949, 21.38919645685277970 ) ) ;
#27650 = ORIENTED_EDGE ( 'NONE', *, *, #36252, .F. ) ;
#27651 = FACE_OUTER_BOUND ( 'NONE', #14969, .T. ) ;
#27652 = ORIENTED_EDGE ( 'NONE', *, *, #24230, .T. ) ;
#27653 = AXIS2_PLACEMENT_3D ( 'NONE', #31930, #12213, #8790 ) ;
#27654 = DIRECTION ( 'NONE',  ( 0.2920567706369694982, 0.000000000000000000, 0.9564009842765243130 ) ) ;
#27655 = DIRECTION ( 'NONE',  ( 0.8455960035018272869, 0.000000000000000000, -0.5338233779647886257 ) ) ;
#27656 = AXIS2_PLACEMENT_3D ( 'NONE', #48372, #32597, #8683 ) ;
#27657 = CARTESIAN_POINT ( 'NONE',  ( -365.0160704661291788, -93.50000000000002842, 51.54700538379266561 ) ) ;
#27658 = DIRECTION ( 'NONE',  ( 0.1182731709213592358, 0.000000000000000000, 0.9929810960135178055 ) ) ;
#27659 = CARTESIAN_POINT ( 'NONE',  ( 75.78974234412359579, -177.1207230881787780, 13.49993235881449394 ) ) ;
#27660 = DIRECTION ( 'NONE',  ( 0.000000000000000000, 0.000000000000000000, 1.000000000000000000 ) ) ;
#27661 = CARTESIAN_POINT ( 'NONE',  ( 0.000000000000000000, -178.6659583184396354, -20.92168833550928042 ) ) ;
#27662 = CARTESIAN_POINT ( 'NONE',  ( -48.18706998087187543, -193.5000000000000000, -0.9564009842765152092 ) ) ;
#27664 = ORIENTED_EDGE ( 'NONE', *, *, #15996, .T. ) ;
#27663 = CARTESIAN_POINT ( 'NONE',  ( 42.45000882818163035, -189.7472609257535510, -84.30834960112932208 ) ) ;
#27665 = ORIENTED_EDGE ( 'NONE', *, *, #21925, .F. ) ;
#27666 = EDGE_CURVE ( 'NONE', #45739, #45186, #18678, .T. ) ;
#27667 = ADVANCED_FACE ( 'NONE', ( #42269 ), #50190, .T. ) ;
#27668 = PLANE ( 'NONE',  #26609 ) ;
#27669 = AXIS2_PLACEMENT_3D ( 'NONE', #11197, #18056, #34084 ) ;
#27670 = PLANE ( 'NONE',  #26273 ) ;
#27671 = ORIENTED_EDGE ( 'NONE', *, *, #39408, .T. ) ;
#27672 = ORIENTED_EDGE ( 'NONE', *, *, #51153, .T. ) ;
#27673 = PLANE ( 'NONE',  #13073 ) ;
#27674 = ORIENTED_EDGE ( 'NONE', *, *, #10394, .T. ) ;
#27675 = DIRECTION ( 'NONE',  ( 0.000000000000000000, 0.000000000000000000, -1.000000000000000000 ) ) ;
#27676 = LINE ( 'NONE', #48175, #46843 ) ;
#27677 = DIRECTION ( 'NONE',  ( 0.000000000000000000, 1.000000000000000000, -0.000000000000000000 ) ) ;
#27678 = DIRECTION ( 'NONE',  ( 1.000000000000000000, 0.000000000000000000, 0.000000000000000000 ) ) ;
#27679 = ORIENTED_EDGE ( 'NONE', *, *, #12917, .T. ) ;
#27680 = ORIENTED_EDGE ( 'NONE', *, *, #202, .F. ) ;
#27681 = ORIENTED_EDGE ( 'NONE', *, *, #40134, .F. ) ;
#27682 = CARTESIAN_POINT ( 'NONE',  ( -161.2555905272864436, -193.5000000000000000, -53.91167979418489864 ) ) ;
#27683 = CARTESIAN_POINT ( 'NONE',  ( -172.0042974347349229, -175.3837268820161057, 10.84123789944660388 ) ) ;
#27684 = EDGE_CURVE ( 'NONE', #16500, #4879, #41773, .T. ) ;
#27685 = DIRECTION ( 'NONE',  ( 0.000000000000000000, 0.000000000000000000, -1.000000000000000000 ) ) ;
#27686 = CARTESIAN_POINT ( 'NONE',  ( -170.8336150310145172, -189.7472609257535510, 25.58083653558488280 ) ) ;
#27687 = VERTEX_POINT ( 'NONE', #1566 ) ;
#27688 = CARTESIAN_POINT ( 'NONE',  ( 72.35619569422321717, -183.6283474603465606, 27.83926365844748574 ) ) ;
#27689 = DIRECTION ( 'NONE',  ( -0.000000000000000000, -0.000000000000000000, 1.000000000000000000 ) ) ;
#27690 = DIRECTION ( 'NONE',  ( 0.000000000000000000, -0.6631226582407885317, 0.7485107481711069655 ) ) ;
#27691 = EDGE_CURVE ( 'NONE', #40958, #28668, #9407, .T. ) ;
#27692 = EDGE_LOOP ( 'NONE', ( #35304, #33655, #13001, #27499 ) ) ;
#27693 = ORIENTED_EDGE ( 'NONE', *, *, #49509, .F. ) ;
#27694 = VERTEX_POINT ( 'NONE', #14185 ) ;
#27695 = DIRECTION ( 'NONE',  ( 0.000000000000000000, 0.000000000000000000, -1.000000000000000000 ) ) ;
#27696 = CARTESIAN_POINT ( 'NONE',  ( -78.64590280292340196, -175.3837268820161057, -121.3052580173827266 ) ) ;
#27697 = VERTEX_POINT ( 'NONE', #2066 ) ;
#27698 = DIRECTION ( 'NONE',  ( -0.000000000000000000, 1.000000000000000000, -0.000000000000000000 ) ) ;
#27699 = LINE ( 'NONE', #3012, #22019 ) ;
#27700 = DIRECTION ( 'NONE',  ( 0.000000000000000000, -1.000000000000000000, 0.000000000000000000 ) ) ;
#27701 = EDGE_LOOP ( 'NONE', ( #22057, #48875, #5253, #31182 ) ) ;
#27702 = DIRECTION ( 'NONE',  ( 1.000000000000000000, -0.000000000000000000, -0.000000000000000000 ) ) ;
#27703 = VECTOR ( 'NONE', #20915, 1000.000000000000114 ) ;
#27704 = VECTOR ( 'NONE', #29533, 1000.000000000000000 ) ;
#27705 = EDGE_LOOP ( 'NONE', ( #36078, #23091 ) ) ;
#27706 = CARTESIAN_POINT ( 'NONE',  ( -14.28570516517293854, -177.1207230881787780, 120.2323164553486521 ) ) ;
#27707 = DIRECTION ( 'NONE',  ( -0.3482016354343866471, 0.000000000000000000, -0.9374196611341253371 ) ) ;
#27708 = VERTEX_POINT ( 'NONE', #18111 ) ;
#27709 = LINE ( 'NONE', #3292, #44137 ) ;
#27710 = PLANE ( 'NONE',  #26389 ) ;
#27711 = FACE_OUTER_BOUND ( 'NONE', #25225, .T. ) ;
#27712 = FACE_OUTER_BOUND ( 'NONE', #2541, .T. ) ;
#27713 = ADVANCED_FACE ( 'NONE', ( #26765 ), #14682, .F. ) ;
#27714 = ORIENTED_EDGE ( 'NONE', *, *, #8646, .T. ) ;
#27715 = CARTESIAN_POINT ( 'NONE',  ( -339.1964088526558498, -102.1108035431470427, 54.98865587491797413 ) ) ;
#27716 = ORIENTED_EDGE ( 'NONE', *, *, #32043, .F. ) ;
#27717 = ORIENTED_EDGE ( 'NONE', *, *, #7024, .F. ) ;
#27718 = VECTOR ( 'NONE', #19154, 1000.000000000000000 ) ;
#27719 = LINE ( 'NONE', #43750, #15126 ) ;
#27721 = ORIENTED_EDGE ( 'NONE', *, *, #14816, .F. ) ;
#27720 = CARTESIAN_POINT ( 'NONE',  ( -332.3517673607765914, -121.8677111499054320, 59.00000000000001421 ) ) ;
#27722 = ORIENTED_EDGE ( 'NONE', *, *, #30836, .F. ) ;
#27723 = CARTESIAN_POINT ( 'NONE',  ( -147.2362428880188077, -183.6283474603465606, -74.98773087994455011 ) ) ;
#27724 = ADVANCED_FACE ( 'NONE', ( #21800 ), #46488, .F. ) ;
#27725 = FACE_OUTER_BOUND ( 'NONE', #46985, .T. ) ;
#27726 = EDGE_CURVE ( 'NONE', #13360, #29379, #45992, .T. ) ;
#27727 = ORIENTED_EDGE ( 'NONE', *, *, #35864, .T. ) ;
#27728 = CARTESIAN_POINT ( 'NONE',  ( -16.77927958806651887, -177.1207230881787780, -120.9136869416130082 ) ) ;
#27729 = PLANE ( 'NONE',  #17904 ) ;
#27730 = EDGE_LOOP ( 'NONE', ( #14107, #26562, #45691, #43809 ) ) ;
#27731 = CARTESIAN_POINT ( 'NONE',  ( -104.9497554727472703, -193.5000000000000000, -110.3950557015148632 ) ) ;
#27732 = LINE ( 'NONE', #4603, #48456 ) ;
#27733 = CARTESIAN_POINT ( 'NONE',  ( 116.9235303384055840, -193.5000000000000000, 10.00000000000000000 ) ) ;
#27734 = FACE_OUTER_BOUND ( 'NONE', #47690, .T. ) ;
#27735 = ORIENTED_EDGE ( 'NONE', *, *, #4818, .F. ) ;
#27736 = ORIENTED_EDGE ( 'NONE', *, *, #27174, .F. ) ;
#27737 = CIRCLE ( 'NONE', #48726, 125.0000000000000000 ) ;
#27739 = EDGE_LOOP ( 'NONE', ( #9412, #42182 ) ) ;
#27738 = VECTOR ( 'NONE', #51851, 1000.000000000000000 ) ;
#27740 = CYLINDRICAL_SURFACE ( 'NONE', #50119, 125.0000000000000000 ) ;
#27741 = LINE ( 'NONE', #31693, #5865 ) ;
#27742 = EDGE_CURVE ( 'NONE', #18024, #1807, #9707, .T. ) ;
#27743 = CARTESIAN_POINT ( 'NONE',  ( -336.3521761649653854, -169.4764303083190384, -38.55084767037274673 ) ) ;
#27744 = CARTESIAN_POINT ( 'NONE',  ( -332.3517673607765914, -164.5945333327934463, -42.41660376256285048 ) ) ;
#27745 = LINE ( 'NONE', #19609, #19678 ) ;
#27746 = VERTEX_POINT ( 'NONE', #22302 ) ;
#27747 = CARTESIAN_POINT ( 'NONE',  ( 65.12862465015751923, -177.1207230881787780, 49.69312418816387833 ) ) ;
#27748 = EDGE_LOOP ( 'NONE', ( #3593, #31604, #3978, #4973 ) ) ;
#27750 = VERTEX_POINT ( 'NONE', #34642 ) ;
#27749 = LINE ( 'NONE', #43782, #4635 ) ;
#27751 = EDGE_LOOP ( 'NONE', ( #17720, #5682, #6644, #17821 ) ) ;
#27752 = VECTOR ( 'NONE', #44305, 1000.000000000000000 ) ;
#27753 = DIRECTION ( 'NONE',  ( -0.000000000000000000, 1.000000000000000000, -0.000000000000000000 ) ) ;
#27754 = CARTESIAN_POINT ( 'NONE',  ( -37.08895481556041318, -177.1207230881787780, 124.4799742258550310 ) ) ;
#27755 = DIRECTION ( 'NONE',  ( 0.000000000000000000, 0.000000000000000000, -1.000000000000000000 ) ) ;
#27756 = CARTESIAN_POINT ( 'NONE',  ( -339.1964088526558498, -157.4273119900853146, -48.27201571435997352 ) ) ;
#27757 = ORIENTED_EDGE ( 'NONE', *, *, #39317, .F. ) ;
#27758 = DIRECTION ( 'NONE',  ( -0.000000000000000000, 0.9927088740980538617, -0.1205366802553232974 ) ) ;
#27759 = ORIENTED_EDGE ( 'NONE', *, *, #6337, .F. ) ;
#27760 = ORIENTED_EDGE ( 'NONE', *, *, #24005, .T. ) ;
#27761 = CARTESIAN_POINT ( 'NONE',  ( -84.19171550243319757, -189.7472609257535510, 119.7898618611247628 ) ) ;
#27762 = CARTESIAN_POINT ( 'NONE',  ( -55.71438232577009586, -175.3837268820161057, -124.7904286264580804 ) ) ;
#27763 = DIRECTION ( 'NONE',  ( 0.000000000000000000, 0.000000000000000000, -1.000000000000000000 ) ) ;
#27764 = VECTOR ( 'NONE', #18739, 1000.000000000000000 ) ;
#27765 = EDGE_CURVE ( 'NONE', #17878, #21936, #10215, .T. ) ;
#27766 = CARTESIAN_POINT ( 'NONE',  ( -48.47912675150885065, -183.6283474603465606, 6.938893903907228378E-15 ) ) ;
#27767 = DIRECTION ( 'NONE',  ( -1.000000000000000000, 0.000000000000000000, -0.000000000000000000 ) ) ;
#27768 = ORIENTED_EDGE ( 'NONE', *, *, #32716, .T. ) ;
#27769 = CARTESIAN_POINT ( 'NONE',  ( -339.1964088526558498, -79.66942718702553350, -39.49849221029258928 ) ) ;
#27770 = CARTESIAN_POINT ( 'NONE',  ( -260.0000000000000000, -63.50000000000000000, 60.00000000000000711 ) ) ;
#27771 = VECTOR ( 'NONE', #4206, 1000.000000000000114 ) ;
#27772 = ADVANCED_FACE ( 'NONE', ( #29934 ), #25993, .F. ) ;
#27773 = FACE_BOUND ( 'NONE', #14538, .T. ) ;
#27774 = VERTEX_POINT ( 'NONE', #18380 ) ;
#27775 = PLANE ( 'NONE',  #34851 ) ;
#27776 = FACE_OUTER_BOUND ( 'NONE', #28878, .T. ) ;
#27777 = ORIENTED_EDGE ( 'NONE', *, *, #51576, .T. ) ;
#27778 = DIRECTION ( 'NONE',  ( -0.000000000000000000, -0.8229838658936516893, 0.5680647467311626952 ) ) ;
#27779 = EDGE_CURVE ( 'NONE', #32119, #30672, #42013, .T. ) ;
#27780 = VERTEX_POINT ( 'NONE', #14432 ) ;
#27781 = EDGE_CURVE ( 'NONE', #28621, #2310, #10740, .T. ) ;
#27782 = EDGE_CURVE ( 'NONE', #35294, #23517, #38069, .T. ) ;
#27783 = FACE_OUTER_BOUND ( 'NONE', #23446, .T. ) ;
#27784 = ADVANCED_FACE ( 'NONE', ( #13647 ), #26498, .F. ) ;
#27785 = AXIS2_PLACEMENT_3D ( 'NONE', #22388, #38411, #34218 ) ;
#27787 = ADVANCED_FACE ( 'NONE', ( #22827 ), #29726, .T. ) ;
#27786 = FACE_BOUND ( 'NONE', #48224, .T. ) ;
#27788 = DIRECTION ( 'NONE',  ( -0.000000000000000000, 0.000000000000000000, 1.000000000000000000 ) ) ;
#27789 = DIRECTION ( 'NONE',  ( 0.8124868780056863082, 0.000000000000000000, -0.5829794791144649047 ) ) ;
#27790 = ORIENTED_EDGE ( 'NONE', *, *, #38650, .F. ) ;
#27791 = ORIENTED_EDGE ( 'NONE', *, *, #20480, .F. ) ;
#27792 = LINE ( 'NONE', #43827, #5790 ) ;
#27793 = ORIENTED_EDGE ( 'NONE', *, *, #15003, .T. ) ;
#27794 = DIRECTION ( 'NONE',  ( 0.000000000000000000, 0.000000000000000000, 1.000000000000000000 ) ) ;
#27795 = DIRECTION ( 'NONE',  ( 0.000000000000000000, -1.000000000000000000, 0.000000000000000000 ) ) ;
#27796 = AXIS2_PLACEMENT_3D ( 'NONE', #39017, #38520, #23006 ) ;
#27797 = AXIS2_PLACEMENT_3D ( 'NONE', #25141, #24869, #49578 ) ;
#27798 = AXIS2_PLACEMENT_3D ( 'NONE', #15459, #31466, #11499 ) ;
#27799 = PRESENTATION_STYLE_ASSIGNMENT (( #15481 ) ) ;
#27800 = FACE_OUTER_BOUND ( 'NONE', #1832, .T. ) ;
#27801 = EDGE_LOOP ( 'NONE', ( #40385, #34229, #17759, #13049 ) ) ;
#27804 = EDGE_LOOP ( 'NONE', ( #34266, #32829, #45675, #6082 ) ) ;
#27803 = PLANE ( 'NONE',  #3767 ) ;
#27802 = CARTESIAN_POINT ( 'NONE',  ( -336.3521761649653854, -107.5615171630107056, 57.84431488793861575 ) ) ;
#27805 = EDGE_LOOP ( 'NONE', ( #7149, #31348 ) ) ;
#27806 = CARTESIAN_POINT ( 'NONE',  ( -1.230335819511603423, -183.6283474603465606, 115.7261930397108216 ) ) ;
#27807 = ORIENTED_EDGE ( 'NONE', *, *, #37450, .F. ) ;
#27808 = DIRECTION ( 'NONE',  ( -0.6965510290629982615, 0.000000000000000000, 0.7175072570443298270 ) ) ;
#27809 = ORIENTED_EDGE ( 'NONE', *, *, #37589, .T. ) ;
#27810 = DIRECTION ( 'NONE',  ( -0.9027978299657387629, 0.000000000000000000, -0.4300652022765304450 ) ) ;
#27811 = ORIENTED_EDGE ( 'NONE', *, *, #4474, .F. ) ;
#27813 = PLANE ( 'NONE',  #35870 ) ;
#27812 = CARTESIAN_POINT ( 'NONE',  ( -48.47912675150885065, -175.3837268820161057, 6.938893903907228378E-15 ) ) ;
#27814 = ORIENTED_EDGE ( 'NONE', *, *, #5754, .F. ) ;
#27815 = AXIS2_PLACEMENT_3D ( 'NONE', #41484, #38765, #5785 ) ;
#27816 = DIRECTION ( 'NONE',  ( -0.000000000000000000, 1.000000000000000000, -0.000000000000000000 ) ) ;
#27817 = ORIENTED_EDGE ( 'NONE', *, *, #4791, .F. ) ;
#27818 = CARTESIAN_POINT ( 'NONE',  ( -82.67254833784559764, -193.5000000000000000, -120.2323164553483963 ) ) ;
#27820 = AXIS2_PLACEMENT_3D ( 'NONE', #13861, #26448, #18576 ) ;
#27819 = CARTESIAN_POINT ( 'NONE',  ( -145.0195698084541505, -189.7472609257535510, 79.40367028273128369 ) ) ;
#27821 = FACE_OUTER_BOUND ( 'NONE', #28275, .T. ) ;
#27822 = DIRECTION ( 'NONE',  ( -0.7948544414133608127, 0.000000000000000000, 0.6068001458185834363 ) ) ;
#27823 = DIRECTION ( 'NONE',  ( 0.9473263538541899509, 0.000000000000000000, 0.3202698538628415692 ) ) ;
#27824 = PLANE ( 'NONE',  #7919 ) ;
#27825 = EDGE_CURVE ( 'NONE', #20039, #50250, #20823, .T. ) ;
#27826 = ADVANCED_FACE ( 'NONE', ( #4798 ), #41294, .T. ) ;
#27827 = ORIENTED_EDGE ( 'NONE', *, *, #41730, .F. ) ;
#27828 = EDGE_CURVE ( 'NONE', #39416, #14560, #5849, .T. ) ;
#27829 = CARTESIAN_POINT ( 'NONE',  ( 22.37192613399954411, 5.637851296924623057E-15, -6.938893903907228378E-15 ) ) ;
#27830 = CARTESIAN_POINT ( 'NONE',  ( -108.4791267515088435, -132.5479369270331915, 60.00000000000000711 ) ) ;
#27831 = DIRECTION ( 'NONE',  ( -0.000000000000000000, 1.000000000000000000, -0.000000000000000000 ) ) ;
#27832 = CARTESIAN_POINT ( 'NONE',  ( -330.4913330509368166, -64.99044476834247064, -7.608018572113060429 ) ) ;
#27833 = ORIENTED_EDGE ( 'NONE', *, *, #10118, .F. ) ;
#27834 = CARTESIAN_POINT ( 'NONE',  ( -48.47912675150885065, -175.3837268820161057, 6.938893903907228378E-15 ) ) ;
#27835 = EDGE_CURVE ( 'NONE', #18649, #46522, #9771, .T. ) ;
#27836 = AXIS2_PLACEMENT_3D ( 'NONE', #45070, #48743, #25093 ) ;
#27837 = DIRECTION ( 'NONE',  ( 0.000000000000000000, 0.000000000000000000, 1.000000000000000000 ) ) ;
#27838 = LINE ( 'NONE', #39658, #38343 ) ;
#27839 = ORIENTED_EDGE ( 'NONE', *, *, #25662, .T. ) ;
#27840 = VERTEX_POINT ( 'NONE', #1632 ) ;
#27841 = ADVANCED_FACE ( 'NONE', ( #45775 ), #45005, .T. ) ;
#27842 = AXIS2_PLACEMENT_3D ( 'NONE', #3535, #19568, #15637 ) ;
#27843 = VERTEX_POINT ( 'NONE', #41041 ) ;
#27844 = EDGE_CURVE ( 'NONE', #34734, #17876, #5056, .T. ) ;
#27845 = CIRCLE ( 'NONE', #4335, 10.00000000000000178 ) ;
#27846 = CARTESIAN_POINT ( 'NONE',  ( -336.3521761649654422, -161.4024510877913485, 45.24454186338643780 ) ) ;
#27847 = ADVANCED_FACE ( 'NONE', ( #21338 ), #16632, .T. ) ;
#27848 = DIRECTION ( 'NONE',  ( -0.000000000000000000, 0.5680647467311540355, -0.8229838658936575735 ) ) ;
#27849 = CARTESIAN_POINT ( 'NONE',  ( -137.9639882952644712, -183.6283474603465606, 87.27805883780237650 ) ) ;
#27850 = LINE ( 'NONE', #23909, #48045 ) ;
#27851 = EDGE_CURVE ( 'NONE', #10865, #10929, #33156, .T. ) ;
#27852 = VERTEX_POINT ( 'NONE', #1093 ) ;
#27853 = CARTESIAN_POINT ( 'NONE',  ( 4.316855663795568177, 53.18022804202947640, -19.20662862702307194 ) ) ;
#27854 = AXIS2_PLACEMENT_3D ( 'NONE', #8998, #40251, #580 ) ;
#27855 = ORIENTED_EDGE ( 'NONE', *, *, #38181, .F. ) ;
#27856 = VECTOR ( 'NONE', #29134, 1000.000000000000114 ) ;
#27857 = VERTEX_POINT ( 'NONE', #17143 ) ;
#27858 = AXIS2_PLACEMENT_3D ( 'NONE', #30083, #21421, #17505 ) ;
#27859 = VERTEX_POINT ( 'NONE', #17418 ) ;
#27860 = FACE_OUTER_BOUND ( 'NONE', #46388, .T. ) ;
#27861 = ORIENTED_EDGE ( 'NONE', *, *, #3104, .T. ) ;
#27862 = ADVANCED_FACE ( 'NONE', ( #41831 ), #579, .T. ) ;
#27863 = DIRECTION ( 'NONE',  ( 1.000000000000000000, 0.000000000000000000, 0.000000000000000000 ) ) ;
#27864 = CARTESIAN_POINT ( 'NONE',  ( 24.63024857337166296, -193.5000000000000000, 101.3904297239426597 ) ) ;
#27867 = ORIENTED_EDGE ( 'NONE', *, *, #21853, .F. ) ;
#27866 = DIRECTION ( 'NONE',  ( 0.000000000000000000, 0.000000000000000000, -1.000000000000000000 ) ) ;
#27865 = PLANE ( 'NONE',  #34210 ) ;
#27868 = DIRECTION ( 'NONE',  ( 0.9473263538541946138, 0.000000000000000000, -0.3202698538628279690 ) ) ;
#27869 = ORIENTED_EDGE ( 'NONE', *, *, #34592, .T. ) ;
#27870 = CARTESIAN_POINT ( 'NONE',  ( -136.1415351158078693, -193.5000000000000000, -89.10837311819173578 ) ) ;
#27871 = VECTOR ( 'NONE', #25453, 1000.000000000000000 ) ;
#27872 = VERTEX_POINT ( 'NONE', #13455 ) ;
#27873 = LINE ( 'NONE', #9669, #47605 ) ;
#27874 = CARTESIAN_POINT ( 'NONE',  ( 17.98688506184921820, -177.1207230881787780, 104.6823626202124444 ) ) ;
#27876 = DIRECTION ( 'NONE',  ( 0.2635871660690715101, 0.000000000000000000, -0.9646355819083576311 ) ) ;
#27875 = CARTESIAN_POINT ( 'NONE',  ( -339.1964088526558498, -73.83865025250274527, 33.67120938215247605 ) ) ;
#27877 = EDGE_LOOP ( 'NONE', ( #12189, #20014, #16719, #5178 ) ) ;
#27878 = VECTOR ( 'NONE', #13709, 1000.000000000000114 ) ;
#27879 = EDGE_CURVE ( 'NONE', #40321, #14309, #13198, .T. ) ;
#27880 = DIRECTION ( 'NONE',  ( 0.000000000000000000, -6.753856733136369375E-14, -1.000000000000000000 ) ) ;
#27881 = LINE ( 'NONE', #31842, #11892 ) ;
#27882 = ORIENTED_EDGE ( 'NONE', *, *, #21094, .F. ) ;
#27883 =( LENGTH_UNIT ( ) NAMED_UNIT ( * ) SI_UNIT ( .MILLI., .METRE. ) );
#27884 = DIRECTION ( 'NONE',  ( 0.000000000000000000, 1.063963731932441632E-14, -1.000000000000000000 ) ) ;
#27885 = DIRECTION ( 'NONE',  ( 0.000000000000000000, 0.000000000000000000, -1.000000000000000000 ) ) ;
#27886 = ADVANCED_FACE ( 'NONE', ( #28682 ), #37359, .F. ) ;
#27887 = ADVANCED_FACE ( 'NONE', ( #9510 ), #9258, .F. ) ;
#27888 = EDGE_CURVE ( 'NONE', #29772, #8372, #49479, .T. ) ;
#27889 = EDGE_LOOP ( 'NONE', ( #50913, #8122, #44021, #18148 ) ) ;
#27890 = EDGE_CURVE ( 'NONE', #3230, #45161, #26235, .T. ) ;
#27891 = CARTESIAN_POINT ( 'NONE',  ( -127.0132498732366173, -177.1207230881787780, 97.24912084693264092 ) ) ;
#27892 = AXIS2_PLACEMENT_3D ( 'NONE', #24692, #16833, #32836 ) ;
#27894 = VECTOR ( 'NONE', #46655, 1000.000000000000114 ) ;
#27893 = LINE ( 'NONE', #23956, #50814 ) ;
#27895 = ADVANCED_FACE ( 'NONE', ( #42077 ), #6098, .T. ) ;
#27896 = VERTEX_POINT ( 'NONE', #30257 ) ;
#27897 = DIRECTION ( 'NONE',  ( 0.000000000000000000, 1.000000000000000000, 0.000000000000000000 ) ) ;
#27898 = ORIENTED_EDGE ( 'NONE', *, *, #36803, .T. ) ;
#27899 = AXIS2_PLACEMENT_3D ( 'NONE', #34056, #9625, #38247 ) ;
#27900 = VECTOR ( 'NONE', #17242, 1000.000000000000000 ) ;
#27901 = CARTESIAN_POINT ( 'NONE',  ( -305.0000000000000568, -173.1613497474968710, -33.67120938215310844 ) ) ;
#27902 = EDGE_CURVE ( 'NONE', #25533, #8754, #50502, .T. ) ;
#27903 = DIRECTION ( 'NONE',  ( -0.000000000000000000, 1.000000000000000000, 0.000000000000000000 ) ) ;
#27904 = DIRECTION ( 'NONE',  ( 0.000000000000000000, -1.000000000000000000, 0.000000000000000000 ) ) ;
#27905 = FACE_OUTER_BOUND ( 'NONE', #18445, .T. ) ;
#27906 = CARTESIAN_POINT ( 'NONE',  ( -162.0868781531755758, -193.5000000000000000, -49.69312418816308963 ) ) ;
#27907 = EDGE_CURVE ( 'NONE', #40028, #51485, #34705, .T. ) ;
#27908 = EDGE_CURVE ( 'NONE', #17428, #1315, #22116, .T. ) ;
#27909 = LINE ( 'NONE', #7444, #10353 ) ;
#27910 = EDGE_CURVE ( 'NONE', #11425, #11764, #38127, .T. ) ;
#27911 = DIRECTION ( 'NONE',  ( 0.000000000000000000, 2.567390744445674500E-14, 1.000000000000000000 ) ) ;
#27912 = PLANE ( 'NONE',  #21362 ) ;
#27914 = EDGE_LOOP ( 'NONE', ( #51987, #40364, #5723, #34361 ) ) ;
#27913 = PLANE ( 'NONE',  #39593 ) ;
#27915 = VECTOR ( 'NONE', #5945, 1000.000000000000000 ) ;
#27916 = ADVANCED_FACE ( 'NONE', ( #10039 ), #34454, .T. ) ;
#27917 = ORIENTED_EDGE ( 'NONE', *, *, #27554, .F. ) ;
#27918 = CARTESIAN_POINT ( 'NONE',  ( -19.18792875895802652, -175.3837268820161057, -120.4907712303050715 ) ) ;
#27919 = EDGE_CURVE ( 'NONE', #51592, #50821, #11046, .T. ) ;
#27920 = CIRCLE ( 'NONE', #43008, 60.00000000000000000 ) ;
#27921 = CYLINDRICAL_SURFACE ( 'NONE', #45618, 125.0000000000000000 ) ;
#27922 = ORIENTED_EDGE ( 'NONE', *, *, #23139, .F. ) ;
#27923 = VERTEX_POINT ( 'NONE', #34202 ) ;
#27924 = ORIENTED_EDGE ( 'NONE', *, *, #36055, .T. ) ;
#27925 = DIRECTION ( 'NONE',  ( 0.000000000000000000, 0.000000000000000000, 1.000000000000000000 ) ) ;
#27926 = CARTESIAN_POINT ( 'NONE',  ( 73.32544842769510751, -193.5000000000000000, -23.23456943914041517 ) ) ;
#27927 = DIRECTION ( 'NONE',  ( 0.000000000000000000, -1.000000000000000000, 0.000000000000000000 ) ) ;
#27928 = DIRECTION ( 'NONE',  ( 0.000000000000000000, 0.000000000000000000, 1.000000000000000000 ) ) ;
#27930 = VERTEX_POINT ( 'NONE', #50248 ) ;
#27929 = AXIS2_PLACEMENT_3D ( 'NONE', #23637, #43371, #30754 ) ;
#27931 = VECTOR ( 'NONE', #26238, 1000.000000000000000 ) ;
#27932 = ORIENTED_EDGE ( 'NONE', *, *, #1208, .T. ) ;
#27933 = VERTEX_POINT ( 'NONE', #42600 ) ;
#27934 = EDGE_CURVE ( 'NONE', #49365, #43643, #27075, .T. ) ;
#27935 = LINE ( 'NONE', #43965, #15721 ) ;
#27936 = FACE_OUTER_BOUND ( 'NONE', #10884, .T. ) ;
#27937 = LINE ( 'NONE', #15611, #1412 ) ;
#27938 = CIRCLE ( 'NONE', #45595, 125.0000000000000000 ) ;
#27939 = PLANE ( 'NONE',  #42159 ) ;
#27940 = DIRECTION ( 'NONE',  ( 0.000000000000000000, 0.7485107481710999711, -0.6631226582407964143 ) ) ;
#27941 = ORIENTED_EDGE ( 'NONE', *, *, #11193, .T. ) ;
#27942 = CARTESIAN_POINT ( 'NONE',  ( 64.72501964220592185, -189.7472609257535510, 53.00774697410174952 ) ) ;
#27943 = AXIS2_PLACEMENT_3D ( 'NONE', #4333, #8526, #19585 ) ;
#27944 = CARTESIAN_POINT ( 'NONE',  ( -48.47912675150885065, -120.5000000000000284, 6.938893903907228378E-15 ) ) ;
#27945 = DIRECTION ( 'NONE',  ( -0.1768902751225592818, 0.000000000000000000, -0.9842305779475992722 ) ) ;
#27946 = DIRECTION ( 'NONE',  ( 0.000000000000000000, 0.000000000000000000, 1.000000000000000000 ) ) ;
#27947 = ORIENTED_EDGE ( 'NONE', *, *, #51670, .F. ) ;
#27948 = ORIENTED_EDGE ( 'NONE', *, *, #1981, .F. ) ;
#27949 = EDGE_LOOP ( 'NONE', ( #28730, #44140, #1697, #8297 ) ) ;
#27950 = DIRECTION ( 'NONE',  ( -0.000000000000000000, 1.000000000000000000, -0.000000000000000000 ) ) ;
#27951 = DIRECTION ( 'NONE',  ( 0.000000000000000000, -1.000000000000000000, 0.000000000000000000 ) ) ;
#27952 = EDGE_LOOP ( 'NONE', ( #33472, #1047, #12413, #38679 ) ) ;
#27953 = DIRECTION ( 'NONE',  ( 0.000000000000000000, -0.1205366802553303057, -0.9927088740980530845 ) ) ;
#27954 = AXIS2_PLACEMENT_3D ( 'NONE', #49962, #13958, #46038 ) ;
#27955 = FACE_OUTER_BOUND ( 'NONE', #39455, .T. ) ;
#27956 = ADVANCED_FACE ( 'NONE', ( #26306 ), #31024, .T. ) ;
#27958 = EDGE_CURVE ( 'NONE', #30593, #12246, #51431, .T. ) ;
#27957 = DIRECTION ( 'NONE',  ( 0.000000000000000000, 0.000000000000000000, 1.000000000000000000 ) ) ;
#27959 = ORIENTED_EDGE ( 'NONE', *, *, #41242, .F. ) ;
#27960 = DIRECTION ( 'NONE',  ( -0.000000000000000000, 1.000000000000000000, 0.000000000000000000 ) ) ;
#27961 = AXIS2_PLACEMENT_3D ( 'NONE', #20554, #45525, #25539 ) ;
#27962 = EDGE_CURVE ( 'NONE', #37621, #17577, #33784, .T. ) ;
#27963 = ORIENTED_EDGE ( 'NONE', *, *, #16190, .F. ) ;
#27964 = CARTESIAN_POINT ( 'NONE',  ( -48.47912675150885065, -189.7472609257535510, 6.938893903907228378E-15 ) ) ;
#27965 = EDGE_LOOP ( 'NONE', ( #4687, #3725, #27265, #30856 ) ) ;
#27966 = DIRECTION ( 'NONE',  ( -1.000000000000000000, 0.000000000000000000, 0.000000000000000000 ) ) ;
#27967 = DIRECTION ( 'NONE',  ( -0.000000000000000000, 1.000000000000000000, -0.000000000000000000 ) ) ;
#27968 = ORIENTED_EDGE ( 'NONE', *, *, #22106, .F. ) ;
#27969 = CARTESIAN_POINT ( 'NONE',  ( -48.18706998087187543, -183.6283474603465606, -0.9564009842765152092 ) ) ;
#27970 = CARTESIAN_POINT ( 'NONE',  ( -170.7635349987907603, -175.3837268820161057, -25.91377046305877130 ) ) ;
#27971 = DIRECTION ( 'NONE',  ( -0.000000000000000000, 1.000000000000000000, -0.000000000000000000 ) ) ;
#27972 = AXIS2_PLACEMENT_3D ( 'NONE', #31836, #43911, #23940 ) ;
#27973 = CYLINDRICAL_SURFACE ( 'NONE', #2269, 125.0000000000000000 ) ;
#27974 = ORIENTED_EDGE ( 'NONE', *, *, #23977, .F. ) ;
#27975 = CARTESIAN_POINT ( 'NONE',  ( -158.1873290247468447, -193.5000000000000000, 57.79541595648305474 ) ) ;
#27976 = ORIENTED_EDGE ( 'NONE', *, *, #43523, .T. ) ;
#27977 = ORIENTED_EDGE ( 'NONE', *, *, #51654, .F. ) ;
#27978 = EDGE_CURVE ( 'NONE', #4174, #33649, #9486, .T. ) ;
#27979 = PLANE ( 'NONE',  #43650 ) ;
#27981 = ORIENTED_EDGE ( 'NONE', *, *, #26318, .F. ) ;
#27980 = CARTESIAN_POINT ( 'NONE',  ( -48.88225018079680950, -183.6283474603465606, -0.9151456172430169067 ) ) ;
#27982 = ORIENTED_EDGE ( 'NONE', *, *, #11177, .F. ) ;
#27983 = FACE_OUTER_BOUND ( 'NONE', #4877, .T. ) ;
#27984 = ADVANCED_FACE ( 'NONE', ( #18693 ), #7120, .F. ) ;
#27985 = DIRECTION ( 'NONE',  ( 1.000000000000000000, -0.000000000000000000, 0.000000000000000000 ) ) ;
#27986 = VERTEX_POINT ( 'NONE', #26565 ) ;
#27987 = DIRECTION ( 'NONE',  ( 0.000000000000000000, -0.000000000000000000, 1.000000000000000000 ) ) ;
#27988 = DIRECTION ( 'NONE',  ( -1.000000000000000000, -0.000000000000000000, 0.000000000000000000 ) ) ;
#27989 = VERTEX_POINT ( 'NONE', #50754 ) ;
#27990 = DIRECTION ( 'NONE',  ( -0.000000000000000000, 1.000000000000000000, -0.000000000000000000 ) ) ;
#27991 = DIRECTION ( 'NONE',  ( 0.000000000000000000, 0.000000000000000000, -1.000000000000000000 ) ) ;
#27992 = AXIS2_PLACEMENT_3D ( 'NONE', #46473, #10456, #34629 ) ;
#27993 = DIRECTION ( 'NONE',  ( -0.000000000000000000, -0.5680647467311485954, 0.8229838658936613482 ) ) ;
#27994 = CARTESIAN_POINT ( 'NONE',  ( -46.00000000000000711, 20.00000000000000000, -46.00000000000000000 ) ) ;
#27995 = ORIENTED_EDGE ( 'NONE', *, *, #46733, .T. ) ;
#27996 = VERTEX_POINT ( 'NONE', #30770 ) ;
#27997 = VECTOR ( 'NONE', #46470, 1000.000000000000000 ) ;
#27998 = EDGE_LOOP ( 'NONE', ( #42676, #34554, #31180, #29553 ) ) ;
#27999 = FACE_OUTER_BOUND ( 'NONE', #48328, .T. ) ;
#28000 = PLANE ( 'NONE',  #25169 ) ;
#28001 = DIRECTION ( 'NONE',  ( 0.000000000000000000, 1.000000000000000000, -0.000000000000000000 ) ) ;
#28002 = FACE_BOUND ( 'NONE', #10911, .T. ) ;
#28003 = LINE ( 'NONE', #15684, #14628 ) ;
#28004 = VERTEX_POINT ( 'NONE', #6861 ) ;
#28005 = CARTESIAN_POINT ( 'NONE',  ( -339.1964088526558498, -64.99044476834248485, -7.608018572113150135 ) ) ;
#28006 = ORIENTED_EDGE ( 'NONE', *, *, #4476, .T. ) ;
#28008 = VERTEX_POINT ( 'NONE', #46819 ) ;
#28007 = PLANE ( 'NONE',  #26459 ) ;
#28009 = ORIENTED_EDGE ( 'NONE', *, *, #20431, .T. ) ;
#28010 = CYLINDRICAL_SURFACE ( 'NONE', #12337, 125.0000000000000000 ) ;
#28011 = DIRECTION ( 'NONE',  ( 0.000000000000000000, 1.000000000000000000, 0.000000000000000000 ) ) ;
#28012 = CARTESIAN_POINT ( 'NONE',  ( 73.32544842769512172, -183.6283474603465606, -23.23456943914042228 ) ) ;
#28013 = ADVANCED_FACE ( 'NONE', ( #10801 ), #26821, .F. ) ;
#28014 = LINE ( 'NONE', #12515, #36009 ) ;
#28015 = ORIENTED_EDGE ( 'NONE', *, *, #45603, .F. ) ;
#28016 = CARTESIAN_POINT ( 'NONE',  ( -332.3517673607765914, -120.8677111499054320, 59.00000000000000000 ) ) ;
#28017 = EDGE_LOOP ( 'NONE', ( #1680, #29636, #43180, #23993 ) ) ;
#28018 = VERTEX_POINT ( 'NONE', #15021 ) ;
#28019 = DIRECTION ( 'NONE',  ( -0.000000000000000000, -0.9927088740980530845, 0.1205366802553303057 ) ) ;
#28020 = CARTESIAN_POINT ( 'NONE',  ( -137.2261550162227195, -177.1207230881787780, 86.60307583628417660 ) ) ;
#28021 = CARTESIAN_POINT ( 'NONE',  ( 21.47984469475713354, -175.3837268820161057, 102.3804074221065292 ) ) ;
#28022 = AXIS2_PLACEMENT_3D ( 'NONE', #9373, #32762, #48805 ) ;
#28023 = FACE_OUTER_BOUND ( 'NONE', #6937, .T. ) ;
#28024 = AXIS2_PLACEMENT_3D ( 'NONE', #19185, #3151, #34935 ) ;
#28025 = CARTESIAN_POINT ( 'NONE',  ( -336.3521761649654422, -98.41210887299327226, -53.46519113769058151 ) ) ;
#28026 = FACE_OUTER_BOUND ( 'NONE', #19500, .T. ) ;
#28027 = ORIENTED_EDGE ( 'NONE', *, *, #23615, .F. ) ;
#28028 = CARTESIAN_POINT ( 'NONE',  ( -336.3521761649654422, -111.7106844931459619, -58.83036664750484590 ) ) ;
#28029 = CARTESIAN_POINT ( 'NONE',  ( -332.3517673607765914, -158.3591674452439122, -47.62880233550485087 ) ) ;
#28030 = AXIS2_PLACEMENT_3D ( 'NONE', #11742, #20668, #40120 ) ;
#28031 = FACE_BOUND ( 'NONE', #15257, .T. ) ;
#28032 = ORIENTED_EDGE ( 'NONE', *, *, #6632, .F. ) ;
#28033 = ADVANCED_FACE ( 'NONE', ( #47069 ), #43112, .T. ) ;
#28034 = DIRECTION ( 'NONE',  ( 0.000000000000000000, 0.000000000000000000, 1.000000000000000000 ) ) ;
#28035 = DIRECTION ( 'NONE',  ( -0.000000000000000000, 0.8660254037844354880, 0.5000000000000054401 ) ) ;
#28036 = ORIENTED_EDGE ( 'NONE', *, *, #13136, .F. ) ;
#28037 = DIRECTION ( 'NONE',  ( 0.000000000000000000, -1.000000000000000000, -1.387778780781445182E-16 ) ) ;
#28038 = VECTOR ( 'NONE', #18773, 1000.000000000000227 ) ;
#28039 = VERTEX_POINT ( 'NONE', #51795 ) ;
#28040 = DIRECTION ( 'NONE',  ( -0.9027978299657387629, 0.000000000000000000, -0.4300652022765304450 ) ) ;
#28041 = FACE_BOUND ( 'NONE', #36449, .T. ) ;
#28042 = FACE_OUTER_BOUND ( 'NONE', #50221, .T. ) ;
#28043 = ADVANCED_BREP_SHAPE_REPRESENTATION ( '', ( #36851, #31742 ), #49435 ) ;
#28044 = EDGE_CURVE ( 'NONE', #47044, #19921, #20345, .T. ) ;
#28045 = FACE_OUTER_BOUND ( 'NONE', #42049, .T. ) ;
#28046 = EDGE_LOOP ( 'NONE', ( #46619, #3960, #5142, #30011 ) ) ;
#28047 = ORIENTED_EDGE ( 'NONE', *, *, #50360, .T. ) ;
#28048 = CARTESIAN_POINT ( 'NONE',  ( -152.8713435144644848, -193.5000000000000000, -68.75510947788595217 ) ) ;
#28049 = EDGE_LOOP ( 'NONE', ( #6261, #5423, #31085, #37423 ) ) ;
#28050 = FACE_OUTER_BOUND ( 'NONE', #37098, .T. ) ;
#28051 = VECTOR ( 'NONE', #13417, 999.9999999999998863 ) ;
#28052 = CARTESIAN_POINT ( 'NONE',  ( -164.2512865680372727, -189.7472609257535510, -47.13604789772048775 ) ) ;
#28053 = AXIS2_PLACEMENT_3D ( 'NONE', #31515, #36485, #8132 ) ;
#28054 = AXIS2_PLACEMENT_3D ( 'NONE', #17976, #34756, #2192 ) ;
#28055 = EDGE_CURVE ( 'NONE', #15026, #24837, #24190, .T. ) ;
#28056 = DIRECTION ( 'NONE',  ( 0.000000000000000000, 0.000000000000000000, 1.000000000000000000 ) ) ;
#28057 = ORIENTED_EDGE ( 'NONE', *, *, #22640, .T. ) ;
#28060 = ORIENTED_EDGE ( 'NONE', *, *, #22399, .T. ) ;
#28059 = DIRECTION ( 'NONE',  ( -0.8858462335218260097, 0.000000000000000000, -0.4639789333096864810 ) ) ;
#28058 = FACE_OUTER_BOUND ( 'NONE', #10183, .T. ) ;
#28061 = ORIENTED_EDGE ( 'NONE', *, *, #19261, .T. ) ;
#28062 = DIRECTION ( 'NONE',  ( 0.1768902751225802927, 0.000000000000000000, -0.9842305779475953864 ) ) ;
#28063 = VERTEX_POINT ( 'NONE', #19980 ) ;
#28064 = DIRECTION ( 'NONE',  ( -0.9785564922995046988, 0.000000000000000000, 0.2059786187410953262 ) ) ;
#28065 = ORIENTED_EDGE ( 'NONE', *, *, #22869, .T. ) ;
#28066 = EDGE_CURVE ( 'NONE', #7899, #9774, #23908, .T. ) ;
#28067 = CARTESIAN_POINT ( 'NONE',  ( -336.3521761649654422, -64.61288906875131488, 4.498567634385603142 ) ) ;
#28068 = ORIENTED_EDGE ( 'NONE', *, *, #30813, .F. ) ;
#28070 = DIRECTION ( 'NONE',  ( 0.000000000000000000, 1.000000000000000000, -0.000000000000000000 ) ) ;
#28069 = DIRECTION ( 'NONE',  ( 0.000000000000000000, -1.000000000000000000, -0.000000000000000000 ) ) ;
#28071 = VECTOR ( 'NONE', #2159, 1000.000000000000000 ) ;
#28072 = VERTEX_POINT ( 'NONE', #47848 ) ;
#28073 = EDGE_CURVE ( 'NONE', #7018, #19848, #43886, .T. ) ;
#28074 = ORIENTED_EDGE ( 'NONE', *, *, #2756, .F. ) ;
#28075 = CARTESIAN_POINT ( 'NONE',  ( -114.9451385648676336, -177.1207230881787780, -104.6823626202119613 ) ) ;
#28076 = ADVANCED_FACE ( 'NONE', ( #11302 ), #27339, .F. ) ;
#28077 = CARTESIAN_POINT ( 'NONE',  ( -336.3521761649654422, -125.1322888500942270, -59.00000000000002132 ) ) ;
#28078 = CARTESIAN_POINT ( 'NONE',  ( -332.3517673607765914, -100.1170788342122080, 54.23253582808833073 ) ) ;
#28079 = FACE_OUTER_BOUND ( 'NONE', #13794, .T. ) ;
#28080 = CARTESIAN_POINT ( 'NONE',  ( 46.00000000000000711, 20.00000000000000000, -46.00000000000000000 ) ) ;
#28081 = CARTESIAN_POINT ( 'NONE',  ( -336.3521761649654422, -127.9985676343858501, 58.88711093124869222 ) ) ;
#28082 = ORIENTED_EDGE ( 'NONE', *, *, #35915, .F. ) ;
#28083 = CARTESIAN_POINT ( 'NONE',  ( 3.319108545074538785, 13.10393101051890419, 46.36183385973379956 ) ) ;
#28084 = LINE ( 'NONE', #40187, #8677 ) ;
#28085 = CARTESIAN_POINT ( 'NONE',  ( 76.21810084846656252, -177.1207230881787780, -8.694908215727984668 ) ) ;
#28086 = CARTESIAN_POINT ( 'NONE',  ( -157.1522883217072604, -189.7472609257535510, 59.71720175837172917 ) ) ;
#28087 = ORIENTED_EDGE ( 'NONE', *, *, #9928, .F. ) ;
#28088 = VECTOR ( 'NONE', #8764, 1000.000000000000000 ) ;
#28089 = CARTESIAN_POINT ( 'NONE',  ( -48.47912675150885065, -177.1207230881787780, 6.938893903907228378E-15 ) ) ;
#28090 = EDGE_CURVE ( 'NONE', #31327, #4741, #20234, .T. ) ;
#28091 = CIRCLE ( 'NONE', #18059, 60.00000000000000000 ) ;
#28092 = VECTOR ( 'NONE', #6536, 1000.000000000000000 ) ;
#28093 = DIRECTION ( 'NONE',  ( 0.000000000000000000, -0.000000000000000000, -1.000000000000000000 ) ) ;
#28094 = LINE ( 'NONE', #20477, #2655 ) ;
#28095 = ORIENTED_EDGE ( 'NONE', *, *, #19315, .F. ) ;
#28096 = ORIENTED_EDGE ( 'NONE', *, *, #31929, .T. ) ;
#28097 = EDGE_LOOP ( 'NONE', ( #12773, #32239, #31547, #9934 ) ) ;
#28098 = DIRECTION ( 'NONE',  ( 0.000000000000000000, -1.000000000000000000, 0.000000000000000000 ) ) ;
#28099 =( GEOMETRIC_REPRESENTATION_CONTEXT ( 3 ) GLOBAL_UNCERTAINTY_ASSIGNED_CONTEXT ( ( #21695 ) ) GLOBAL_UNIT_ASSIGNED_CONTEXT ( ( #7587, #3638, #32798 ) ) REPRESENTATION_CONTEXT ( 'NONE', 'WORKASPACE' ) );
#28100 = CARTESIAN_POINT ( 'NONE',  ( 20.65191334053707095, -175.3837268820161057, 102.9412430821799802 ) ) ;
#28101 = CARTESIAN_POINT ( 'NONE',  ( -48.47912675150885065, -177.1207230881787780, 6.938893903907228378E-15 ) ) ;
#28102 = AXIS2_PLACEMENT_3D ( 'NONE', #36922, #32458, #24831 ) ;
#28103 = ORIENTED_EDGE ( 'NONE', *, *, #7353, .F. ) ;
#28104 = VECTOR ( 'NONE', #23871, 999.9999999999998863 ) ;
#28105 = CARTESIAN_POINT ( 'NONE',  ( -332.3517673607765914, -123.5000000000000284, 0.000000000000000000 ) ) ;
#28106 = ORIENTED_EDGE ( 'NONE', *, *, #25943, .F. ) ;
#28107 = VERTEX_POINT ( 'NONE', #255 ) ;
#28108 = VECTOR ( 'NONE', #38349, 1000.000000000000000 ) ;
#28109 = ORIENTED_EDGE ( 'NONE', *, *, #28713, .F. ) ;
#28110 = ORIENTED_EDGE ( 'NONE', *, *, #46492, .T. ) ;
#28111 = DIRECTION ( 'NONE',  ( -0.7378332790417189146, 0.000000000000000000, -0.6749830015182196608 ) ) ;
#28112 = EDGE_CURVE ( 'NONE', #13761, #38315, #17033, .T. ) ;
#28113 = EDGE_CURVE ( 'NONE', #41296, #35254, #31813, .T. ) ;
#28114 = VERTEX_POINT ( 'NONE', #27849 ) ;
#28115 = DIRECTION ( 'NONE',  ( -0.3202698538628487301, 0.000000000000000000, 0.9473263538541877304 ) ) ;
#28116 = FACE_OUTER_BOUND ( 'NONE', #9465, .T. ) ;
#28119 = VERTEX_POINT ( 'NONE', #7880 ) ;
#28118 = CARTESIAN_POINT ( 'NONE',  ( -25.00456841203573077, 45.00000000000000000, 3.062176466986057355E-15 ) ) ;
#28117 = CARTESIAN_POINT ( 'NONE',  ( -48.47912675150885065, -120.5000000000000284, 6.938893903907228378E-15 ) ) ;
#28120 = VECTOR ( 'NONE', #31010, 1000.000000000000114 ) ;
#28121 = CARTESIAN_POINT ( 'NONE',  ( -49.25565061422688728, -177.1207230881787780, -0.6300878435817132139 ) ) ;
#28122 = VECTOR ( 'NONE', #46855, 1000.000000000000000 ) ;
#28123 = ORIENTED_EDGE ( 'NONE', *, *, #36259, .F. ) ;
#28124 = DIRECTION ( 'NONE',  ( 0.000000000000000000, -0.4647231720437604574, 0.8854560256532141294 ) ) ;
#28125 = ORIENTED_EDGE ( 'NONE', *, *, #27299, .T. ) ;
#28126 = VECTOR ( 'NONE', #39469, 1000.000000000000000 ) ;
#28127 = CARTESIAN_POINT ( 'NONE',  ( -49.25565061422688728, -189.7472609257535510, -0.6300878435817132139 ) ) ;
#28128 = EDGE_CURVE ( 'NONE', #30637, #48961, #39169, .T. ) ;
#28129 = DIRECTION ( 'NONE',  ( -0.000000000000000000, 0.2393156642875685636, 0.9709418174260492362 ) ) ;
#28131 = CARTESIAN_POINT ( 'NONE',  ( 64.46023522152408702, -193.5000000000000000, -51.19472891551279048 ) ) ;
#28130 = DIRECTION ( 'NONE',  ( 1.000000000000000000, -0.000000000000000000, 0.000000000000000000 ) ) ;
#28132 = VECTOR ( 'NONE', #27193, 1000.000000000000000 ) ;
#28133 = VERTEX_POINT ( 'NONE', #36254 ) ;
#28134 = EDGE_CURVE ( 'NONE', #12983, #28415, #1066, .T. ) ;
#28135 = DIRECTION ( 'NONE',  ( 0.000000000000000000, 0.000000000000000000, -1.000000000000000000 ) ) ;
#28136 = DIRECTION ( 'NONE',  ( 0.000000000000000000, 1.000000000000000000, 0.000000000000000000 ) ) ;
#28137 = EDGE_CURVE ( 'NONE', #25732, #26284, #15332, .T. ) ;
#28138 = DIRECTION ( 'NONE',  ( 0.000000000000000000, -1.000000000000000000, -0.000000000000000000 ) ) ;
#28139 = ORIENTED_EDGE ( 'NONE', *, *, #37297, .F. ) ;
#28140 = VECTOR ( 'NONE', #50145, 1000.000000000000000 ) ;
#28141 = LINE ( 'NONE', #8441, #21615 ) ;
#28142 = DIRECTION ( 'NONE',  ( 0.000000000000000000, 0.000000000000000000, -1.000000000000000000 ) ) ;
#28143 = VECTOR ( 'NONE', #14192, 1000.000000000000000 ) ;
#28144 = LINE ( 'NONE', #43673, #6448 ) ;
#28145 = ADVANCED_FACE ( 'NONE', ( #51524 ), #16043, .F. ) ;
#28146 = ORIENTED_EDGE ( 'NONE', *, *, #32946, .F. ) ;
#28147 = DIRECTION ( 'NONE',  ( -1.000000000000000000, 0.000000000000000000, -0.000000000000000000 ) ) ;
#28148 = VECTOR ( 'NONE', #35772, 1000.000000000000000 ) ;
#28149 = DIRECTION ( 'NONE',  ( 0.000000000000000000, 0.000000000000000000, -1.000000000000000000 ) ) ;
#28150 = AXIS2_PLACEMENT_3D ( 'NONE', #43474, #31370, #40023 ) ;
#28151 = VERTEX_POINT ( 'NONE', #48099 ) ;
#28152 = CARTESIAN_POINT ( 'NONE',  ( -48.47912675150885065, -175.3837268820161057, -0.9999999999999931166 ) ) ;
#28153 = VERTEX_POINT ( 'NONE', #31538 ) ;
#28154 = DIRECTION ( 'NONE',  ( 0.9473263538541923934, 0.000000000000000000, -0.3202698538628350744 ) ) ;
#28155 = FACE_OUTER_BOUND ( 'NONE', #27563, .T. ) ;
#28156 = CARTESIAN_POINT ( 'NONE',  ( -332.3517673607765914, -123.5000000000000284, 0.000000000000000000 ) ) ;
#28157 = CARTESIAN_POINT ( 'NONE',  ( -332.3517673607765914, -181.8730728925770563, 8.732051761644092025 ) ) ;
#28158 = DIRECTION ( 'NONE',  ( 0.000000000000000000, 0.000000000000000000, 1.000000000000000000 ) ) ;
#28159 = CARTESIAN_POINT ( 'NONE',  ( -85.14888725715768203, -175.3837268820161057, 119.5003291395398577 ) ) ;
#28160 = VECTOR ( 'NONE', #6602, 1000.000000000000000 ) ;
#28161 = FACE_OUTER_BOUND ( 'NONE', #29944, .T. ) ;
#28162 = LINE ( 'NONE', #20288, #26413 ) ;
#28164 = ORIENTED_EDGE ( 'NONE', *, *, #22703, .T. ) ;
#28163 = CARTESIAN_POINT ( 'NONE',  ( -132.4142998968131053, -193.5000000000000000, -91.27439114664585418 ) ) ;
#28165 = CIRCLE ( 'NONE', #8902, 124.9999999999999858 ) ;
#28166 = AXIS2_PLACEMENT_3D ( 'NONE', #39968, #16084, #11617 ) ;
#28167 = VERTEX_POINT ( 'NONE', #28100 ) ;
#28168 = DIRECTION ( 'NONE',  ( -0.000000000000000000, 1.000000000000000000, -0.000000000000000000 ) ) ;
#28169 = EDGE_CURVE ( 'NONE', #16821, #37730, #47594, .T. ) ;
#28170 = DIRECTION ( 'NONE',  ( -0.3482016354343928088, 0.000000000000000000, -0.9374196611341231167 ) ) ;
#28171 = ORIENTED_EDGE ( 'NONE', *, *, #323, .T. ) ;
#28172 = ORIENTED_EDGE ( 'NONE', *, *, #37810, .T. ) ;
#28173 = AXIS2_PLACEMENT_3D ( 'NONE', #13943, #45744, #9483 ) ;
#28174 = VERTEX_POINT ( 'NONE', #7632 ) ;
#28175 = CARTESIAN_POINT ( 'NONE',  ( 0.000000000000000000, -180.7855672281372108, -14.11962419296555105 ) ) ;
#28176 = VECTOR ( 'NONE', #645, 1000.000000000000227 ) ;
#28177 = EDGE_CURVE ( 'NONE', #21402, #2898, #40202, .T. ) ;
#28178 = ADVANCED_FACE ( 'NONE', ( #28371 ), #23156, .T. ) ;
#28179 = EDGE_CURVE ( 'NONE', #9404, #14211, #38843, .T. ) ;
#28180 = DIRECTION ( 'NONE',  ( 0.000000000000000000, 0.000000000000000000, 1.000000000000000000 ) ) ;
#28181 = CARTESIAN_POINT ( 'NONE',  ( -48.47912675150885065, -175.3837268820161057, 6.938893903907228378E-15 ) ) ;
#28182 = ORIENTED_EDGE ( 'NONE', *, *, #49485, .F. ) ;
#28183 = VERTEX_POINT ( 'NONE', #1033 ) ;
#28184 = EDGE_CURVE ( 'NONE', #8692, #27526, #40709, .T. ) ;
#28185 = ORIENTED_EDGE ( 'NONE', *, *, #34387, .T. ) ;
#28186 = VECTOR ( 'NONE', #15134, 1000.000000000000000 ) ;
#28187 = DIRECTION ( 'NONE',  ( 0.000000000000000000, 0.000000000000000000, -1.000000000000000000 ) ) ;
#28188 = CARTESIAN_POINT ( 'NONE',  ( -48.41988612361515010, -193.5000000000000000, 0.9982437317643287900 ) ) ;
#28189 = PLANE ( 'NONE',  #51804 ) ;
#28190 = ADVANCED_FACE ( 'NONE', ( #12865 ), #28884, .T. ) ;
#28191 = DIRECTION ( 'NONE',  ( 0.9982437317643217956, 0.000000000000000000, -0.05924062789370748011 ) ) ;
#28192 = DIRECTION ( 'NONE',  ( 0.000000000000000000, 0.000000000000000000, 1.000000000000000000 ) ) ;
#28193 = ORIENTED_EDGE ( 'NONE', *, *, #47218, .F. ) ;
#28194 = CYLINDRICAL_SURFACE ( 'NONE', #29719, 125.0000000000000000 ) ;
#28195 = DIRECTION ( 'NONE',  ( -0.000000000000000000, -0.6631226582407885317, 0.7485107481711069655 ) ) ;
#28196 = ADVANCED_FACE ( 'NONE', ( #5260 ), #8410, .F. ) ;
#28197 = DIRECTION ( 'NONE',  ( 1.000000000000000000, -0.000000000000000000, -0.000000000000000000 ) ) ;
#28198 = LINE ( 'NONE', #3777, #12286 ) ;
#28199 = ADVANCED_FACE ( 'NONE', ( #25476 ), #1297, .T. ) ;
#28200 = ORIENTED_EDGE ( 'NONE', *, *, #27691, .F. ) ;
#28201 = ORIENTED_EDGE ( 'NONE', *, *, #3807, .T. ) ;
#28202 = VERTEX_POINT ( 'NONE', #17610 ) ;
#28203 = LINE ( 'NONE', #43985, #16418 ) ;
#28204 = AXIS2_PLACEMENT_3D ( 'NONE', #8003, #48489, #28479 ) ;
#28205 = ADVANCED_FACE ( 'NONE', ( #5003 ), #33621, .F. ) ;
#28206 = FACE_OUTER_BOUND ( 'NONE', #39337, .T. ) ;
#28207 = ORIENTED_EDGE ( 'NONE', *, *, #42635, .F. ) ;
#28208 = LINE ( 'NONE', #48202, #40822 ) ;
#28209 = AXIS2_PLACEMENT_3D ( 'NONE', #21774, #18602, #46723 ) ;
#28210 = AXIS2_PLACEMENT_3D ( 'NONE', #51002, #46285, #14731 ) ;
#28211 = EDGE_CURVE ( 'NONE', #44616, #6723, #37036, .T. ) ;
#28212 = FACE_OUTER_BOUND ( 'NONE', #29115, .T. ) ;
#28213 = ORIENTED_EDGE ( 'NONE', *, *, #17974, .F. ) ;
#28214 = DIRECTION ( 'NONE',  ( 1.000000000000000000, 8.718379230999705894E-17, -3.044005838999302267E-31 ) ) ;
#28215 = EDGE_CURVE ( 'NONE', #42588, #38711, #41492, .T. ) ;
#28216 = ORIENTED_EDGE ( 'NONE', *, *, #29877, .T. ) ;
#28217 = CARTESIAN_POINT ( 'NONE',  ( 65.12862465015753344, -183.6283474603465606, 49.69312418816388544 ) ) ;
#28218 = ORIENTED_EDGE ( 'NONE', *, *, #5028, .T. ) ;
#28219 = PLANE ( 'NONE',  #12006 ) ;
#28220 = AXIS2_PLACEMENT_3D ( 'NONE', #34797, #14864, #47419 ) ;
#28221 = AXIS2_PLACEMENT_3D ( 'NONE', #17486, #25102, #33502 ) ;
#28222 = CARTESIAN_POINT ( 'NONE',  ( -104.8182102393454045, -175.3837268820161057, 111.5836353223472770 ) ) ;
#28223 = ORIENTED_EDGE ( 'NONE', *, *, #16336, .T. ) ;
#28224 = VECTOR ( 'NONE', #34631, 1000.000000000000114 ) ;
#28225 = AXIS2_PLACEMENT_3D ( 'NONE', #21380, #40296, #32689 ) ;
#28226 = DIRECTION ( 'NONE',  ( -0.000000000000000000, -1.000000000000000000, -0.000000000000000000 ) ) ;
#28227 = PLANE ( 'NONE',  #15479 ) ;
#28228 = DIRECTION ( 'NONE',  ( 1.000000000000000000, 0.000000000000000000, 0.000000000000000000 ) ) ;
#28229 = VECTOR ( 'NONE', #45494, 1000.000000000000114 ) ;
#28230 = DIRECTION ( 'NONE',  ( 0.9890401873221644768, 0.000000000000000000, -0.1476465640024779702 ) ) ;
#28231 = EDGE_CURVE ( 'NONE', #41178, #50666, #9201, .T. ) ;
#28232 = ORIENTED_EDGE ( 'NONE', *, *, #27765, .F. ) ;
#28234 = VECTOR ( 'NONE', #1121, 1000.000000000000000 ) ;
#28233 = CARTESIAN_POINT ( 'NONE',  ( -339.1964088526558498, -182.1300919119129560, -6.615309698014600670 ) ) ;
#28235 = EDGE_LOOP ( 'NONE', ( #9220, #21698, #19550, #44321 ) ) ;
#28236 = AXIS2_PLACEMENT_3D ( 'NONE', #29687, #9470, #1588 ) ;
#28237 = DIRECTION ( 'NONE',  ( -0.000000000000000000, 1.000000000000000000, -0.000000000000000000 ) ) ;
#28239 = VERTEX_POINT ( 'NONE', #40451 ) ;
#28238 = DIRECTION ( 'NONE',  ( 0.000000000000000000, -0.9927088740980530845, 0.1205366802553303196 ) ) ;
#28240 = ORIENTED_EDGE ( 'NONE', *, *, #21660, .T. ) ;
#28241 = DIRECTION ( 'NONE',  ( 0.000000000000000000, -0.000000000000000000, -1.000000000000000000 ) ) ;
#28242 = CARTESIAN_POINT ( 'NONE',  ( -48.47912675150885065, -189.7472609257535510, 6.938893903907228378E-15 ) ) ;
#28243 = AXIS2_PLACEMENT_3D ( 'NONE', #41679, #5705, #38249 ) ;
#28244 = VECTOR ( 'NONE', #1938, 1000.000000000000000 ) ;
#28245 = EDGE_LOOP ( 'NONE', ( #8145, #33379, #25426, #51128 ) ) ;
#28246 = CARTESIAN_POINT ( 'NONE',  ( -339.1964088526558498, -96.52406086224443982, -52.47426709956138069 ) ) ;
#28247 = DIRECTION ( 'NONE',  ( 0.000000000000000000, 1.882753212593494549E-13, -1.000000000000000000 ) ) ;
#28248 = VERTEX_POINT ( 'NONE', #49144 ) ;
#28249 = DIRECTION ( 'NONE',  ( -0.7378332790417189146, 0.000000000000000000, -0.6749830015182196608 ) ) ;
#28250 = DIRECTION ( 'NONE',  ( 0.000000000000000000, 1.156482317317871232E-16, 1.000000000000000000 ) ) ;
#28251 = CIRCLE ( 'NONE', #40813, 60.00000000000000000 ) ;
#28252 = EDGE_CURVE ( 'NONE', #49023, #32161, #27920, .T. ) ;
#28253 = ADVANCED_FACE ( 'NONE', ( #5524 ), #29154, .T. ) ;
#28254 = DIRECTION ( 'NONE',  ( -0.000000000000000000, 1.000000000000000000, 0.000000000000000000 ) ) ;
#28255 = DIRECTION ( 'NONE',  ( 0.9890401873221644768, 0.000000000000000000, -0.1476465640024779702 ) ) ;
#28256 = ORIENTED_EDGE ( 'NONE', *, *, #45533, .T. ) ;
#28257 = VERTEX_POINT ( 'NONE', #33370 ) ;
#28258 = EDGE_CURVE ( 'NONE', #21618, #24982, #785, .T. ) ;
#28259 = ORIENTED_EDGE ( 'NONE', *, *, #40082, .T. ) ;
#28260 = EDGE_CURVE ( 'NONE', #52027, #31544, #45538, .T. ) ;
#28261 = DIRECTION ( 'NONE',  ( 0.000000000000000000, -1.000000000000000000, 0.000000000000000000 ) ) ;
#28262 = DIRECTION ( 'NONE',  ( -0.6965510290629932655, 0.000000000000000000, -0.7175072570443347120 ) ) ;
#28263 = VECTOR ( 'NONE', #7430, 1000.000000000000114 ) ;
#28264 = CIRCLE ( 'NONE', #41698, 125.0000000000000000 ) ;
#28265 = DIRECTION ( 'NONE',  ( 0.000000000000000000, 0.000000000000000000, 1.000000000000000000 ) ) ;
#28266 = AXIS2_PLACEMENT_3D ( 'NONE', #47621, #14524, #6886 ) ;
#28268 = VECTOR ( 'NONE', #1929, 1000.000000000000000 ) ;
#28267 = FACE_BOUND ( 'NONE', #33195, .T. ) ;
#28269 = CARTESIAN_POINT ( 'NONE',  ( -330.4913330509368166, -176.3931552210903249, -28.32515014536811293 ) ) ;
#28270 = ORIENTED_EDGE ( 'NONE', *, *, #25722, .T. ) ;
#28271 = AXIS2_PLACEMENT_3D ( 'NONE', #42565, #14715, #14986 ) ;
#28272 = ORIENTED_EDGE ( 'NONE', *, *, #34965, .T. ) ;
#28274 = ORIENTED_EDGE ( 'NONE', *, *, #50094, .F. ) ;
#28273 = CARTESIAN_POINT ( 'NONE',  ( -339.1964088526558498, -175.9742670995615015, -26.97593913775538965 ) ) ;
#28275 = EDGE_LOOP ( 'NONE', ( #35681, #15704, #47154, #31130 ) ) ;
#28276 = EDGE_CURVE ( 'NONE', #43984, #43356, #49659, .T. ) ;
#28277 = DIRECTION ( 'NONE',  ( 0.000000000000000000, 0.000000000000000000, 1.000000000000000000 ) ) ;
#28278 = DIRECTION ( 'NONE',  ( -0.000000000000000000, -0.000000000000000000, 1.000000000000000000 ) ) ;
#28279 = CARTESIAN_POINT ( 'NONE',  ( -167.1580984288391107, -189.7472609257535510, -39.24667733211878584 ) ) ;
#28280 = PLANE ( 'NONE',  #14191 ) ;
#28281 = ORIENTED_EDGE ( 'NONE', *, *, #50367, .F. ) ;
#28282 = CARTESIAN_POINT ( 'NONE',  ( -11.80936624585915418, -189.7472609257535510, -119.5003291395395877 ) ) ;
#28283 = ORIENTED_EDGE ( 'NONE', *, *, #5967, .T. ) ;
#28284 = EDGE_CURVE ( 'NONE', #29227, #41086, #13396, .T. ) ;
#28285 = VERTEX_POINT ( 'NONE', #36792 ) ;
#28286 = CARTESIAN_POINT ( 'NONE',  ( -147.0463339291295881, -177.1207230881787780, 76.87330921200150158 ) ) ;
#28287 = VECTOR ( 'NONE', #28648, 1000.000000000000000 ) ;
#28288 = VECTOR ( 'NONE', #30500, 1000.000000000000227 ) ;
#28289 = DIRECTION ( 'NONE',  ( 0.000000000000000000, -2.659909329831104317E-14, -1.000000000000000000 ) ) ;
#28290 = DIRECTION ( 'NONE',  ( -0.8124868780056863082, 0.000000000000000000, 0.5829794791144649047 ) ) ;
#28291 = VECTOR ( 'NONE', #24251, 1000.000000000000000 ) ;
#28292 = DIRECTION ( 'NONE',  ( 0.000000000000000000, -1.000000000000000000, 0.000000000000000000 ) ) ;
#28293 = PLANE ( 'NONE',  #26211 ) ;
#28294 = VERTEX_POINT ( 'NONE', #16832 ) ;
#28295 = LINE ( 'NONE', #16221, #8714 ) ;
#28296 = LINE ( 'NONE', #47771, #37442 ) ;
#28297 = FACE_BOUND ( 'NONE', #18008, .T. ) ;
#28298 = ORIENTED_EDGE ( 'NONE', *, *, #16616, .T. ) ;
#28299 = CIRCLE ( 'NONE', #40902, 60.00000000000000000 ) ;
#28300 = AXIS2_PLACEMENT_3D ( 'NONE', #35756, #11595, #27866 ) ;
#28301 = DIRECTION ( 'NONE',  ( -0.000000000000000000, 1.000000000000000000, -0.000000000000000000 ) ) ;
#28302 = AXIS2_PLACEMENT_3D ( 'NONE', #44329, #17239, #40878 ) ;
#28303 = DIRECTION ( 'NONE',  ( 0.000000000000000000, 0.5680647467311540355, -0.8229838658936575735 ) ) ;
#28304 = ORIENTED_EDGE ( 'NONE', *, *, #27279, .T. ) ;
#28305 = DIRECTION ( 'NONE',  ( 0.8124868780056825335, 0.000000000000000000, -0.5829794791144703447 ) ) ;
#28306 = EDGE_CURVE ( 'NONE', #17420, #36143, #25422, .T. ) ;
#28307 = AXIS2_PLACEMENT_3D ( 'NONE', #28694, #40263, #8734 ) ;
#28308 = ORIENTED_EDGE ( 'NONE', *, *, #33557, .T. ) ;
#28309 = VECTOR ( 'NONE', #2152, 1000.000000000000000 ) ;
#28310 = CARTESIAN_POINT ( 'NONE',  ( -26.37732090265850005, -175.3837268820161057, -122.0143860769387061 ) ) ;
#28311 = CARTESIAN_POINT ( 'NONE',  ( -339.1964088526558498, -123.5000000000000284, 0.000000000000000000 ) ) ;
#28312 = CARTESIAN_POINT ( 'NONE',  ( -339.1964088526558498, -162.9984922102927385, -43.83057281297435992 ) ) ;
#28313 = EDGE_CURVE ( 'NONE', #37656, #41503, #44542, .T. ) ;
#28314 = EDGE_CURVE ( 'NONE', #1525, #10115, #4596, .T. ) ;
#28315 = DIRECTION ( 'NONE',  ( 0.000000000000000000, 0.000000000000000000, 1.000000000000000000 ) ) ;
#28316 = ORIENTED_EDGE ( 'NONE', *, *, #51366, .F. ) ;
#28317 = EDGE_LOOP ( 'NONE', ( #4629, #18038, #49822, #45226 ) ) ;
#28318 = CARTESIAN_POINT ( 'NONE',  ( 44.19966546217225556, 28.88712326890130555, -43.13141586961224050 ) ) ;
#28319 = CIRCLE ( 'NONE', #16608, 125.0000000000000000 ) ;
#28320 = ORIENTED_EDGE ( 'NONE', *, *, #51375, .F. ) ;
#28321 = CARTESIAN_POINT ( 'NONE',  ( 51.05451324771860300, -193.5000000000000000, 75.61781872352698031 ) ) ;
#28322 = CARTESIAN_POINT ( 'NONE',  ( -126.2322430781613889, -177.1207230881787780, 97.87467957288052389 ) ) ;
#28323 = AXIS2_PLACEMENT_3D ( 'NONE', #19854, #51938, #36925 ) ;
#28324 = CARTESIAN_POINT ( 'NONE',  ( -48.47912675150885065, -177.1207230881787780, 6.938893903907228378E-15 ) ) ;
#28325 = DIRECTION ( 'NONE',  ( -0.000000000000000000, 1.000000000000000000, -0.000000000000000000 ) ) ;
#28326 = ORIENTED_EDGE ( 'NONE', *, *, #8789, .F. ) ;
#28329 = ORIENTED_EDGE ( 'NONE', *, *, #9915, .T. ) ;
#28328 = PLANE ( 'NONE',  #14697 ) ;
#28327 = DIRECTION ( 'NONE',  ( -0.6965510290629882695, 0.000000000000000000, -0.7175072570443395970 ) ) ;
#28330 = AXIS2_PLACEMENT_3D ( 'NONE', #11438, #16443, #40322 ) ;
#28331 = ORIENTED_EDGE ( 'NONE', *, *, #44833, .T. ) ;
#28332 = EDGE_CURVE ( 'NONE', #6252, #5943, #5129, .T. ) ;
#28333 = VECTOR ( 'NONE', #22488, 1000.000000000000114 ) ;
#28334 = CARTESIAN_POINT ( 'NONE',  ( -47.82630463331832971, -189.7472609257535510, -0.7575112421616121416 ) ) ;
#28335 = EDGE_LOOP ( 'NONE', ( #18323, #18541, #24464, #34934 ) ) ;
#28336 = DIRECTION ( 'NONE',  ( -0.2635871660690648488, 0.000000000000000000, -0.9646355819083595184 ) ) ;
#28337 = ORIENTED_EDGE ( 'NONE', *, *, #28792, .F. ) ;
#28338 = DIRECTION ( 'NONE',  ( 0.4031234292879792847, 0.000000000000000000, -0.9151456172430153524 ) ) ;
#28339 = ORIENTED_EDGE ( 'NONE', *, *, #18626, .T. ) ;
#28341 = DIRECTION ( 'NONE',  ( -1.000000000000000000, 0.000000000000000000, 0.000000000000000000 ) ) ;
#28340 = FACE_OUTER_BOUND ( 'NONE', #10258, .T. ) ;
#28342 = ORIENTED_EDGE ( 'NONE', *, *, #51775, .T. ) ;
#28343 = ADVANCED_FACE ( 'NONE', ( #30069 ), #50054, .F. ) ;
#28344 = AXIS2_PLACEMENT_3D ( 'NONE', #37326, #1062, #44704 ) ;
#28345 = ORIENTED_EDGE ( 'NONE', *, *, #18769, .T. ) ;
#28346 = DIRECTION ( 'NONE',  ( -0.9995608365087944591, 0.000000000000000000, 0.02963332782255633305 ) ) ;
#28347 = CARTESIAN_POINT ( 'NONE',  ( 68.93474881819257405, -189.7472609257535510, 39.87457906003773900 ) ) ;
#28348 = FACE_OUTER_BOUND ( 'NONE', #49062, .T. ) ;
#28349 = DIRECTION ( 'NONE',  ( 0.000000000000000000, -0.000000000000000000, -1.000000000000000000 ) ) ;
#28350 = CARTESIAN_POINT ( 'NONE',  ( -124.9871112439422092, -175.3837268820161057, -98.85104101073277150 ) ) ;
#28351 = CARTESIAN_POINT ( 'NONE',  ( 65.38692482895591240, -183.6283474603465606, -51.57055649762701677 ) ) ;
#28352 = ORIENTED_EDGE ( 'NONE', *, *, #51349, .T. ) ;
#28353 =( LENGTH_UNIT ( ) NAMED_UNIT ( * ) SI_UNIT ( .MILLI., .METRE. ) );
#28354 = EDGE_CURVE ( 'NONE', #51222, #29810, #42212, .T. ) ;
#28355 = DIRECTION ( 'NONE',  ( 0.6068001458185890984, 0.000000000000000000, 0.7948544414133565938 ) ) ;
#28356 = CARTESIAN_POINT ( 'NONE',  ( -171.4462109067799247, -177.1207230881787780, 15.97798378892250426 ) ) ;
#28357 = DIRECTION ( 'NONE',  ( -0.000000000000000000, 0.5680647467311656929, 0.8229838658936495799 ) ) ;
#28358 = ORIENTED_EDGE ( 'NONE', *, *, #16231, .T. ) ;
#28359 = VECTOR ( 'NONE', #41078, 1000.000000000000114 ) ;
#28360 = DIRECTION ( 'NONE',  ( -0.8757349421956412971, 0.000000000000000000, 0.4827922027307366970 ) ) ;
#28361 = AXIS2_PLACEMENT_3D ( 'NONE', #47143, #3259, #2984 ) ;
#28362 = DIRECTION ( 'NONE',  ( 0.000000000000000000, 0.000000000000000000, 1.000000000000000000 ) ) ;
#28363 = DIRECTION ( 'NONE',  ( -0.000000000000000000, 1.000000000000000000, -0.000000000000000000 ) ) ;
#28364 = ORIENTED_EDGE ( 'NONE', *, *, #39701, .F. ) ;
#28365 = ORIENTED_EDGE ( 'NONE', *, *, #34270, .F. ) ;
#28366 = ORIENTED_EDGE ( 'NONE', *, *, #19145, .T. ) ;
#28367 = EDGE_CURVE ( 'NONE', #50110, #26396, #29543, .T. ) ;
#28368 = VECTOR ( 'NONE', #39495, 1000.000000000000000 ) ;
#28369 = DIRECTION ( 'NONE',  ( -0.000000000000000000, 0.4647231720437573488, -0.8854560256532157947 ) ) ;
#28370 = DIRECTION ( 'NONE',  ( -0.000000000000000000, 1.000000000000000000, -0.000000000000000000 ) ) ;
#28371 = FACE_OUTER_BOUND ( 'NONE', #28317, .T. ) ;
#28372 = DIRECTION ( 'NONE',  ( 0.000000000000000000, 0.000000000000000000, -1.000000000000000000 ) ) ;
#28373 = ORIENTED_EDGE ( 'NONE', *, *, #21961, .F. ) ;
#28374 = EDGE_CURVE ( 'NONE', #8829, #18239, #21144, .T. ) ;
#28375 = EDGE_CURVE ( 'NONE', #45414, #7213, #41116, .T. ) ;
#28376 = PLANE ( 'NONE',  #41942 ) ;
#28377 = ORIENTED_EDGE ( 'NONE', *, *, #25597, .T. ) ;
#28378 = AXIS2_PLACEMENT_3D ( 'NONE', #4970, #474, #32549 ) ;
#28379 = ORIENTED_EDGE ( 'NONE', *, *, #3102, .F. ) ;
#28380 = EDGE_CURVE ( 'NONE', #15465, #50694, #33505, .T. ) ;
#28381 = ORIENTED_EDGE ( 'NONE', *, *, #19825, .F. ) ;
#28382 = DIRECTION ( 'NONE',  ( 0.7575112421616236880, 0.000000000000000000, -0.6528221181905174975 ) ) ;
#28383 = CARTESIAN_POINT ( 'NONE',  ( -53.47502265695602119, -193.5000000000000000, -124.9001241957025883 ) ) ;
#28384 = DIRECTION ( 'NONE',  ( 0.6965510290629882695, 0.000000000000000000, 0.7175072570443395970 ) ) ;
#28387 = EDGE_LOOP ( 'NONE', ( #23958, #8034, #12374, #19251 ) ) ;
#28386 = LINE ( 'NONE', #8424, #4005 ) ;
#28385 = PLANE ( 'NONE',  #24986 ) ;
#28388 = CIRCLE ( 'NONE', #12453, 125.0000000000000000 ) ;
#28389 = CIRCLE ( 'NONE', #37641, 125.0000000000000000 ) ;
#28390 = ADVANCED_FACE ( 'NONE', ( #14050, #33228 ), #49543, .T. ) ;
#28391 = CARTESIAN_POINT ( 'NONE',  ( -330.4913330509368166, -137.3729703655840524, -58.37414404713467064 ) ) ;
#28392 = ORIENTED_EDGE ( 'NONE', *, *, #2575, .T. ) ;
#28393 = CARTESIAN_POINT ( 'NONE',  ( -162.3451783319732442, -183.6283474603465606, 51.57055649762783389 ) ) ;
#28395 = VECTOR ( 'NONE', #40210, 1000.000000000000000 ) ;
#28394 = CARTESIAN_POINT ( 'NONE',  ( -339.1964088526558498, -108.8949048983204051, 57.16590939599314680 ) ) ;
#28396 = ORIENTED_EDGE ( 'NONE', *, *, #46811, .F. ) ;
#28397 = DIRECTION ( 'NONE',  ( 0.2920567706369833760, 0.000000000000000000, -0.9564009842765202052 ) ) ;
#28398 = PLANE ( 'NONE',  #4887 ) ;
#28400 = CARTESIAN_POINT ( 'NONE',  ( -48.47912675150885065, -175.3837268820161057, 6.938893903907228378E-15 ) ) ;
#28399 = CARTESIAN_POINT ( 'NONE',  ( 3.652658254809377336, -177.1207230881787780, -112.5098962032389522 ) ) ;
#28401 = VERTEX_POINT ( 'NONE', #9329 ) ;
#28402 = CIRCLE ( 'NONE', #38512, 125.0000000000000000 ) ;
#28403 = CARTESIAN_POINT ( 'NONE',  ( -305.0000000000000568, -63.55776901541228341, -2.632288850093980503 ) ) ;
#28404 = DIRECTION ( 'NONE',  ( 1.000000000000000000, -0.000000000000000000, -0.000000000000000000 ) ) ;
#28405 =( NAMED_UNIT ( * ) SI_UNIT ( $, .STERADIAN. ) SOLID_ANGLE_UNIT ( ) );
#28406 = ORIENTED_EDGE ( 'NONE', *, *, #8005, .T. ) ;
#28407 = CARTESIAN_POINT ( 'NONE',  ( -336.3521761649654422, -106.8245764869328980, 56.65561927337994064 ) ) ;
#28408 = CARTESIAN_POINT ( 'NONE',  ( -48.36085358058748795, -183.6283474603465606, 0.9929810960135245779 ) ) ;
#28409 = ORIENTED_EDGE ( 'NONE', *, *, #29494, .T. ) ;
#28410 = CARTESIAN_POINT ( 'NONE',  ( -48.47912675150885065, -177.1207230881787780, 6.938893903907228378E-15 ) ) ;
#28411 = DIRECTION ( 'NONE',  ( -0.9960498426152171181, 0.000000000000000000, 0.08879589532293157006 ) ) ;
#28412 = VECTOR ( 'NONE', #23326, 1000.000000000000000 ) ;
#28413 = ORIENTED_EDGE ( 'NONE', *, *, #48297, .T. ) ;
#28414 = DIRECTION ( 'NONE',  ( 0.000000000000000000, 1.000000000000000000, -0.000000000000000000 ) ) ;
#28415 = VERTEX_POINT ( 'NONE', #33750 ) ;
#28416 = DIRECTION ( 'NONE',  ( 0.000000000000000000, 0.000000000000000000, 1.000000000000000000 ) ) ;
#28417 = CARTESIAN_POINT ( 'NONE',  ( 67.04262753014327814, -189.7472609257535510, -47.74645837849745078 ) ) ;
#28418 = CARTESIAN_POINT ( 'NONE',  ( -51.89154260666836649, -193.5000000000000000, 124.9534129907280828 ) ) ;
#28419 = ADVANCED_FACE ( 'NONE', ( #49275 ), #13268, .T. ) ;
#28420 = DIRECTION ( 'NONE',  ( 0.000000000000000000, 0.000000000000000000, -1.000000000000000000 ) ) ;
#28421 = LINE ( 'NONE', #4790, #14885 ) ;
#28422 = CARTESIAN_POINT ( 'NONE',  ( -48.53836737940257251, -177.1207230881787780, 0.9982437317643279018 ) ) ;
#28423 = AXIS2_PLACEMENT_3D ( 'NONE', #36560, #28147, #4251 ) ;
#28424 = CIRCLE ( 'NONE', #41876, 125.0000000000000000 ) ;
#28425 = DIRECTION ( 'NONE',  ( 1.000000000000000000, -0.000000000000000000, -0.000000000000000000 ) ) ;
#28426 = DIRECTION ( 'NONE',  ( -0.000000000000000000, 1.000000000000000000, -0.000000000000000000 ) ) ;
#28428 = ORIENTED_EDGE ( 'NONE', *, *, #29400, .T. ) ;
#28427 = LINE ( 'NONE', #12132, #7725 ) ;
#28429 = VECTOR ( 'NONE', #10997, 1000.000000000000000 ) ;
#28430 = EDGE_LOOP ( 'NONE', ( #51698, #50410, #7452, #11319 ) ) ;
#28431 = DIRECTION ( 'NONE',  ( 0.000000000000000000, 0.000000000000000000, -1.000000000000000000 ) ) ;
#28432 = ADVANCED_FACE ( 'NONE', ( #9842 ), #29015, .F. ) ;
#28433 = EDGE_CURVE ( 'NONE', #471, #7989, #5655, .T. ) ;
#28434 = DIRECTION ( 'NONE',  ( 0.7948544414133565938, 0.000000000000000000, -0.6068001458185890984 ) ) ;
#28435 = ORIENTED_EDGE ( 'NONE', *, *, #47505, .F. ) ;
#28436 = AXIS2_PLACEMENT_3D ( 'NONE', #45655, #9642, #6491 ) ;
#28437 = EDGE_LOOP ( 'NONE', ( #29503, #6241, #15675, #22391 ) ) ;
#28438 = ADVANCED_FACE ( 'NONE', ( #25350 ), #41369, .F. ) ;
#28439 = ORIENTED_EDGE ( 'NONE', *, *, #41074, .F. ) ;
#28440 = FACE_OUTER_BOUND ( 'NONE', #35556, .T. ) ;
#28441 = CARTESIAN_POINT ( 'NONE',  ( -48.47912675150885065, -189.7472609257535510, 6.938893903907228378E-15 ) ) ;
#28442 = CARTESIAN_POINT ( 'NONE',  ( -339.1964088526558498, -89.82879061784706209, -49.66134974749692788 ) ) ;
#28443 = ORIENTED_EDGE ( 'NONE', *, *, #22155, .F. ) ;
#28444 = ORIENTED_EDGE ( 'NONE', *, *, #2800, .T. ) ;
#28445 = ORIENTED_EDGE ( 'NONE', *, *, #34552, .F. ) ;
#28446 = VECTOR ( 'NONE', #46531, 1000.000000000000000 ) ;
#28447 = DIRECTION ( 'NONE',  ( 0.000000000000000000, 6.938893903907222461E-16, 1.000000000000000000 ) ) ;
#28448 = FACE_OUTER_BOUND ( 'NONE', #42819, .T. ) ;
#28450 = ORIENTED_EDGE ( 'NONE', *, *, #3196, .F. ) ;
#28449 = CARTESIAN_POINT ( 'NONE',  ( -138.3705904895685705, -193.5000000000000000, -86.85922373029296750 ) ) ;
#28451 = CARTESIAN_POINT ( 'NONE',  ( -339.1964088526558498, -167.9936954712156592, -38.74998146212110584 ) ) ;
#28452 = DIRECTION ( 'NONE',  ( 1.000000000000000000, 0.000000000000000000, 0.000000000000000000 ) ) ;
#28453 = VERTEX_POINT ( 'NONE', #34002 ) ;
#28454 = LINE ( 'NONE', #24004, #338 ) ;
#28455 = DIRECTION ( 'NONE',  ( -0.8455960035018272869, 0.000000000000000000, 0.5338233779647886257 ) ) ;
#28456 = FACE_OUTER_BOUND ( 'NONE', #45015, .T. ) ;
#28457 = DIRECTION ( 'NONE',  ( 0.000000000000000000, 1.000000000000000000, 0.000000000000000000 ) ) ;
#28458 = ORIENTED_EDGE ( 'NONE', *, *, #37226, .F. ) ;
#28459 = ORIENTED_EDGE ( 'NONE', *, *, #20358, .T. ) ;
#28460 = DIRECTION ( 'NONE',  ( 0.000000000000000000, 0.000000000000000000, 1.000000000000000000 ) ) ;
#28462 = AXIS2_PLACEMENT_3D ( 'NONE', #33294, #9909, #25923 ) ;
#28461 = CARTESIAN_POINT ( 'NONE',  ( -47.55243714407702527, -175.3837268820161057, 0.3758275821142491591 ) ) ;
#28463 = ORIENTED_EDGE ( 'NONE', *, *, #5396, .T. ) ;
#28464 = CARTESIAN_POINT ( 'NONE',  ( -16.00000000000000711, 20.00000000000000355, 0.000000000000000000 ) ) ;
#28465 = AXIS2_PLACEMENT_3D ( 'NONE', #41963, #38017, #2549 ) ;
#28466 = DIRECTION ( 'NONE',  ( 1.000000000000000000, -0.000000000000000000, -0.000000000000000000 ) ) ;
#28467 = ORIENTED_EDGE ( 'NONE', *, *, #49685, .T. ) ;
#28468 = DIRECTION ( 'NONE',  ( 0.000000000000000000, 0.000000000000000000, -1.000000000000000000 ) ) ;
#28469 = DIRECTION ( 'NONE',  ( 0.000000000000000000, 0.000000000000000000, 1.000000000000000000 ) ) ;
#28470 = VERTEX_POINT ( 'NONE', #21675 ) ;
#28471 = LINE ( 'NONE', #40556, #34938 ) ;
#28472 = ORIENTED_EDGE ( 'NONE', *, *, #18530, .T. ) ;
#28473 = DIRECTION ( 'NONE',  ( -0.000000000000000000, 1.000000000000000000, -0.000000000000000000 ) ) ;
#28474 = EDGE_LOOP ( 'NONE', ( #25493, #40723, #5993, #31697 ) ) ;
#28475 = EDGE_CURVE ( 'NONE', #51761, #24816, #1433, .T. ) ;
#28476 = CARTESIAN_POINT ( 'NONE',  ( -339.1964088526558498, -95.63860483659122735, -52.00954392751761191 ) ) ;
#28477 = ADVANCED_FACE ( 'NONE', ( #49796 ), #13780, .F. ) ;
#28478 = DIRECTION ( 'NONE',  ( 0.000000000000000000, 0.000000000000000000, 1.000000000000000000 ) ) ;
#28479 = DIRECTION ( 'NONE',  ( 0.000000000000000000, 0.000000000000000000, 1.000000000000000000 ) ) ;
#28480 = ADVANCED_FACE ( 'NONE', ( #5911 ), #37949, .T. ) ;
#28481 = CARTESIAN_POINT ( 'NONE',  ( -148.7414553014637590, -175.3837268820161057, 72.96212019587208886 ) ) ;
#28482 = ADVANCED_FACE ( 'NONE', ( #22450 ), #7456, .F. ) ;
#28483 = VECTOR ( 'NONE', #26184, 1000.000000000000000 ) ;
#28484 = EDGE_LOOP ( 'NONE', ( #871, #6988, #40330, #47464 ) ) ;
#28485 = DIRECTION ( 'NONE',  ( 0.000000000000000000, 0.000000000000000000, -1.000000000000000000 ) ) ;
#28486 = VERTEX_POINT ( 'NONE', #2210 ) ;
#28487 = ORIENTED_EDGE ( 'NONE', *, *, #43998, .F. ) ;
#28488 = EDGE_CURVE ( 'NONE', #33930, #9394, #6928, .T. ) ;
#28489 = CARTESIAN_POINT ( 'NONE',  ( -63.31390705753094039, -189.7472609257535510, 123.1094209424469312 ) ) ;
#28491 = ORIENTED_EDGE ( 'NONE', *, *, #6285, .F. ) ;
#28490 = DIRECTION ( 'NONE',  ( 0.000000000000000000, 1.000000000000000000, 0.000000000000000000 ) ) ;
#28492 = ADVANCED_FACE ( 'NONE', ( #30569 ), #18757, .F. ) ;
#28493 = ORIENTED_EDGE ( 'NONE', *, *, #6409, .F. ) ;
#28494 = CARTESIAN_POINT ( 'NONE',  ( -32.87124591993210743, -175.3837268820161057, 124.0217483183788261 ) ) ;
#28495 = ADVANCED_FACE ( 'NONE', ( #18251 ), #27404, .F. ) ;
#28496 = EDGE_CURVE ( 'NONE', #29784, #49553, #46368, .T. ) ;
#28497 = EDGE_CURVE ( 'NONE', #31354, #24136, #41394, .T. ) ;
#28498 = DIRECTION ( 'NONE',  ( -0.000000000000000000, 0.000000000000000000, 1.000000000000000000 ) ) ;
#28499 = ORIENTED_EDGE ( 'NONE', *, *, #24411, .F. ) ;
#28500 = EDGE_CURVE ( 'NONE', #30377, #8106, #46625, .T. ) ;
#28501 = AXIS2_PLACEMENT_3D ( 'NONE', #37822, #9985, #18383 ) ;
#28502 = CARTESIAN_POINT ( 'NONE',  ( -27.18512803868276251, -189.7472609257535510, -123.1729094355498404 ) ) ;
#28503 = VERTEX_POINT ( 'NONE', #38470 ) ;
#28504 = CARTESIAN_POINT ( 'NONE',  ( -75.48985759771373694, -177.1207230881787780, -122.0467960216648606 ) ) ;
#28505 = DIRECTION ( 'NONE',  ( 0.000000000000000000, 8.349802331035031902E-14, 1.000000000000000000 ) ) ;
#28506 = EDGE_CURVE ( 'NONE', #21379, #32832, #2475, .T. ) ;
#28507 = DIRECTION ( 'NONE',  ( 0.000000000000000000, 0.4647231720437631775, -0.8854560256532126861 ) ) ;
#28508 = CARTESIAN_POINT ( 'NONE',  ( -144.0067397530739299, -177.1207230881787780, -80.61932246194588458 ) ) ;
#28509 = ORIENTED_EDGE ( 'NONE', *, *, #41070, .T. ) ;
#28510 = ORIENTED_EDGE ( 'NONE', *, *, #13722, .T. ) ;
#28511 = EDGE_LOOP ( 'NONE', ( #39494, #50327, #50463, #47465 ) ) ;
#28512 = FACE_OUTER_BOUND ( 'NONE', #16136, .T. ) ;
#28513 = DIRECTION ( 'NONE',  ( 1.000000000000000000, -0.000000000000000000, -0.000000000000000000 ) ) ;
#28514 = CARTESIAN_POINT ( 'NONE',  ( 38.46761263173351608, -175.3837268820161057, 89.80681772907068705 ) ) ;
#28515 = FACE_BOUND ( 'NONE', #5221, .T. ) ;
#28516 = LINE ( 'NONE', #49812, #18011 ) ;
#28517 = ORIENTED_EDGE ( 'NONE', *, *, #42015, .T. ) ;
#28518 = ADVANCED_FACE ( 'NONE', ( #11369 ), #31089, .T. ) ;
#28519 = AXIS2_PLACEMENT_3D ( 'NONE', #23998, #4039, #44494 ) ;
#28520 = VECTOR ( 'NONE', #30838, 1000.000000000000000 ) ;
#28521 = VERTEX_POINT ( 'NONE', #47389 ) ;
#28523 = EDGE_LOOP ( 'NONE', ( #38425, #10, #13209, #43173 ) ) ;
#28522 = CARTESIAN_POINT ( 'NONE',  ( -49.35486169370449971, -177.1207230881787780, 0.4827922027307437469 ) ) ;
#28524 = ORIENTED_EDGE ( 'NONE', *, *, #35478, .F. ) ;
#28525 = CARTESIAN_POINT ( 'NONE',  ( -133.0671220150036049, -183.6283474603465606, -92.03190238880748097 ) ) ;
#28526 = CARTESIAN_POINT ( 'NONE',  ( -149.5539421794694306, -189.7472609257535510, 73.54509967498654532 ) ) ;
#28527 = DIRECTION ( 'NONE',  ( 0.9785564922995046988, 0.000000000000000000, -0.2059786187410953262 ) ) ;
#28528 = CARTESIAN_POINT ( 'NONE',  ( -48.47912675150885065, -175.3837268820161057, 6.938893903907228378E-15 ) ) ;
#28529 = ORIENTED_EDGE ( 'NONE', *, *, #3504, .F. ) ;
#28530 = PLANE ( 'NONE',  #11597 ) ;
#28531 = ORIENTED_EDGE ( 'NONE', *, *, #19369, .T. ) ;
#28532 = EDGE_CURVE ( 'NONE', #29008, #13637, #24586, .T. ) ;
#28533 = ORIENTED_EDGE ( 'NONE', *, *, #11280, .T. ) ;
#28534 = DIRECTION ( 'NONE',  ( 0.000000000000000000, 1.000000000000000000, 0.000000000000000000 ) ) ;
#28535 = VECTOR ( 'NONE', #29290, 1000.000000000000114 ) ;
#28536 = CARTESIAN_POINT ( 'NONE',  ( -339.1964088526558498, -71.49045607248255862, -27.86139516340906397 ) ) ;
#28537 = CARTESIAN_POINT ( 'NONE',  ( -48.47912675150885065, -183.6283474603465606, 6.938893903907228378E-15 ) ) ;
#28538 = DIRECTION ( 'NONE',  ( -0.000000000000000000, 1.000000000000000000, -0.000000000000000000 ) ) ;
#28539 = ADVANCED_FACE ( 'NONE', ( #26886 ), #2977, .T. ) ;
#28540 = ADVANCED_FACE ( 'NONE', ( #42408 ), #14565, .F. ) ;
#28541 = EDGE_CURVE ( 'NONE', #43643, #11866, #29610, .T. ) ;
#28542 = DIRECTION ( 'NONE',  ( -1.000000000000000000, -0.000000000000000000, -0.000000000000000000 ) ) ;
#28543 = DIRECTION ( 'NONE',  ( 0.000000000000000000, -0.000000000000000000, 1.000000000000000000 ) ) ;
#28544 = EDGE_CURVE ( 'NONE', #47197, #32221, #2719, .T. ) ;
#28545 = ORIENTED_EDGE ( 'NONE', *, *, #25254, .F. ) ;
#28546 = DIRECTION ( 'NONE',  ( 0.000000000000000000, -1.000000000000000000, -0.000000000000000000 ) ) ;
#28547 = CARTESIAN_POINT ( 'NONE',  ( -330.4913330509368166, -84.00150778970706256, 43.83057281297416097 ) ) ;
#28548 = EDGE_CURVE ( 'NONE', #4246, #43850, #30845, .T. ) ;
#28549 = CARTESIAN_POINT ( 'NONE',  ( 75.28414827670442833, -193.5000000000000000, -7.666780576874961284 ) ) ;
#28550 = FACE_BOUND ( 'NONE', #16993, .T. ) ;
#28551 = ORIENTED_EDGE ( 'NONE', *, *, #15648, .F. ) ;
#28552 = EDGE_CURVE ( 'NONE', #25351, #11371, #39242, .T. ) ;
#28553 = CARTESIAN_POINT ( 'NONE',  ( -172.2804936848317823, -193.5000000000000000, -7.024906801078567575 ) ) ;
#28554 = VERTEX_POINT ( 'NONE', #31871 ) ;
#28555 = CARTESIAN_POINT ( 'NONE',  ( -260.0000000000000000, -93.50000000000002842, 51.54700538379266561 ) ) ;
#28556 = ORIENTED_EDGE ( 'NONE', *, *, #33535, .F. ) ;
#28557 = PLANE ( 'NONE',  #25446 ) ;
#28558 = EDGE_CURVE ( 'NONE', #39566, #28133, #31609, .T. ) ;
#28559 = VERTEX_POINT ( 'NONE', #3745 ) ;
#28560 = AXIS2_PLACEMENT_3D ( 'NONE', #27864, #47087, #22908 ) ;
#28561 = EDGE_CURVE ( 'NONE', #19688, #38326, #37193, .T. ) ;
#28562 = VECTOR ( 'NONE', #38391, 1000.000000000000000 ) ;
#28563 = DIRECTION ( 'NONE',  ( 0.000000000000000000, 0.000000000000000000, 1.000000000000000000 ) ) ;
#28564 = EDGE_CURVE ( 'NONE', #21974, #17216, #15376, .T. ) ;
#28565 = CARTESIAN_POINT ( 'NONE',  ( -339.1964088526558498, -109.8658467157473666, -57.40522506028092664 ) ) ;
#28567 = ORIENTED_EDGE ( 'NONE', *, *, #41059, .T. ) ;
#28566 = FACE_OUTER_BOUND ( 'NONE', #19738, .T. ) ;
#28568 = EDGE_CURVE ( 'NONE', #6875, #2378, #28773, .T. ) ;
#28569 = CARTESIAN_POINT ( 'NONE',  ( 48.47907891923915713, -175.3837268820161057, 78.89300572996904748 ) ) ;
#28570 = ORIENTED_EDGE ( 'NONE', *, *, #49778, .T. ) ;
#28571 = ADVANCED_FACE ( 'NONE', ( #48431 ), #27921, .T. ) ;
#28572 = ORIENTED_EDGE ( 'NONE', *, *, #9405, .T. ) ;
#28573 = CARTESIAN_POINT ( 'NONE',  ( 9.336583202542589888, -189.7472609257535510, 110.8257356506556306 ) ) ;
#28574 = AXIS2_PLACEMENT_3D ( 'NONE', #21476, #49600, #17282 ) ;
#28575 = ORIENTED_EDGE ( 'NONE', *, *, #14112, .T. ) ;
#28576 = DIRECTION ( 'NONE',  ( -1.000000000000000000, 0.000000000000000000, 0.000000000000000000 ) ) ;
#28577 = CARTESIAN_POINT ( 'NONE',  ( 30.50828161901820224, -177.1207230881787780, 96.88131563365348597 ) ) ;
#28578 = CYLINDRICAL_SURFACE ( 'NONE', #22995, 125.0000000000000000 ) ;
#28579 = EDGE_CURVE ( 'NONE', #20140, #45478, #11643, .T. ) ;
#28580 = DIRECTION ( 'NONE',  ( 1.000000000000000000, -0.000000000000000000, 0.000000000000000000 ) ) ;
#28581 = DIRECTION ( 'NONE',  ( -1.000000000000000000, -0.000000000000000000, 0.000000000000000000 ) ) ;
#28582 = ORIENTED_EDGE ( 'NONE', *, *, #42547, .F. ) ;
#28585 = EDGE_LOOP ( 'NONE', ( #12720, #5653 ) ) ;
#28584 = DIRECTION ( 'NONE',  ( 0.000000000000000000, 0.000000000000000000, -1.000000000000000000 ) ) ;
#28583 = DIRECTION ( 'NONE',  ( -0.000000000000000000, 1.000000000000000000, -0.000000000000000000 ) ) ;
#28586 = EDGE_LOOP ( 'NONE', ( #42538, #47090, #30618, #10906 ) ) ;
#28587 = DIRECTION ( 'NONE',  ( 0.000000000000000000, 1.000000000000000000, -0.000000000000000000 ) ) ;
#28588 = ORIENTED_EDGE ( 'NONE', *, *, #26417, .F. ) ;
#28589 = DIRECTION ( 'NONE',  ( -1.000000000000000000, -0.000000000000000000, -0.000000000000000000 ) ) ;
#28590 = AXIS2_PLACEMENT_3D ( 'NONE', #33431, #33670, #25522 ) ;
#28591 = ORIENTED_EDGE ( 'NONE', *, *, #50402, .T. ) ;
#28592 = CARTESIAN_POINT ( 'NONE',  ( -339.1964088526558498, -137.1341532842523065, 57.40522506028101901 ) ) ;
#28593 = DIRECTION ( 'NONE',  ( 0.8455960035018311727, 0.000000000000000000, -0.5338233779647826305 ) ) ;
#28594 = ORIENTED_EDGE ( 'NONE', *, *, #46249, .T. ) ;
#28596 = CARTESIAN_POINT ( 'NONE',  ( -48.82732838694323618, -177.1207230881787780, -0.9374196611341184537 ) ) ;
#28595 = CARTESIAN_POINT ( 'NONE',  ( -48.07600332222088468, -193.5000000000000000, 0.9151456172430280089 ) ) ;
#28597 = EDGE_LOOP ( 'NONE', ( #44231, #11755, #21875, #27212 ) ) ;
#28598 = AXIS2_PLACEMENT_3D ( 'NONE', #24428, #12332, #40193 ) ;
#28599 = ORIENTED_EDGE ( 'NONE', *, *, #31579, .F. ) ;
#28600 = CARTESIAN_POINT ( 'NONE',  ( 0.000000000000000000, -74.94395191227387443, 33.51582005713760282 ) ) ;
#28601 = DIRECTION ( 'NONE',  ( -0.000000000000000000, -0.9927088740980548609, -0.1205366802553164696 ) ) ;
#28602 = CARTESIAN_POINT ( 'NONE',  ( 64.01121016852529522, -189.7472609257535510, -54.50618404930953176 ) ) ;
#28603 = DIRECTION ( 'NONE',  ( 0.000000000000000000, -1.000000000000000000, 0.000000000000000000 ) ) ;
#28604 = FACE_OUTER_BOUND ( 'NONE', #45722, .T. ) ;
#28605 = CARTESIAN_POINT ( 'NONE',  ( -48.47912675150883643, -213.5000000000000000, -125.0000000000000568 ) ) ;
#28606 = ADVANCED_FACE ( 'NONE', ( #24252 ), #27670, .F. ) ;
#28607 = EDGE_CURVE ( 'NONE', #1605, #49769, #8218, .T. ) ;
#28608 = ITEM_DEFINED_TRANSFORMATION ( 'NONE', 'NONE', #26752,  #31742 ) ;
#28609 = DIRECTION ( 'NONE',  ( 0.8294056854501971054, 0.000000000000000000, 0.5586467658036594619 ) ) ;
#28610 = CARTESIAN_POINT ( 'NONE',  ( 6.039888445539280504, -183.6283474603465606, 111.3726929437940498 ) ) ;
#28611 = LINE ( 'NONE', #41757, #48333 ) ;
#28612 = CARTESIAN_POINT ( 'NONE',  ( -238.7407812814481076, -213.5000000000000000, 41.45482488023466772 ) ) ;
#28613 = ORIENTED_EDGE ( 'NONE', *, *, #28681, .T. ) ;
#28614 = ORIENTED_EDGE ( 'NONE', *, *, #17023, .T. ) ;
#28615 = VECTOR ( 'NONE', #5140, 1000.000000000000000 ) ;
#28616 = CARTESIAN_POINT ( 'NONE',  ( 0.000000000000000000, -116.3883358649361526, -58.56982357178523557 ) ) ;
#28617 = CARTESIAN_POINT ( 'NONE',  ( -48.47912675150885065, -177.1207230881787780, 6.938893903907228378E-15 ) ) ;
#28618 = DIRECTION ( 'NONE',  ( 0.000000000000000000, 0.000000000000000000, 1.000000000000000000 ) ) ;
#28619 = ORIENTED_EDGE ( 'NONE', *, *, #22461, .F. ) ;
#28620 = ORIENTED_EDGE ( 'NONE', *, *, #17404, .T. ) ;
#28621 = VERTEX_POINT ( 'NONE', #12663 ) ;
#28622 = DIRECTION ( 'NONE',  ( -0.9720229140804139689, 0.000000000000000000, 0.2348860457809708036 ) ) ;
#28623 = DIRECTION ( 'NONE',  ( 0.000000000000000000, 0.000000000000000000, 1.000000000000000000 ) ) ;
#28624 = EDGE_CURVE ( 'NONE', #30907, #45145, #10340, .T. ) ;
#28625 = CARTESIAN_POINT ( 'NONE',  ( -153.7332855749581881, -175.3837268820161057, 67.42819922234390617 ) ) ;
#28626 = CARTESIAN_POINT ( 'NONE',  ( -332.3517673607765914, -76.43926241122620979, -35.68215131113738181 ) ) ;
#28627 = VECTOR ( 'NONE', #37624, 1000.000000000000000 ) ;
#28628 = VERTEX_POINT ( 'NONE', #320 ) ;
#28629 = CARTESIAN_POINT ( 'NONE',  ( -332.3517673607765914, -123.5000000000000284, 0.000000000000000000 ) ) ;
#28630 = CYLINDRICAL_SURFACE ( 'NONE', #18468, 4.999999999999997335 ) ;
#28631 = ORIENTED_EDGE ( 'NONE', *, *, #26113, .F. ) ;
#28632 = EDGE_CURVE ( 'NONE', #19724, #13689, #16365, .T. ) ;
#28633 = AXIS2_PLACEMENT_3D ( 'NONE', #19908, #35939, #14674 ) ;
#28634 = CARTESIAN_POINT ( 'NONE',  ( -78.00521078983979351, -175.3837268820161057, 121.4627941443857253 ) ) ;
#28635 = ORIENTED_EDGE ( 'NONE', *, *, #31118, .F. ) ;
#28636 = VERTEX_POINT ( 'NONE', #66 ) ;
#28637 = DIRECTION ( 'NONE',  ( -0.7765238627180437447, 0.000000000000000000, 0.6300878435817094392 ) ) ;
#28638 = VECTOR ( 'NONE', #29660, 1000.000000000000000 ) ;
#28639 = PLANE ( 'NONE',  #10780 ) ;
#28640 = DIRECTION ( 'NONE',  ( 0.000000000000000000, 0.000000000000000000, -1.000000000000000000 ) ) ;
#28643 = EDGE_LOOP ( 'NONE', ( #50554, #30071, #19512, #40111 ) ) ;
#28642 = DIRECTION ( 'NONE',  ( -0.000000000000000000, 1.000000000000000000, -0.000000000000000000 ) ) ;
#28641 = CARTESIAN_POINT ( 'NONE',  ( -336.3521761649654422, -81.08339623743702873, -41.09453333279329712 ) ) ;
#28644 = AXIS2_PLACEMENT_3D ( 'NONE', #35819, #12670, #16116 ) ;
#28645 = CARTESIAN_POINT ( 'NONE',  ( -21.46839590530488451, -183.6283474603465606, 122.0467960216650738 ) ) ;
#28646 = ORIENTED_EDGE ( 'NONE', *, *, #49903, .F. ) ;
#28647 = PLANE ( 'NONE',  #47397 ) ;
#28648 = DIRECTION ( 'NONE',  ( -0.000000000000000000, 1.000000000000000000, -0.000000000000000000 ) ) ;
#28649 = ORIENTED_EDGE ( 'NONE', *, *, #11307, .T. ) ;
#28650 = DIRECTION ( 'NONE',  ( -0.000000000000000000, -0.1205366802553130001, 0.9927088740980551940 ) ) ;
#28651 = CARTESIAN_POINT ( 'NONE',  ( -332.3517673607765914, -174.3267994849386184, -31.88473700876087591 ) ) ;
#28653 = PLANE ( 'NONE',  #9747 ) ;
#28652 = DIRECTION ( 'NONE',  ( 0.000000000000000000, 0.000000000000000000, -1.000000000000000000 ) ) ;
#28654 = ORIENTED_EDGE ( 'NONE', *, *, #12696, .F. ) ;
#28655 =( REPRESENTATION_RELATIONSHIP ('NONE','NONE', #4578, #11639 ) REPRESENTATION_RELATIONSHIP_WITH_TRANSFORMATION ( #42249 )SHAPE_REPRESENTATION_RELATIONSHIP( ) );
#28656 = DIRECTION ( 'NONE',  ( -0.000000000000000000, -0.3546048870425267951, 0.9350162426854181641 ) ) ;
#28657 = DIRECTION ( 'NONE',  ( -0.7378332790417189146, 0.000000000000000000, -0.6749830015182196608 ) ) ;
#28658 = CARTESIAN_POINT ( 'NONE',  ( -332.3517673607765914, -179.2447759217480154, -19.39547174791710660 ) ) ;
#28659 = ORIENTED_EDGE ( 'NONE', *, *, #49650, .T. ) ;
#28660 = DIRECTION ( 'NONE',  ( -0.000000000000000000, 1.000000000000000000, -0.000000000000000000 ) ) ;
#28661 = CARTESIAN_POINT ( 'NONE',  ( -336.3521761649654422, -86.34605966037949543, -45.90766452162698386 ) ) ;
#28662 = VECTOR ( 'NONE', #31397, 1000.000000000000000 ) ;
#28663 = CARTESIAN_POINT ( 'NONE',  ( 52.59568867645218404, -189.7472609257535510, -73.54509967498589162 ) ) ;
#28664 = VERTEX_POINT ( 'NONE', #12408 ) ;
#28665 = ADVANCED_FACE ( 'NONE', ( #32124 ), #48170, .F. ) ;
#28666 = VECTOR ( 'NONE', #47180, 1000.000000000000000 ) ;
#28667 = CARTESIAN_POINT ( 'NONE',  ( -105.4063847101409692, -175.3837268820161057, -111.2847127925096373 ) ) ;
#28668 = VERTEX_POINT ( 'NONE', #44482 ) ;
#28669 = DIRECTION ( 'NONE',  ( 0.000000000000000000, 0.000000000000000000, -1.000000000000000000 ) ) ;
#28670 = ORIENTED_EDGE ( 'NONE', *, *, #43323, .F. ) ;
#28671 = LINE ( 'NONE', #23961, #7180 ) ;
#28672 = DIRECTION ( 'NONE',  ( 0.05924062789370748011, 0.000000000000000000, 0.9982437317643217956 ) ) ;
#28673 = LINE ( 'NONE', #29212, #40294 ) ;
#28674 = LINE ( 'NONE', #50434, #45762 ) ;
#28675 = DIRECTION ( 'NONE',  ( -0.2348860457809775482, 0.000000000000000000, -0.9720229140804121926 ) ) ;
#28676 = VECTOR ( 'NONE', #14559, 1000.000000000000227 ) ;
#28677 = DIRECTION ( 'NONE',  ( 0.000000000000000000, 0.000000000000000000, 1.000000000000000000 ) ) ;
#28678 = VECTOR ( 'NONE', #12216, 1000.000000000000227 ) ;
#28679 = VECTOR ( 'NONE', #14133, 1000.000000000000114 ) ;
#28680 = CARTESIAN_POINT ( 'NONE',  ( -173.0563034899574859, -175.3837268820161057, -10.27263529369817618 ) ) ;
#28681 = EDGE_CURVE ( 'NONE', #37834, #51354, #1099, .T. ) ;
#28682 = FACE_OUTER_BOUND ( 'NONE', #19693, .T. ) ;
#28684 = VERTEX_POINT ( 'NONE', #15592 ) ;
#28683 = PLANE ( 'NONE',  #5232 ) ;
#28685 = ORIENTED_EDGE ( 'NONE', *, *, #26594, .T. ) ;
#28686 = DIRECTION ( 'NONE',  ( -0.000000000000000000, 1.000000000000000000, -0.000000000000000000 ) ) ;
#28687 = DIRECTION ( 'NONE',  ( 0.000000000000000000, 0.000000000000000000, -1.000000000000000000 ) ) ;
#28688 = VERTEX_POINT ( 'NONE', #7942 ) ;
#28689 = ORIENTED_EDGE ( 'NONE', *, *, #8774, .F. ) ;
#28690 = ORIENTED_EDGE ( 'NONE', *, *, #48797, .F. ) ;
#28691 = LINE ( 'NONE', #7706, #6557 ) ;
#28692 = AXIS2_PLACEMENT_3D ( 'NONE', #20012, #48664, #16079 ) ;
#28693 = LINE ( 'NONE', #24771, #4316 ) ;
#28694 = CARTESIAN_POINT ( 'NONE',  ( -332.3517673607765914, -64.50000000000000000, -2.632288850093980503 ) ) ;
#28695 = ORIENTED_EDGE ( 'NONE', *, *, #3369, .T. ) ;
#28696 = ORIENTED_EDGE ( 'NONE', *, *, #31097, .F. ) ;
#28697 = AXIS2_PLACEMENT_3D ( 'NONE', #28883, #25222, #44934 ) ;
#28698 = FACE_OUTER_BOUND ( 'NONE', #17295, .T. ) ;
#28699 = FACE_OUTER_BOUND ( 'NONE', #18832, .T. ) ;
#28701 = EDGE_LOOP ( 'NONE', ( #24747, #37455, #6454, #33726 ) ) ;
#28700 = DIRECTION ( 'NONE',  ( -0.000000000000000000, 1.000000000000000000, -0.000000000000000000 ) ) ;
#28702 = CARTESIAN_POINT ( 'NONE',  ( 60.58466639580034041, -189.7472609257535510, -61.07445476073405644 ) ) ;
#28703 = LINE ( 'NONE', #32667, #51613 ) ;
#28704 = ORIENTED_EDGE ( 'NONE', *, *, #18240, .F. ) ;
#28705 = DIRECTION ( 'NONE',  ( 0.000000000000000000, 1.000000000000000000, 0.000000000000000000 ) ) ;
#28706 = ORIENTED_EDGE ( 'NONE', *, *, #44831, .T. ) ;
#28707 = EDGE_CURVE ( 'NONE', #11608, #28063, #44742, .T. ) ;
#28708 = CARTESIAN_POINT ( 'NONE',  ( 55.10060313344061456, -193.5000000000000000, 68.17212999877224888 ) ) ;
#28709 = FACE_OUTER_BOUND ( 'NONE', #19133, .T. ) ;
#28710 = DIRECTION ( 'NONE',  ( -1.000000000000000000, 0.000000000000000000, 0.000000000000000000 ) ) ;
#28711 = VECTOR ( 'NONE', #256, 1000.000000000000000 ) ;
#28712 = AXIS2_PLACEMENT_3D ( 'NONE', #45627, #41924, #37726 ) ;
#28713 = EDGE_CURVE ( 'NONE', #35017, #22103, #589, .T. ) ;
#28714 = ORIENTED_EDGE ( 'NONE', *, *, #45833, .T. ) ;
#28715 = VECTOR ( 'NONE', #12528, 1000.000000000000114 ) ;
#28716 = ORIENTED_EDGE ( 'NONE', *, *, #19275, .T. ) ;
#28717 = AXIS2_PLACEMENT_3D ( 'NONE', #34785, #26662, #50845 ) ;
#28718 = DIRECTION ( 'NONE',  ( 0.000000000000000000, -1.000000000000000000, 0.000000000000000000 ) ) ;
#28719 = DIRECTION ( 'NONE',  ( -8.718379230999708359E-17, 0.6631226582407965253, 0.7485107481711000821 ) ) ;
#28720 = ORIENTED_EDGE ( 'NONE', *, *, #13147, .F. ) ;
#28721 = LINE ( 'NONE', #4840, #39262 ) ;
#28722 = CARTESIAN_POINT ( 'NONE',  ( -95.72791768350688812, -177.1207230881787780, -115.7261930397105232 ) ) ;
#28723 = ORIENTED_EDGE ( 'NONE', *, *, #12545, .T. ) ;
#28724 = EDGE_CURVE ( 'NONE', #10667, #27207, #2790, .T. ) ;
#28725 = CARTESIAN_POINT ( 'NONE',  ( 71.09073365861578964, -189.7472609257535510, 32.84887689123991095 ) ) ;
#28726 = ADVANCED_FACE ( 'NONE', ( #23724 ), #39730, .F. ) ;
#28727 = CARTESIAN_POINT ( 'NONE',  ( -332.3517673607765914, -78.25545813661345562, 37.90245108779119931 ) ) ;
#28728 = VERTEX_POINT ( 'NONE', #49985 ) ;
#28729 = DIRECTION ( 'NONE',  ( 0.000000000000000000, -0.000000000000000000, 1.000000000000000000 ) ) ;
#28730 = ORIENTED_EDGE ( 'NONE', *, *, #11232, .F. ) ;
#28731 = ADVANCED_FACE ( 'NONE', ( #45014 ), #37364, .F. ) ;
#28732 = DIRECTION ( 'NONE',  ( 0.000000000000000000, 0.000000000000000000, -1.000000000000000000 ) ) ;
#28733 = VERTEX_POINT ( 'NONE', #41048 ) ;
#28734 = AXIS2_PLACEMENT_3D ( 'NONE', #45961, #30668, #46986 ) ;
#28735 = DIRECTION ( 'NONE',  ( 0.000000000000000000, -0.2393156642875482465, 0.9709418174260544543 ) ) ;
#28736 = LINE ( 'NONE', #13508, #29759 ) ;
#28737 = DIRECTION ( 'NONE',  ( -0.000000000000000000, -0.8229838658936575735, -0.5680647467311540355 ) ) ;
#28738 = DIRECTION ( 'NONE',  ( 0.000000000000000000, 0.000000000000000000, 1.000000000000000000 ) ) ;
#28739 = AXIS2_PLACEMENT_3D ( 'NONE', #22371, #14756, #22890 ) ;
#28740 = ORIENTED_EDGE ( 'NONE', *, *, #16543, .F. ) ;
#28741 = CARTESIAN_POINT ( 'NONE',  ( -48.47912675150885065, -189.7472609257535510, 6.938893903907228378E-15 ) ) ;
#28742 = ORIENTED_EDGE ( 'NONE', *, *, #44512, .T. ) ;
#28743 = EDGE_LOOP ( 'NONE', ( #20265, #32070, #9349, #42815 ) ) ;
#28744 = ADVANCED_FACE ( 'NONE', ( #32895 ), #13980, .T. ) ;
#28745 = DIRECTION ( 'NONE',  ( 0.000000000000000000, 0.000000000000000000, 1.000000000000000000 ) ) ;
#28747 = EDGE_LOOP ( 'NONE', ( #4592, #31121, #9574, #20657 ) ) ;
#28746 = DIRECTION ( 'NONE',  ( -0.000000000000000000, 1.000000000000000000, -0.000000000000000000 ) ) ;
#28748 = VERTEX_POINT ( 'NONE', #9006 ) ;
#28749 = FACE_OUTER_BOUND ( 'NONE', #34329, .T. ) ;
#28750 = VECTOR ( 'NONE', #35676, 1000.000000000000000 ) ;
#28751 = DIRECTION ( 'NONE',  ( 0.000000000000000000, 0.000000000000000000, 1.000000000000000000 ) ) ;
#28752 = AXIS2_PLACEMENT_3D ( 'NONE', #36653, #657, #20101 ) ;
#28753 = CIRCLE ( 'NONE', #41332, 125.0000000000000000 ) ;
#28754 = EDGE_LOOP ( 'NONE', ( #47904, #16767, #41898, #1300 ) ) ;
#28755 = CARTESIAN_POINT ( 'NONE',  ( -332.3517673607765914, -123.5000000000000284, 0.000000000000000000 ) ) ;
#28756 = ORIENTED_EDGE ( 'NONE', *, *, #23303, .T. ) ;
#28757 = LINE ( 'NONE', #16712, #13232 ) ;
#28758 = PLANE ( 'NONE',  #34193 ) ;
#28759 = VECTOR ( 'NONE', #45455, 999.9999999999998863 ) ;
#28760 = CARTESIAN_POINT ( 'NONE',  ( 69.25251857196690253, -193.5000000000000000, 38.92640747825684144 ) ) ;
#28761 = CARTESIAN_POINT ( 'NONE',  ( -170.0000000000000284, -123.5000000000000284, 41.63467731922665394 ) ) ;
#28762 = ORIENTED_EDGE ( 'NONE', *, *, #19282, .T. ) ;
#28763 = ORIENTED_EDGE ( 'NONE', *, *, #18108, .T. ) ;
#28764 = EDGE_LOOP ( 'NONE', ( #1373, #21762, #43250, #36370 ) ) ;
#28765 = DIRECTION ( 'NONE',  ( -1.000000000000000000, 0.000000000000000000, -0.000000000000000000 ) ) ;
#28766 = DIRECTION ( 'NONE',  ( 0.000000000000000000, -1.000000000000000000, 0.000000000000000000 ) ) ;
#28767 = DIRECTION ( 'NONE',  ( -5.782411586589357392E-17, 0.000000000000000000, 1.000000000000000000 ) ) ;
#28768 = FACE_BOUND ( 'NONE', #16054, .T. ) ;
#28769 = DIRECTION ( 'NONE',  ( 0.5586467658036535777, 0.000000000000000000, -0.8294056854502011022 ) ) ;
#28770 = ORIENTED_EDGE ( 'NONE', *, *, #46344, .T. ) ;
#28771 = EDGE_CURVE ( 'NONE', #48639, #18266, #49210, .T. ) ;
#28772 = EDGE_CURVE ( 'NONE', #45713, #14384, #17679, .T. ) ;
#28773 = CIRCLE ( 'NONE', #32164, 125.0000000000000000 ) ;
#28774 = VERTEX_POINT ( 'NONE', #25284 ) ;
#28776 = VERTEX_POINT ( 'NONE', #16891 ) ;
#28775 = CARTESIAN_POINT ( 'NONE',  ( -8.721998590732194856, -193.5000000000000000, -118.5089480183145270 ) ) ;
#28777 = VERTEX_POINT ( 'NONE', #25040 ) ;
#28778 = CARTESIAN_POINT ( 'NONE',  ( 2.066935079424583765, -175.3837268820161057, -114.3245189510257802 ) ) ;
#28779 = CARTESIAN_POINT ( 'NONE',  ( -330.4913330509368166, -123.9999999999993605, 59.99791663049644086 ) ) ;
#28780 = CARTESIAN_POINT ( 'NONE',  ( -339.1964088526558498, -138.3439121830101328, -58.13482838284710397 ) ) ;
#28781 = PLANE ( 'NONE',  #27599 ) ;
#28782 = ORIENTED_EDGE ( 'NONE', *, *, #15658, .T. ) ;
#28783 = EDGE_CURVE ( 'NONE', #48674, #19578, #37104, .T. ) ;
#28784 = DIRECTION ( 'NONE',  ( -0.000000000000000000, -0.1205366802553130001, 0.9927088740980551940 ) ) ;
#28785 = AXIS2_PLACEMENT_3D ( 'NONE', #2897, #42839, #6846 ) ;
#28786 = ORIENTED_EDGE ( 'NONE', *, *, #31346, .T. ) ;
#28787 = CIRCLE ( 'NONE', #6165, 125.0000000000000000 ) ;
#28788 = EDGE_CURVE ( 'NONE', #4396, #44477, #48948, .T. ) ;
#28789 = VERTEX_POINT ( 'NONE', #41559 ) ;
#28790 = DIRECTION ( 'NONE',  ( 0.000000000000000000, -1.000000000000000000, 0.000000000000000000 ) ) ;
#28791 = AXIS2_PLACEMENT_3D ( 'NONE', #21335, #33434, #24487 ) ;
#28792 = EDGE_CURVE ( 'NONE', #48639, #47918, #37887, .T. ) ;
#28793 = SURFACE_STYLE_USAGE ( .BOTH. , #13823 ) ;
#28794 = PLANE ( 'NONE',  #46330 ) ;
#28795 = DIRECTION ( 'NONE',  ( 0.000000000000000000, -0.000000000000000000, -1.000000000000000000 ) ) ;
#28796 = CARTESIAN_POINT ( 'NONE',  ( -332.3517673607765914, -166.6218737817864621, 41.71934804797023588 ) ) ;
#28797 = ADVANCED_FACE ( 'NONE', ( #9776 ), #8680, .T. ) ;
#28798 = CARTESIAN_POINT ( 'NONE',  ( 18.82962626094778003, -177.1207230881787780, 104.1428419024404377 ) ) ;
#28799 = DIRECTION ( 'NONE',  ( 0.000000000000000000, -1.000000000000000000, 0.000000000000000000 ) ) ;
#28800 = DIRECTION ( 'NONE',  ( -0.000000000000000000, 1.000000000000000000, -0.000000000000000000 ) ) ;
#28801 = VECTOR ( 'NONE', #35671, 1000.000000000000114 ) ;
#28802 = ORIENTED_EDGE ( 'NONE', *, *, #4358, .T. ) ;
#28803 = CARTESIAN_POINT ( 'NONE',  ( -147.6585554144535024, -177.1207230881787780, 76.08180419845385245 ) ) ;
#28804 = DIRECTION ( 'NONE',  ( 0.000000000000000000, -1.000000000000000000, -0.000000000000000000 ) ) ;
#28805 = DIRECTION ( 'NONE',  ( -0.000000000000000000, 1.000000000000000000, -0.000000000000000000 ) ) ;
#28806 = FACE_BOUND ( 'NONE', #14453, .T. ) ;
#28807 = ORIENTED_EDGE ( 'NONE', *, *, #22338, .F. ) ;
#28808 = PLANE ( 'NONE',  #8006 ) ;
#28809 = ORIENTED_EDGE ( 'NONE', *, *, #19979, .F. ) ;
#28810 = VECTOR ( 'NONE', #32565, 999.9999999999998863 ) ;
#28811 = PLANE ( 'NONE',  #47934 ) ;
#28812 = ORIENTED_EDGE ( 'NONE', *, *, #46940, .F. ) ;
#28813 = LINE ( 'NONE', #51993, #28801 ) ;
#28814 = ORIENTED_EDGE ( 'NONE', *, *, #20865, .F. ) ;
#28815 = AXIS2_PLACEMENT_3D ( 'NONE', #5244, #1276, #25206 ) ;
#28816 = CARTESIAN_POINT ( 'NONE',  ( -330.4913330509368166, -151.3613951634091848, -52.00954392751743427 ) ) ;
#28817 = LINE ( 'NONE', #44866, #34347 ) ;
#28819 = ORIENTED_EDGE ( 'NONE', *, *, #48348, .F. ) ;
#28818 = CARTESIAN_POINT ( 'NONE',  ( -40.96347969518279797, -175.3837268820161057, -123.7720294769269032 ) ) ;
#28821 = VECTOR ( 'NONE', #51551, 1000.000000000000000 ) ;
#28820 = DIRECTION ( 'NONE',  ( -0.000000000000000000, -0.9709418174260534551, -0.2393156642875516327 ) ) ;
#28822 = ORIENTED_EDGE ( 'NONE', *, *, #17935, .T. ) ;
#28823 = ORIENTED_EDGE ( 'NONE', *, *, #33944, .F. ) ;
#28824 = EDGE_CURVE ( 'NONE', #4373, #30471, #4809, .T. ) ;
#28825 = DIRECTION ( 'NONE',  ( -0.000000000000000000, -0.8854560256532062468, 0.4647231720437755564 ) ) ;
#28827 = DIRECTION ( 'NONE',  ( 0.000000000000000000, -1.000000000000000000, 0.000000000000000000 ) ) ;
#28826 = AXIS2_PLACEMENT_3D ( 'NONE', #15955, #3587, #27755 ) ;
#28828 = ORIENTED_EDGE ( 'NONE', *, *, #49111, .T. ) ;
#28829 =( NAMED_UNIT ( * ) PLANE_ANGLE_UNIT ( ) SI_UNIT ( $, .RADIAN. ) );
#28830 = CARTESIAN_POINT ( 'NONE',  ( -29.85296035031868911, -183.6283474603465606, 122.5936119678275986 ) ) ;
#28831 = PLANE ( 'NONE',  #7865 ) ;
#28832 = EDGE_CURVE ( 'NONE', #45987, #51254, #23803, .T. ) ;
#28833 = EDGE_CURVE ( 'NONE', #43088, #17428, #12878, .T. ) ;
#28834 = EDGE_CURVE ( 'NONE', #5601, #24900, #20829, .T. ) ;
#28835 = ADVANCED_FACE ( 'NONE', ( #29474 ), #5330, .T. ) ;
#28836 = CARTESIAN_POINT ( 'NONE',  ( -145.6517069852673103, -189.7472609257535510, 78.62880929222940551 ) ) ;
#28837 = LINE ( 'NONE', #32536, #21418 ) ;
#28838 = ORIENTED_EDGE ( 'NONE', *, *, #40126, .T. ) ;
#28841 = VERTEX_POINT ( 'NONE', #13464 ) ;
#28840 = CARTESIAN_POINT ( 'NONE',  ( -49.21696003055058810, -193.5000000000000000, 0.6749830015182108900 ) ) ;
#28839 = FACE_OUTER_BOUND ( 'NONE', #15287, .T. ) ;
#28842 = ORIENTED_EDGE ( 'NONE', *, *, #23359, .T. ) ;
#28843 = EDGE_CURVE ( 'NONE', #29027, #12470, #7003, .T. ) ;
#28844 = CARTESIAN_POINT ( 'NONE',  ( -70.42295845586424718, -189.7472609257535510, -123.0587999703025162 ) ) ;
#28845 = ORIENTED_EDGE ( 'NONE', *, *, #1920, .F. ) ;
#28846 = CARTESIAN_POINT ( 'NONE',  ( -339.1964088526558498, -70.60684477890995936, -28.32515014536858189 ) ) ;
#28847 = VECTOR ( 'NONE', #33859, 1000.000000000000227 ) ;
#28848 = ORIENTED_EDGE ( 'NONE', *, *, #32441, .T. ) ;
#28849 = FACE_OUTER_BOUND ( 'NONE', #30787, .T. ) ;
#28850 = CARTESIAN_POINT ( 'NONE',  ( -47.66663987350317200, -175.3837268820161057, -0.5829794791144634614 ) ) ;
#28851 = ORIENTED_EDGE ( 'NONE', *, *, #14687, .T. ) ;
#28852 = EDGE_CURVE ( 'NONE', #38380, #42973, #42255, .T. ) ;
#28853 = CARTESIAN_POINT ( 'NONE',  ( -339.1964088526558498, -157.1712093821526821, 49.66134974749714104 ) ) ;
#28854 = VERTEX_POINT ( 'NONE', #34460 ) ;
#28855 = AXIS2_PLACEMENT_3D ( 'NONE', #2331, #3089, #18360 ) ;
#28856 = EDGE_CURVE ( 'NONE', #45319, #43465, #48157, .T. ) ;
#28857 = ORIENTED_EDGE ( 'NONE', *, *, #11531, .F. ) ;
#28858 = DIRECTION ( 'NONE',  ( 0.000000000000000000, 0.000000000000000000, 1.000000000000000000 ) ) ;
#28859 = CARTESIAN_POINT ( 'NONE',  ( -339.1964088526558498, -122.9999999999993747, 59.00000000000002132 ) ) ;
#28860 = EDGE_CURVE ( 'NONE', #34735, #9360, #30511, .T. ) ;
#28861 = CARTESIAN_POINT ( 'NONE',  ( 73.80528149577284580, -193.5000000000000000, 25.91377046305969145 ) ) ;
#28862 = CARTESIAN_POINT ( 'NONE',  ( -123.4791267515088435, -198.5000000000000000, 80.00000000000000000 ) ) ;
#28863 = VERTEX_POINT ( 'NONE', #22643 ) ;
#28864 = CARTESIAN_POINT ( 'NONE',  ( -332.3517673607765914, -166.5797264208035244, 40.34602258462248159 ) ) ;
#28865 = EDGE_CURVE ( 'NONE', #23646, #44424, #30514, .T. ) ;
#28866 = PRODUCT_CONTEXT ( 'NONE', #15947, 'mechanical' ) ;
#28867 = DIRECTION ( 'NONE',  ( 0.3202698538628416247, 0.000000000000000000, -0.9473263538541900619 ) ) ;
#28868 = AXIS2_PLACEMENT_3D ( 'NONE', #39876, #3905, #12025 ) ;
#28869 = LINE ( 'NONE', #44917, #304 ) ;
#28870 = CARTESIAN_POINT ( 'NONE',  ( -330.4913330509368166, -70.14212160686581399, 27.43969411971463046 ) ) ;
#28871 = EDGE_CURVE ( 'NONE', #17942, #6329, #15417, .T. ) ;
#28872 = LINE ( 'NONE', #44659, #46699 ) ;
#28873 = ORIENTED_EDGE ( 'NONE', *, *, #20480, .T. ) ;
#28874 = VERTEX_POINT ( 'NONE', #34211 ) ;
#28875 = DIRECTION ( 'NONE',  ( 0.000000000000000000, -1.000000000000000000, 0.000000000000000000 ) ) ;
#28876 = CARTESIAN_POINT ( 'NONE',  ( -140.8230258362169707, -175.3837268820161057, 84.24728067916045404 ) ) ;
#28877 = FACE_OUTER_BOUND ( 'NONE', #26775, .T. ) ;
#28878 = EDGE_LOOP ( 'NONE', ( #5895, #49556, #41194, #5593 ) ) ;
#28879 = ORIENTED_EDGE ( 'NONE', *, *, #46344, .F. ) ;
#28880 = ORIENTED_EDGE ( 'NONE', *, *, #24891, .T. ) ;
#28881 = EDGE_CURVE ( 'NONE', #47910, #36663, #30776, .T. ) ;
#28882 = CARTESIAN_POINT ( 'NONE',  ( -339.1964088526558498, -156.6043281241909426, 48.84008046109164525 ) ) ;
#28883 = CARTESIAN_POINT ( 'NONE',  ( -47.55243714407702527, -189.7472609257535510, 0.3758275821142491591 ) ) ;
#28884 = PLANE ( 'NONE',  #21222 ) ;
#28885 = DIRECTION ( 'NONE',  ( 0.000000000000000000, -1.000000000000000000, -0.000000000000000000 ) ) ;
#28886 = VECTOR ( 'NONE', #1904, 1000.000000000000000 ) ;
#28887 = ORIENTED_EDGE ( 'NONE', *, *, #43712, .F. ) ;
#28888 = VECTOR ( 'NONE', #39141, 1000.000000000000000 ) ;
#28889 = CARTESIAN_POINT ( 'NONE',  ( -48.47912675150885065, -189.7472609257535510, 6.938893903907228378E-15 ) ) ;
#28890 = CARTESIAN_POINT ( 'NONE',  ( -121.1142239062970560, -177.1207230881787780, 101.7307360698549132 ) ) ;
#28891 = VERTEX_POINT ( 'NONE', #46824 ) ;
#28892 = CIRCLE ( 'NONE', #43155, 60.00000000000000000 ) ;
#28893 = FACE_OUTER_BOUND ( 'NONE', #51245, .T. ) ;
#28894 = VERTEX_POINT ( 'NONE', #50763 ) ;
#28895 = PLANE ( 'NONE',  #20844 ) ;
#28896 = EDGE_LOOP ( 'NONE', ( #11464, #36176, #12456, #40025 ) ) ;
#28897 = DIRECTION ( 'NONE',  ( 0.6300878435817148793, 0.000000000000000000, -0.7765238627180394149 ) ) ;
#28898 = ADVANCED_FACE ( 'NONE', ( #46561 ), #2917, .T. ) ;
#28899 = EDGE_CURVE ( 'NONE', #51292, #43700, #10044, .T. ) ;
#28900 = CIRCLE ( 'NONE', #8763, 125.0000000000000000 ) ;
#28901 = EDGE_CURVE ( 'NONE', #18053, #38078, #18698, .T. ) ;
#28902 = EDGE_CURVE ( 'NONE', #14774, #5680, #34710, .T. ) ;
#28903 = CARTESIAN_POINT ( 'NONE',  ( 30.50828161901820224, -193.5000000000000000, 96.88131563365348597 ) ) ;
#28904 = CARTESIAN_POINT ( 'NONE',  ( 42.10477485469927927, -193.5000000000000000, 86.13684908212515268 ) ) ;
#28907 = ORIENTED_EDGE ( 'NONE', *, *, #23057, .T. ) ;
#28906 = CARTESIAN_POINT ( 'NONE',  ( -336.3521761649654422, -171.1288023355047585, 34.85916744524404720 ) ) ;
#28905 = DIRECTION ( 'NONE',  ( 0.000000000000000000, 1.000000000000000000, -0.000000000000000000 ) ) ;
#28908 = DIRECTION ( 'NONE',  ( 0.000000000000000000, 0.000000000000000000, 1.000000000000000000 ) ) ;
#28909 = VERTEX_POINT ( 'NONE', #10805 ) ;
#28910 = CARTESIAN_POINT ( 'NONE',  ( 75.17589904515342880, -175.3837268820161057, -18.28755301364250130 ) ) ;
#28911 = CARTESIAN_POINT ( 'NONE',  ( -305.0000000000000568, -65.65568511206123503, -15.93848283698870105 ) ) ;
#28912 = ORIENTED_EDGE ( 'NONE', *, *, #17504, .F. ) ;
#28913 = DIRECTION ( 'NONE',  ( 0.000000000000000000, 0.000000000000000000, 1.000000000000000000 ) ) ;
#28915 = PLANE ( 'NONE',  #6372 ) ;
#28914 = CARTESIAN_POINT ( 'NONE',  ( -102.0975050429524487, -177.1207230881787780, -111.8087531435654256 ) ) ;
#28916 = ORIENTED_EDGE ( 'NONE', *, *, #28843, .F. ) ;
#28917 = FACE_OUTER_BOUND ( 'NONE', #9164, .T. ) ;
#28918 = DIRECTION ( 'NONE',  ( 0.000000000000000000, 0.4739294676984008858, 0.8805628084623552398 ) ) ;
#28919 = DIRECTION ( 'NONE',  ( 0.000000000000000000, 0.000000000000000000, -1.000000000000000000 ) ) ;
#28920 = EDGE_CURVE ( 'NONE', #43333, #11713, #10293, .T. ) ;
#28921 = EDGE_LOOP ( 'NONE', ( #28095, #27082, #8031, #14825 ) ) ;
#28922 = FACE_OUTER_BOUND ( 'NONE', #15841, .T. ) ;
#28923 = PLANE ( 'NONE',  #19865 ) ;
#28924 = CARTESIAN_POINT ( 'NONE',  ( -48.47912675150885065, -193.5000000000000000, -0.9999999999999931166 ) ) ;
#28925 = AXIS2_PLACEMENT_3D ( 'NONE', #41004, #21043, #41260 ) ;
#28926 = DIRECTION ( 'NONE',  ( 0.000000000000000000, 1.000000000000000000, 0.000000000000000000 ) ) ;
#28927 = CIRCLE ( 'NONE', #32260, 125.0000000000000000 ) ;
#28928 = VERTEX_POINT ( 'NONE', #31028 ) ;
#28930 = VECTOR ( 'NONE', #15317, 1000.000000000000000 ) ;
#28929 = DIRECTION ( 'NONE',  ( 0.000000000000000000, 0.000000000000000000, 1.000000000000000000 ) ) ;
#28931 = EDGE_CURVE ( 'NONE', #35, #14481, #6354, .T. ) ;
#28932 = CARTESIAN_POINT ( 'NONE',  ( -48.59739992243022755, -175.3837268820161057, 0.9929810960135230236 ) ) ;
#28933 = ORIENTED_EDGE ( 'NONE', *, *, #28856, .F. ) ;
#28934 = DIRECTION ( 'NONE',  ( 0.000000000000000000, 0.000000000000000000, 1.000000000000000000 ) ) ;
#28935 = DIRECTION ( 'NONE',  ( 0.1476465640024710868, 0.000000000000000000, 0.9890401873221654760 ) ) ;
#28936 = VECTOR ( 'NONE', #16004, 1000.000000000000114 ) ;
#28937 = LINE ( 'NONE', #8987, #25211 ) ;
#28938 = FACE_OUTER_BOUND ( 'NONE', #50167, .T. ) ;
#28939 = CARTESIAN_POINT ( 'NONE',  ( -161.8276685539205744, -193.5000000000000000, 50.28156562190586953 ) ) ;
#28940 = VECTOR ( 'NONE', #10310, 1000.000000000000000 ) ;
#28941 = DIRECTION ( 'NONE',  ( 0.000000000000000000, 0.000000000000000000, 1.000000000000000000 ) ) ;
#28942 = CARTESIAN_POINT ( 'NONE',  ( 26.52087324849106054, -198.5000000000000000, -70.00000000000002842 ) ) ;
#28943 = CARTESIAN_POINT ( 'NONE',  ( 24.15597040328003331, -183.6283474603465606, -101.7307360698544159 ) ) ;
#28945 = ORIENTED_EDGE ( 'NONE', *, *, #32358, .T. ) ;
#28944 = DIRECTION ( 'NONE',  ( 0.000000000000000000, 0.000000000000000000, 1.000000000000000000 ) ) ;
#28946 = VERTEX_POINT ( 'NONE', #38405 ) ;
#28947 = DIRECTION ( 'NONE',  ( 0.9960498426152165630, 0.000000000000000000, 0.08879589532293852283 ) ) ;
#28948 = ORIENTED_EDGE ( 'NONE', *, *, #10104, .F. ) ;
#28949 = ORIENTED_EDGE ( 'NONE', *, *, #42562, .F. ) ;
#28950 = CIRCLE ( 'NONE', #33130, 125.0000000000000000 ) ;
#28951 = EDGE_LOOP ( 'NONE', ( #39331, #29716, #7168, #14749 ) ) ;
#28952 = DIRECTION ( 'NONE',  ( -0.000000000000000000, -1.000000000000000000, 0.000000000000000000 ) ) ;
#28953 = AXIS2_PLACEMENT_3D ( 'NONE', #11263, #11536, #11782 ) ;
#28954 = VECTOR ( 'NONE', #34378, 1000.000000000000000 ) ;
#28955 = EDGE_CURVE ( 'NONE', #39789, #16540, #45653, .T. ) ;
#28956 = DIRECTION ( 'NONE',  ( 0.000000000000000000, 1.000000000000000000, 0.000000000000000000 ) ) ;
#28957 = FACE_OUTER_BOUND ( 'NONE', #42829, .T. ) ;
#28958 = ORIENTED_EDGE ( 'NONE', *, *, #46279, .T. ) ;
#28959 = VERTEX_POINT ( 'NONE', #15025 ) ;
#28960 = VECTOR ( 'NONE', #4652, 999.9999999999998863 ) ;
#28961 = DIRECTION ( 'NONE',  ( -0.000000000000000000, -0.5680647467311569221, -0.8229838658936556861 ) ) ;
#28963 = EDGE_LOOP ( 'NONE', ( #14064, #17124, #10432, #14577 ) ) ;
#28962 = DIRECTION ( 'NONE',  ( -0.4031234292879600778, 0.000000000000000000, -0.9151456172430237901 ) ) ;
#28964 = AXIS2_PLACEMENT_3D ( 'NONE', #36999, #995, #49098 ) ;
#28965 = CIRCLE ( 'NONE', #25606, 125.0000000000000000 ) ;
#28966 = DIRECTION ( 'NONE',  ( 0.000000000000000000, -0.000000000000000000, 1.000000000000000000 ) ) ;
#28967 = ORIENTED_EDGE ( 'NONE', *, *, #19405, .T. ) ;
#28968 = FACE_OUTER_BOUND ( 'NONE', #7749, .T. ) ;
#28969 = ORIENTED_EDGE ( 'NONE', *, *, #11177, .T. ) ;
#28970 = DIRECTION ( 'NONE',  ( 0.000000000000000000, 0.000000000000000000, 1.000000000000000000 ) ) ;
#28971 = LINE ( 'NONE', #25309, #4681 ) ;
#28972 = CARTESIAN_POINT ( 'NONE',  ( -173.1763543514842070, -177.1207230881787780, 8.694908215728872847 ) ) ;
#28973 = AXIS2_PLACEMENT_3D ( 'NONE', #45037, #17700, #8488 ) ;
#28974 = VERTEX_POINT ( 'NONE', #18443 ) ;
#28975 = ORIENTED_EDGE ( 'NONE', *, *, #20026, .T. ) ;
#28976 = CARTESIAN_POINT ( 'NONE',  ( -336.3521761649654422, -181.8730728925770563, 8.732051761644092025 ) ) ;
#28977 = DIRECTION ( 'NONE',  ( 0.000000000000000000, 0.000000000000000000, 1.000000000000000000 ) ) ;
#28978 = VERTEX_POINT ( 'NONE', #10544 ) ;
#28979 = ADVANCED_FACE ( 'NONE', ( #11053 ), #27080, .T. ) ;
#28980 = DIRECTION ( 'NONE',  ( -0.000000000000000000, 1.000000000000000000, -0.000000000000000000 ) ) ;
#28981 = CARTESIAN_POINT ( 'NONE',  ( 56.28386853063362594, -193.5000000000000000, 66.33788548805519270 ) ) ;
#28982 = ORIENTED_EDGE ( 'NONE', *, *, #32378, .T. ) ;
#28983 = CARTESIAN_POINT ( 'NONE',  ( 38.46761263173351608, -193.5000000000000000, 89.80681772907068705 ) ) ;
#28984 = DIRECTION ( 'NONE',  ( -1.000000000000000000, 0.000000000000000000, 0.000000000000000000 ) ) ;
#28985 = EDGE_LOOP ( 'NONE', ( #17586, #51214, #4309, #43752 ) ) ;
#28986 = DIRECTION ( 'NONE',  ( -1.000000000000000000, -0.000000000000000000, -0.000000000000000000 ) ) ;
#28987 = EDGE_LOOP ( 'NONE', ( #38028, #40851, #33052, #30495 ) ) ;
#28988 = FACE_BOUND ( 'NONE', #30808, .T. ) ;
#28989 = AXIS2_PLACEMENT_3D ( 'NONE', #38944, #30295, #30547 ) ;
#28990 = PLANE ( 'NONE',  #48054 ) ;
#28991 = DIRECTION ( 'NONE',  ( 1.000000000000000000, 0.000000000000000000, -0.000000000000000000 ) ) ;
#28992 = EDGE_LOOP ( 'NONE', ( #10700, #46083, #41692, #45035 ) ) ;
#28993 = CIRCLE ( 'NONE', #33209, 125.0000000000000000 ) ;
#28994 = VECTOR ( 'NONE', #49968, 1000.000000000000000 ) ;
#28995 = DIRECTION ( 'NONE',  ( -0.6528221181905227155, 0.000000000000000000, 0.7575112421616191360 ) ) ;
#28996 = FACE_OUTER_BOUND ( 'NONE', #26204, .T. ) ;
#28997 = CARTESIAN_POINT ( 'NONE',  ( -170.0000000000000284, -123.5000000000000284, 0.000000000000000000 ) ) ;
#28998 = ADVANCED_FACE ( 'NONE', ( #30182 ), #25717, .T. ) ;
#28999 = CARTESIAN_POINT ( 'NONE',  ( 31.84037011350117297, -189.7472609257535510, -94.47107458416900272 ) ) ;
#29000 = VERTEX_POINT ( 'NONE', #37284 ) ;
#29001 = DIRECTION ( 'NONE',  ( 0.000000000000000000, 0.000000000000000000, -1.000000000000000000 ) ) ;
#29002 = ORIENTED_EDGE ( 'NONE', *, *, #33599, .T. ) ;
#29003 = ORIENTED_EDGE ( 'NONE', *, *, #51644, .T. ) ;
#29004 = ADVANCED_FACE ( 'NONE', ( #49125 ), #45444, .F. ) ;
#29005 = VECTOR ( 'NONE', #4763, 1000.000000000000000 ) ;
#29006 = CARTESIAN_POINT ( 'NONE',  ( -336.3521761649654422, -82.40546666720629787, 42.41660376256258047 ) ) ;
#29008 = VERTEX_POINT ( 'NONE', #46224 ) ;
#29007 = CARTESIAN_POINT ( 'NONE',  ( -132.4142998968130769, -183.6283474603465606, -91.27439114664586839 ) ) ;
#29009 = AXIS2_PLACEMENT_3D ( 'NONE', #35087, #11158, #6724 ) ;
#29010 = EDGE_LOOP ( 'NONE', ( #3091, #12976, #14985, #37196 ) ) ;
#29011 = DIRECTION ( 'NONE',  ( -0.000000000000000000, -1.000000000000000000, 0.000000000000000000 ) ) ;
#29012 = AXIS2_PLACEMENT_3D ( 'NONE', #51827, #36, #27880 ) ;
#29013 = EDGE_CURVE ( 'NONE', #11736, #16530, #22123, .T. ) ;
#29014 = VECTOR ( 'NONE', #42942, 1000.000000000000000 ) ;
#29015 = PLANE ( 'NONE',  #12011 ) ;
#29016 = DIRECTION ( 'NONE',  ( -0.000000000000000000, 1.000000000000000000, -0.000000000000000000 ) ) ;
#29017 = ORIENTED_EDGE ( 'NONE', *, *, #25379, .T. ) ;
#29018 = FACE_OUTER_BOUND ( 'NONE', #48577, .T. ) ;
#29019 = ORIENTED_EDGE ( 'NONE', *, *, #8217, .T. ) ;
#29020 = CARTESIAN_POINT ( 'NONE',  ( -339.1964088526558498, -123.5000000000000284, 0.000000000000000000 ) ) ;
#29021 = DIRECTION ( 'NONE',  ( -0.000000000000000000, 1.000000000000000000, -0.000000000000000000 ) ) ;
#29022 = EDGE_CURVE ( 'NONE', #45092, #26309, #14165, .T. ) ;
#29023 = DIRECTION ( 'NONE',  ( 0.000000000000000000, 0.000000000000000000, 1.000000000000000000 ) ) ;
#29024 = DIRECTION ( 'NONE',  ( -0.000000000000000000, 1.000000000000000000, -0.000000000000000000 ) ) ;
#29025 = ORIENTED_EDGE ( 'NONE', *, *, #49646, .T. ) ;
#29026 = EDGE_LOOP ( 'NONE', ( #35364, #29629, #48382, #39270 ) ) ;
#29027 = VERTEX_POINT ( 'NONE', #33601 ) ;
#29028 = DIRECTION ( 'NONE',  ( -5.399917434947259359E-17, -1.000000000000000000, 0.000000000000000000 ) ) ;
#29029 = PLANE ( 'NONE',  #36941 ) ;
#29030 = ADVANCED_FACE ( 'NONE', ( #21522 ), #1795, .T. ) ;
#29031 = AXIS2_PLACEMENT_3D ( 'NONE', #11801, #3941, #43368 ) ;
#29032 = CIRCLE ( 'NONE', #8076, 125.0000000000000000 ) ;
#29033 = FACE_OUTER_BOUND ( 'NONE', #23364, .T. ) ;
#29034 = AXIS2_PLACEMENT_3D ( 'NONE', #27819, #43857, #11273 ) ;
#29035 = CARTESIAN_POINT ( 'NONE',  ( -330.4913330509368166, -173.1613497474965300, 33.67120938215357029 ) ) ;
#29036 = LINE ( 'NONE', #41133, #1223 ) ;
#29037 = EDGE_LOOP ( 'NONE', ( #42003, #22668, #2745, #42026 ) ) ;
#29038 = AXIS2_PLACEMENT_3D ( 'NONE', #51514, #6338, #20751 ) ;
#29039 = VERTEX_POINT ( 'NONE', #26218 ) ;
#29041 = ORIENTED_EDGE ( 'NONE', *, *, #34498, .T. ) ;
#29040 = DIRECTION ( 'NONE',  ( -0.000000000000000000, 1.000000000000000000, -0.000000000000000000 ) ) ;
#29042 = VERTEX_POINT ( 'NONE', #17590 ) ;
#29043 = CARTESIAN_POINT ( 'NONE',  ( -28.74596282265200387, -193.5000000000000000, 123.4325817657431230 ) ) ;
#29044 = CIRCLE ( 'NONE', #21532, 125.0000000000000000 ) ;
#29045 = EDGE_CURVE ( 'NONE', #44067, #42973, #50171, .T. ) ;
#29046 = DIRECTION ( 'NONE',  ( 0.000000000000000000, 0.000000000000000000, 1.000000000000000000 ) ) ;
#29047 = AXIS2_PLACEMENT_3D ( 'NONE', #37149, #16691, #17721 ) ;
#29048 = CIRCLE ( 'NONE', #24985, 125.0000000000000000 ) ;
#29049 = LINE ( 'NONE', #8822, #30496 ) ;
#29050 = DIRECTION ( 'NONE',  ( -0.000000000000000000, -0.9350162426854169428, -0.3546048870425300148 ) ) ;
#29051 = VERTEX_POINT ( 'NONE', #13630 ) ;
#29052 = DIRECTION ( 'NONE',  ( 1.000000000000000000, -0.000000000000000000, 0.000000000000000000 ) ) ;
#29053 = VECTOR ( 'NONE', #38010, 1000.000000000000000 ) ;
#29055 = EDGE_CURVE ( 'NONE', #25331, #17693, #21262, .T. ) ;
#29054 = ORIENTED_EDGE ( 'NONE', *, *, #20180, .T. ) ;
#29056 = ORIENTED_EDGE ( 'NONE', *, *, #49931, .T. ) ;
#29057 = CARTESIAN_POINT ( 'NONE',  ( -47.51449116960048968, -193.5000000000000000, -0.2635871660690578544 ) ) ;
#29058 = SURFACE_STYLE_FILL_AREA ( #33576 ) ;
#29059 = DIRECTION ( 'NONE',  ( -0.000000000000000000, 1.000000000000000000, -0.000000000000000000 ) ) ;
#29060 = CARTESIAN_POINT ( 'NONE',  ( -19.92568551777507224, -193.5000000000000000, -121.6951149130962904 ) ) ;
#29061 = DIRECTION ( 'NONE',  ( 1.000000000000000000, -0.000000000000000000, -0.000000000000000000 ) ) ;
#29062 = FACE_OUTER_BOUND ( 'NONE', #27405, .T. ) ;
#29063 = ORIENTED_EDGE ( 'NONE', *, *, #44573, .F. ) ;
#29064 = CARTESIAN_POINT ( 'NONE',  ( -48.47912675150885065, -177.1207230881787780, 6.938893903907228378E-15 ) ) ;
#29065 = PLANE ( 'NONE',  #4742 ) ;
#29066 = PLANE ( 'NONE',  #1815 ) ;
#29067 = FACE_BOUND ( 'NONE', #47712, .T. ) ;
#29068 = ORIENTED_EDGE ( 'NONE', *, *, #11873, .T. ) ;
#29069 = AXIS2_PLACEMENT_3D ( 'NONE', #6727, #21721, #38518 ) ;
#29070 = AXIS2_PLACEMENT_3D ( 'NONE', #35280, #11357, #14552 ) ;
#29071 = LINE ( 'NONE', #25918, #34000 ) ;
#29072 = ORIENTED_EDGE ( 'NONE', *, *, #7953, .T. ) ;
#29073 = AXIS2_PLACEMENT_3D ( 'NONE', #46446, #49869, #10426 ) ;
#29074 = DIRECTION ( 'NONE',  ( 0.000000000000000000, 0.000000000000000000, -1.000000000000000000 ) ) ;
#29075 = EDGE_CURVE ( 'NONE', #2077, #34754, #49895, .T. ) ;
#29076 = ORIENTED_EDGE ( 'NONE', *, *, #8806, .F. ) ;
#29077 = EDGE_CURVE ( 'NONE', #47681, #38828, #34119, .T. ) ;
#29078 = LINE ( 'NONE', #1747, #42234 ) ;
#29079 = CARTESIAN_POINT ( 'NONE',  ( -68.21229068036655008, -177.1207230881787780, -123.4325817657429809 ) ) ;
#29080 = AXIS2_PLACEMENT_3D ( 'NONE', #35513, #35776, #14797 ) ;
#29081 = LINE ( 'NONE', #21215, #8314 ) ;
#29082 = AXIS2_PLACEMENT_3D ( 'NONE', #30863, #2996, #51606 ) ;
#29084 = ORIENTED_EDGE ( 'NONE', *, *, #47518, .F. ) ;
#29083 = DIRECTION ( 'NONE',  ( -0.000000000000000000, -1.000000000000000000, 0.000000000000000000 ) ) ;
#29085 = VECTOR ( 'NONE', #17340, 1000.000000000000000 ) ;
#29086 = VECTOR ( 'NONE', #13371, 1000.000000000000000 ) ;
#29087 = ADVANCED_FACE ( 'NONE', ( #5503 ), #1546, .F. ) ;
#29088 = CIRCLE ( 'NONE', #6467, 4.000000000000003553 ) ;
#29089 = CARTESIAN_POINT ( 'NONE',  ( -332.3517673607765914, -128.1121410293017391, 59.82247199109905011 ) ) ;
#29090 = EDGE_LOOP ( 'NONE', ( #15777, #8753, #27301, #23190 ) ) ;
#29091 = ORIENTED_EDGE ( 'NONE', *, *, #6256, .F. ) ;
#29092 = EDGE_CURVE ( 'NONE', #12643, #19641, #29913, .T. ) ;
#29093 = ORIENTED_EDGE ( 'NONE', *, *, #33000, .F. ) ;
#29094 = CARTESIAN_POINT ( 'NONE',  ( 116.9235303384055840, -193.5000000000000000, -9.999999999999971578 ) ) ;
#29095 = DIRECTION ( 'NONE',  ( 0.6965510290630033685, 0.000000000000000000, -0.7175072570443249420 ) ) ;
#29096 = EDGE_CURVE ( 'NONE', #16039, #19239, #17836, .T. ) ;
#29097 = VERTEX_POINT ( 'NONE', #13110 ) ;
#29098 = DIRECTION ( 'NONE',  ( 0.000000000000000000, -0.000000000000000000, 1.000000000000000000 ) ) ;
#29099 = CARTESIAN_POINT ( 'NONE',  ( 46.00000000000000000, 20.00000000000000000, -4.999999999999997335 ) ) ;
#29100 = CARTESIAN_POINT ( 'NONE',  ( -47.63353074800703268, -193.5000000000000000, 0.5338233779648018373 ) ) ;
#29101 = VERTEX_POINT ( 'NONE', #6005 ) ;
#29102 = EDGE_CURVE ( 'NONE', #19173, #33563, #4487, .T. ) ;
#29103 = DIRECTION ( 'NONE',  ( 0.000000000000000000, 0.000000000000000000, -1.000000000000000000 ) ) ;
#29104 = CARTESIAN_POINT ( 'NONE',  ( -336.3521761649654422, -165.9166037625627439, 41.09453333279358134 ) ) ;
#29105 = ORIENTED_EDGE ( 'NONE', *, *, #32930, .T. ) ;
#29108 = VERTEX_POINT ( 'NONE', #33078 ) ;
#29107 = CARTESIAN_POINT ( 'NONE',  ( -162.7543581613524282, -183.6283474603465606, 50.65739320402011003 ) ) ;
#29106 = DIRECTION ( 'NONE',  ( 0.000000000000000000, 0.000000000000000000, 1.000000000000000000 ) ) ;
#29109 = CIRCLE ( 'NONE', #24922, 60.00000000000000000 ) ;
#29110 = ORIENTED_EDGE ( 'NONE', *, *, #29211, .T. ) ;
#29111 = VECTOR ( 'NONE', #39412, 1000.000000000000000 ) ;
#29112 = DIRECTION ( 'NONE',  ( 0.5085311186492154079, 0.000000000000000000, 0.8610436117673585521 ) ) ;
#29113 = EDGE_LOOP ( 'NONE', ( #50623, #9722, #16804, #280 ) ) ;
#29114 = DIRECTION ( 'NONE',  ( -1.000000000000000000, -0.000000000000000000, -0.000000000000000000 ) ) ;
#29115 = EDGE_LOOP ( 'NONE', ( #42757, #21193, #20413, #24576 ) ) ;
#29116 = AXIS2_PLACEMENT_3D ( 'NONE', #24494, #20553, #32377 ) ;
#29117 = LINE ( 'NONE', #25191, #26332 ) ;
#29118 = CARTESIAN_POINT ( 'NONE',  ( -16.77927958806651887, -183.6283474603465606, -120.9136869416130082 ) ) ;
#29119 = ORIENTED_EDGE ( 'NONE', *, *, #32776, .F. ) ;
#29120 = CARTESIAN_POINT ( 'NONE',  ( -305.0000000000000568, -131.2283041299240836, 59.50019592636143528 ) ) ;
#29121 = VERTEX_POINT ( 'NONE', #29133 ) ;
#29122 = ORIENTED_EDGE ( 'NONE', *, *, #49749, .F. ) ;
#29123 = CARTESIAN_POINT ( 'NONE',  ( -332.3517673607765914, -182.5000000000000568, 1.632288850093980725 ) ) ;
#29124 = VECTOR ( 'NONE', #26957, 999.9999999999998863 ) ;
#29125 = DIRECTION ( 'NONE',  ( -1.000000000000000000, 0.000000000000000000, -0.000000000000000000 ) ) ;
#29126 = AXIS2_PLACEMENT_3D ( 'NONE', #29242, #20572, #36606 ) ;
#29127 = CARTESIAN_POINT ( 'NONE',  ( -336.3521761649654422, -70.03480886230919111, 25.08789112700620194 ) ) ;
#29128 = CARTESIAN_POINT ( 'NONE',  ( -365.0000000000001137, -168.5000000000000284, 5.000000000000001776 ) ) ;
#29129 = ORIENTED_EDGE ( 'NONE', *, *, #37829, .T. ) ;
#29130 = CIRCLE ( 'NONE', #6496, 125.0000000000000000 ) ;
#29131 = CARTESIAN_POINT ( 'NONE',  ( -49.45768324380835423, -183.6283474603465606, -0.2059786187411025149 ) ) ;
#29132 = PRODUCT_CONTEXT ( 'NONE', #21312, 'mechanical' ) ;
#29133 = CARTESIAN_POINT ( 'NONE',  ( -336.3521761649654422, -149.0257676989619142, 54.29949524055110999 ) ) ;
#29134 = DIRECTION ( 'NONE',  ( 0.000000000000000000, -0.3546048870425426158, -0.9350162426854120579 ) ) ;
#29135 = CIRCLE ( 'NONE', #8165, 125.0000000000000000 ) ;
#29136 = CARTESIAN_POINT ( 'NONE',  ( 0.000000000000000000, -109.3803758070342838, -57.28556722813713975 ) ) ;
#29137 = DIRECTION ( 'NONE',  ( 0.000000000000000000, -1.000000000000000000, 0.000000000000000000 ) ) ;
#29138 = VECTOR ( 'NONE', #42820, 1000.000000000000227 ) ;
#29139 = PLANE ( 'NONE',  #30741 ) ;
#29140 = ORIENTED_EDGE ( 'NONE', *, *, #4293, .F. ) ;
#29141 = EDGE_CURVE ( 'NONE', #40004, #12706, #33030, .T. ) ;
#29142 = CARTESIAN_POINT ( 'NONE',  ( -45.06671089634843952, -177.1207230881787780, -124.9534129907280544 ) ) ;
#29143 = DIRECTION ( 'NONE',  ( -0.9960498426152158968, 0.000000000000000000, -0.08879589532294571153 ) ) ;
#29144 = ADVANCED_FACE ( 'NONE', ( #43292 ), #26479, .T. ) ;
#29145 = ORIENTED_EDGE ( 'NONE', *, *, #15954, .F. ) ;
#29146 = ADVANCED_FACE ( 'NONE', ( #15450 ), #34626, .T. ) ;
#29147 = DIRECTION ( 'NONE',  ( -1.000000000000000000, 0.000000000000000000, 0.000000000000000000 ) ) ;
#29148 = EDGE_LOOP ( 'NONE', ( #22795, #19207, #23033, #39225 ) ) ;
#29149 = EDGE_CURVE ( 'NONE', #51044, #32234, #37235, .T. ) ;
#29150 = DIRECTION ( 'NONE',  ( 0.000000000000000000, -0.000000000000000000, 1.000000000000000000 ) ) ;
#29151 = AXIS2_PLACEMENT_3D ( 'NONE', #41802, #46019, #10010 ) ;
#29152 = EDGE_CURVE ( 'NONE', #50966, #47996, #47503, .T. ) ;
#29153 = LINE ( 'NONE', #36791, #1864 ) ;
#29154 = PLANE ( 'NONE',  #34640 ) ;
#29155 = CARTESIAN_POINT ( 'NONE',  ( -339.1964088526558498, -64.99044476834248485, -7.608018572113150135 ) ) ;
#29156 = ADVANCED_FACE ( 'NONE', ( #34875 ), #26745, .T. ) ;
#29157 = VECTOR ( 'NONE', #40713, 1000.000000000000000 ) ;
#29158 = EDGE_LOOP ( 'NONE', ( #12688, #34429, #26656, #46902 ) ) ;
#29159 = CARTESIAN_POINT ( 'NONE',  ( 42.96730897722186171, 35.00000000000000000, -41.16782622478179832 ) ) ;
#29160 = EDGE_CURVE ( 'NONE', #17350, #44424, #14941, .T. ) ;
#29161 = DIRECTION ( 'NONE',  ( 0.000000000000000000, 0.000000000000000000, 1.000000000000000000 ) ) ;
#29162 = EDGE_CURVE ( 'NONE', #9912, #48105, #46994, .T. ) ;
#29163 = DIRECTION ( 'NONE',  ( 0.000000000000000000, 1.000000000000000000, -0.000000000000000000 ) ) ;
#29164 = ORIENTED_EDGE ( 'NONE', *, *, #24352, .F. ) ;
#29165 = CARTESIAN_POINT ( 'NONE',  ( -48.47912675150885065, -177.1207230881787780, 6.938893903907228378E-15 ) ) ;
#29166 = VECTOR ( 'NONE', #10618, 1000.000000000000000 ) ;
#29167 = EDGE_CURVE ( 'NONE', #51235, #51254, #47254, .T. ) ;
#29168 = AXIS2_PLACEMENT_3D ( 'NONE', #16313, #24718, #48375 ) ;
#29169 = ORIENTED_EDGE ( 'NONE', *, *, #39302, .F. ) ;
#29170 = DIRECTION ( 'NONE',  ( -0.000000000000000000, 1.000000000000000000, -0.000000000000000000 ) ) ;
#29171 = VECTOR ( 'NONE', #48538, 1000.000000000000000 ) ;
#29172 = EDGE_CURVE ( 'NONE', #27213, #7756, #10974, .T. ) ;
#29173 = VECTOR ( 'NONE', #39394, 1000.000000000000000 ) ;
#29174 = VECTOR ( 'NONE', #32850, 1000.000000000000000 ) ;
#29175 = LINE ( 'NONE', #9213, #19998 ) ;
#29176 = CARTESIAN_POINT ( 'NONE',  ( -69.77312546433407192, -189.7472609257535510, 123.1729094355500109 ) ) ;
#29179 = ORIENTED_EDGE ( 'NONE', *, *, #26318, .T. ) ;
#29178 = DIRECTION ( 'NONE',  ( 1.000000000000000000, -0.000000000000000000, -0.000000000000000000 ) ) ;
#29177 = PLANE ( 'NONE',  #46823 ) ;
#29180 = FACE_OUTER_BOUND ( 'NONE', #51226, .T. ) ;
#29181 = ORIENTED_EDGE ( 'NONE', *, *, #26313, .F. ) ;
#29182 = CARTESIAN_POINT ( 'NONE',  ( -67.22356632362124174, -177.1207230881787780, -123.5865930638409509 ) ) ;
#29183 = DIRECTION ( 'NONE',  ( -0.000000000000000000, 1.000000000000000000, 0.000000000000000000 ) ) ;
#29184 = VERTEX_POINT ( 'NONE', #26997 ) ;
#29185 = PLANE ( 'NONE',  #37588 ) ;
#29188 = ORIENTED_EDGE ( 'NONE', *, *, #26030, .T. ) ;
#29187 = DIRECTION ( 'NONE',  ( 0.000000000000000000, 0.000000000000000000, -1.000000000000000000 ) ) ;
#29186 = LINE ( 'NONE', #45241, #51811 ) ;
#29189 = EDGE_CURVE ( 'NONE', #47995, #48520, #27165, .T. ) ;
#29190 = ORIENTED_EDGE ( 'NONE', *, *, #48436, .F. ) ;
#29191 = FACE_OUTER_BOUND ( 'NONE', #10976, .T. ) ;
#29192 = AXIS2_PLACEMENT_3D ( 'NONE', #4304, #27951, #622 ) ;
#29193 = DIRECTION ( 'NONE',  ( -0.000000000000000000, 1.000000000000000000, -0.000000000000000000 ) ) ;
#29194 = AXIS2_PLACEMENT_3D ( 'NONE', #9169, #25195, #37271 ) ;
#29195 = DIRECTION ( 'NONE',  ( 0.9266896074318317078, 0.000000000000000000, 0.3758275821142421647 ) ) ;
#29196 = EDGE_LOOP ( 'NONE', ( #9431, #276, #7457, #5342 ) ) ;
#29197 = LINE ( 'NONE', #34180, #31561 ) ;
#29198 = DIRECTION ( 'NONE',  ( 0.000000000000000000, -0.000000000000000000, 1.000000000000000000 ) ) ;
#29199 = CARTESIAN_POINT ( 'NONE',  ( -332.3517673607765914, -127.9985676343858501, 58.88711093124869222 ) ) ;
#29200 = CIRCLE ( 'NONE', #35912, 9.999999999999994671 ) ;
#29201 = DIRECTION ( 'NONE',  ( -0.1768902751225592818, 0.000000000000000000, -0.9842305779475992722 ) ) ;
#29202 = ORIENTED_EDGE ( 'NONE', *, *, #44218, .F. ) ;
#29203 = CARTESIAN_POINT ( 'NONE',  ( 1.755575411425451593, -175.3837268820161057, 114.4616734920527392 ) ) ;
#29204 = CARTESIAN_POINT ( 'NONE',  ( 2.449293598294706513E-15, -53.50000000000000000, 20.00000000000000000 ) ) ;
#29205 = EDGE_CURVE ( 'NONE', #29027, #34600, #3349, .T. ) ;
#29206 = LINE ( 'NONE', #12644, #14031 ) ;
#29207 = ORIENTED_EDGE ( 'NONE', *, *, #25799, .T. ) ;
#29208 = VECTOR ( 'NONE', #6040, 1000.000000000000000 ) ;
#29209 = CARTESIAN_POINT ( 'NONE',  ( -161.4019114581580823, -175.3837268820161057, 53.60452120946281696 ) ) ;
#29210 = DIRECTION ( 'NONE',  ( 0.9890401873221654760, 0.000000000000000000, -0.1476465640024710868 ) ) ;
#29211 = EDGE_CURVE ( 'NONE', #25859, #12134, #14665, .T. ) ;
#29212 = CARTESIAN_POINT ( 'NONE',  ( -305.0000000000000568, -178.6135371030394481, 23.71704087764532076 ) ) ;
#29213 = DIRECTION ( 'NONE',  ( -0.000000000000000000, -1.000000000000000000, -0.000000000000000000 ) ) ;
#29214 = EDGE_CURVE ( 'NONE', #48223, #42957, #31457, .T. ) ;
#29215 = ADVANCED_FACE ( 'NONE', ( #39077 ), #38313, .F. ) ;
#29216 = EDGE_CURVE ( 'NONE', #9326, #48404, #13758, .T. ) ;
#29218 = AXIS2_PLACEMENT_3D ( 'NONE', #32265, #36212, #31234 ) ;
#29217 = CARTESIAN_POINT ( 'NONE',  ( -339.1964088526558498, -66.33409060400673241, -14.60509510167901404 ) ) ;
#29219 = CARTESIAN_POINT ( 'NONE',  ( -332.3517673607765914, -135.0638248728647852, 57.91551518289418254 ) ) ;
#29220 = DIRECTION ( 'NONE',  ( 0.8455960035018234011, 0.000000000000000000, 0.5338233779647948429 ) ) ;
#29222 = EDGE_LOOP ( 'NONE', ( #13975, #46028, #16282, #19569 ) ) ;
#29221 = PLANE ( 'NONE',  #32059 ) ;
#29223 = ORIENTED_EDGE ( 'NONE', *, *, #37589, .F. ) ;
#29224 = FACE_OUTER_BOUND ( 'NONE', #42749, .T. ) ;
#29225 = DIRECTION ( 'NONE',  ( 0.000000000000000000, 1.000000000000000000, -0.000000000000000000 ) ) ;
#29227 = VERTEX_POINT ( 'NONE', #38577 ) ;
#29226 = CARTESIAN_POINT ( 'NONE',  ( -260.0000000000000000, -63.50000000000000000, -60.00000000000000711 ) ) ;
#29228 = AXIS2_PLACEMENT_3D ( 'NONE', #39965, #12379, #19741 ) ;
#29229 = VECTOR ( 'NONE', #33534, 1000.000000000000000 ) ;
#29230 = ORIENTED_EDGE ( 'NONE', *, *, #1381, .F. ) ;
#29231 = EDGE_CURVE ( 'NONE', #8999, #48057, #2577, .T. ) ;
#29232 = AXIS2_PLACEMENT_3D ( 'NONE', #46319, #14776, #23171 ) ;
#29233 = ORIENTED_EDGE ( 'NONE', *, *, #23469, .F. ) ;
#29234 = DIRECTION ( 'NONE',  ( 0.000000000000000000, -0.000000000000000000, 1.000000000000000000 ) ) ;
#29235 = VECTOR ( 'NONE', #42866, 1000.000000000000000 ) ;
#29236 = EDGE_CURVE ( 'NONE', #14954, #19312, #31201, .T. ) ;
#29237 = DIRECTION ( 'NONE',  ( 0.000000000000000000, 0.000000000000000000, 1.000000000000000000 ) ) ;
#29238 = EDGE_LOOP ( 'NONE', ( #45608, #41784, #17193, #25377 ) ) ;
#29239 = ADVANCED_FACE ( 'NONE', ( #11225 ), #27251, .T. ) ;
#29240 = CARTESIAN_POINT ( 'NONE',  ( 72.12732647922463514, -183.6283474603465606, 28.81338593824056460 ) ) ;
#29241 = AXIS2_PLACEMENT_3D ( 'NONE', #50198, #5800, #21555 ) ;
#29243 = VERTEX_POINT ( 'NONE', #28025 ) ;
#29242 = CARTESIAN_POINT ( 'NONE',  ( -365.0000000000001137, -78.50000000000002842, 0.000000000000000000 ) ) ;
#29244 = CARTESIAN_POINT ( 'NONE',  ( 74.31448861501728231, -177.1207230881787780, -23.38221600314289361 ) ) ;
#29245 = ORIENTED_EDGE ( 'NONE', *, *, #7610, .T. ) ;
#29246 = FACE_OUTER_BOUND ( 'NONE', #1474, .T. ) ;
#29247 = VERTEX_POINT ( 'NONE', #19895 ) ;
#29248 = CARTESIAN_POINT ( 'NONE',  ( 75.67769207106684348, -183.6283474603465606, 14.49428645563876827 ) ) ;
#29249 = LINE ( 'NONE', #9288, #34061 ) ;
#29250 = CARTESIAN_POINT ( 'NONE',  ( -154.0877180371535360, -189.7472609257535510, -66.87170886601934683 ) ) ;
#29251 = CIRCLE ( 'NONE', #19161, 60.00000000000000000 ) ;
#29252 = ORIENTED_EDGE ( 'NONE', *, *, #47746, .F. ) ;
#29253 = EDGE_LOOP ( 'NONE', ( #8811, #25696, #15364, #19345 ) ) ;
#29254 = CARTESIAN_POINT ( 'NONE',  ( -339.1964088526558498, -103.0458197858333165, -55.34326076196084188 ) ) ;
#29255 = LINE ( 'NONE', #5354, #27500 ) ;
#29256 = ORIENTED_EDGE ( 'NONE', *, *, #13391, .F. ) ;
#29257 = DIRECTION ( 'NONE',  ( 0.000000000000000000, -0.9927088740980530845, 0.1205366802553303057 ) ) ;
#29258 = DIRECTION ( 'NONE',  ( 0.000000000000000000, -1.000000000000000000, 0.000000000000000000 ) ) ;
#29259 = ORIENTED_EDGE ( 'NONE', *, *, #9969, .F. ) ;
#29260 = FACE_BOUND ( 'NONE', #40196, .T. ) ;
#29261 = CARTESIAN_POINT ( 'NONE',  ( 73.09196206113300320, -183.6283474603465606, 29.07697310430964421 ) ) ;
#29262 = EDGE_LOOP ( 'NONE', ( #42429, #4946, #9273, #14836 ) ) ;
#29263 = CARTESIAN_POINT ( 'NONE',  ( 35.67816836544797354, -183.6283474603465606, -92.42591454022746689 ) ) ;
#29264 = ORIENTED_EDGE ( 'NONE', *, *, #4640, .T. ) ;
#29265 = PRODUCT_DEFINITION_FORMATION_WITH_SPECIFIED_SOURCE ( 'ANY', '', #41948, .NOT_KNOWN. ) ;
#29266 = CIRCLE ( 'NONE', #39319, 125.0000000000000000 ) ;
#29267 = CARTESIAN_POINT ( 'NONE',  ( -330.4913330509368166, -150.4759391377560576, -52.47426709956116042 ) ) ;
#29268 = VECTOR ( 'NONE', #20976, 1000.000000000000114 ) ;
#29269 = LINE ( 'NONE', #1140, #41279 ) ;
#29270 = VERTEX_POINT ( 'NONE', #170 ) ;
#29271 = VECTOR ( 'NONE', #34655, 1000.000000000000000 ) ;
#29272 = CARTESIAN_POINT ( 'NONE',  ( -330.4913330509368166, -64.86990808808705822, 6.615309698014281814 ) ) ;
#29273 = LINE ( 'NONE', #45326, #17171 ) ;
#29274 = CARTESIAN_POINT ( 'NONE',  ( -87.28630321566649286, -193.5000000000000000, 118.8234112238818341 ) ) ;
#29275 = EDGE_CURVE ( 'NONE', #47980, #12857, #25527, .T. ) ;
#29276 = ADVANCED_FACE ( 'NONE', ( #16217 ), #44065, .T. ) ;
#29277 = CARTESIAN_POINT ( 'NONE',  ( -53.47502265695599277, -183.6283474603465606, -124.9001241957025883 ) ) ;
#29278 = ORIENTED_EDGE ( 'NONE', *, *, #39450, .T. ) ;
#29279 = DIRECTION ( 'NONE',  ( 0.000000000000000000, 0.000000000000000000, -1.000000000000000000 ) ) ;
#29280 = ORIENTED_EDGE ( 'NONE', *, *, #49642, .T. ) ;
#29281 = ORIENTED_EDGE ( 'NONE', *, *, #14250, .T. ) ;
#29282 = AXIS2_PLACEMENT_3D ( 'NONE', #32786, #16780, #52004 ) ;
#29283 = CARTESIAN_POINT ( 'NONE',  ( 54.46899307705341187, -193.5000000000000000, -70.89911581792813422 ) ) ;
#29285 = ORIENTED_EDGE ( 'NONE', *, *, #11519, .T. ) ;
#29284 = CARTESIAN_POINT ( 'NONE',  ( -145.2888470698896981, -175.3837268820161057, -77.48473115145237955 ) ) ;
#29286 = ORIENTED_EDGE ( 'NONE', *, *, #36352, .F. ) ;
#29287 = LINE ( 'NONE', #1432, #34128 ) ;
#29288 = AXIS2_PLACEMENT_3D ( 'NONE', #37532, #34365, #37782 ) ;
#29289 = CARTESIAN_POINT ( 'NONE',  ( -339.1964088526558498, -122.9999999999993747, 59.00000000000002132 ) ) ;
#29290 = DIRECTION ( 'NONE',  ( 0.6965510290629932655, 0.000000000000000000, 0.7175072570443347120 ) ) ;
#29291 = ORIENTED_EDGE ( 'NONE', *, *, #38223, .F. ) ;
#29292 = DIRECTION ( 'NONE',  ( 0.000000000000000000, 0.000000000000000000, 1.000000000000000000 ) ) ;
#29293 = ADVANCED_FACE ( 'NONE', ( #48801 ), #8332, .F. ) ;
#29294 = VERTEX_POINT ( 'NONE', #40362 ) ;
#29295 = CARTESIAN_POINT ( 'NONE',  ( -44.48323084606168720, -183.6283474603465606, 123.9361149384469769 ) ) ;
#29296 = PLANE ( 'NONE',  #41729 ) ;
#29297 = CARTESIAN_POINT ( 'NONE',  ( -163.0741914257288272, -189.7472609257535510, 47.37063079638398477 ) ) ;
#29298 = CARTESIAN_POINT ( 'NONE',  ( -24.23284180386169240, -183.6283474603465606, -121.6072260099953439 ) ) ;
#29299 = EDGE_LOOP ( 'NONE', ( #50946, #18451, #26793, #47619 ) ) ;
#29300 = VERTEX_POINT ( 'NONE', #35927 ) ;
#29301 = EDGE_CURVE ( 'NONE', #35839, #42243, #39588, .T. ) ;
#29302 = ORIENTED_EDGE ( 'NONE', *, *, #42577, .F. ) ;
#29303 = FACE_OUTER_BOUND ( 'NONE', #18857, .T. ) ;
#29304 = DIRECTION ( 'NONE',  ( -0.9995608365087946812, 0.000000000000000000, 0.02963332782254913048 ) ) ;
#29305 = VECTOR ( 'NONE', #3366, 1000.000000000000000 ) ;
#29306 = CARTESIAN_POINT ( 'NONE',  ( -33.86391487983340909, -189.7472609257535510, 124.1426420773540684 ) ) ;
#29307 = DIRECTION ( 'NONE',  ( 0.000000000000000000, -0.000000000000000000, 1.000000000000000000 ) ) ;
#29308 = ORIENTED_EDGE ( 'NONE', *, *, #44672, .F. ) ;
#29309 = AXIS2_PLACEMENT_3D ( 'NONE', #47740, #46966, #146 ) ;
#29310 = ORIENTED_EDGE ( 'NONE', *, *, #5937, .F. ) ;
#29312 = ORIENTED_EDGE ( 'NONE', *, *, #26296, .T. ) ;
#29311 = DIRECTION ( 'NONE',  ( 0.000000000000000000, -0.9709418174260502354, 0.2393156642875652051 ) ) ;
#29313 = ORIENTED_EDGE ( 'NONE', *, *, #26234, .T. ) ;
#29314 = DIRECTION ( 'NONE',  ( 0.8757349421956412971, 0.000000000000000000, -0.4827922027307366970 ) ) ;
#29315 = CYLINDRICAL_SURFACE ( 'NONE', #15760, 124.9999999999999858 ) ;
#29316 = CARTESIAN_POINT ( 'NONE',  ( -336.3521761649654422, -128.9912765084839066, 58.76657425099337928 ) ) ;
#29317 = DIRECTION ( 'NONE',  ( -0.000000000000000000, 1.000000000000000000, -0.000000000000000000 ) ) ;
#29318 = CYLINDRICAL_SURFACE ( 'NONE', #10837, 125.0000000000000000 ) ;
#29319 = ORIENTED_EDGE ( 'NONE', *, *, #4969, .T. ) ;
#29320 = CARTESIAN_POINT ( 'NONE',  ( 9.518239912201957864, -213.5000000000000000, 110.7307791902283043 ) ) ;
#29321 = ORIENTED_EDGE ( 'NONE', *, *, #13441, .T. ) ;
#29322 = AXIS2_PLACEMENT_3D ( 'NONE', #42713, #10647, #34799 ) ;
#29323 = ADVANCED_FACE ( 'NONE', ( #7804 ), #8575, .T. ) ;
#29324 = ORIENTED_EDGE ( 'NONE', *, *, #18260, .F. ) ;
#29325 = LINE ( 'NONE', #45119, #50596 ) ;
#29326 = DIRECTION ( 'NONE',  ( -0.6528221181905280446, 0.000000000000000000, 0.7575112421616145841 ) ) ;
#29327 = ORIENTED_EDGE ( 'NONE', *, *, #15065, .F. ) ;
#29328 = DIRECTION ( 'NONE',  ( 0.000000000000000000, 0.000000000000000000, 1.000000000000000000 ) ) ;
#29329 = DIRECTION ( 'NONE',  ( -0.5829794791144820021, 0.000000000000000000, 0.8124868780056742068 ) ) ;
#29330 = CARTESIAN_POINT ( 'NONE',  ( -48.47912675150885065, -189.7472609257535510, 6.938893903907228378E-15 ) ) ;
#29331 = EDGE_CURVE ( 'NONE', #30477, #26117, #31372, .T. ) ;
#29332 = DIRECTION ( 'NONE',  ( -0.1182731709213592358, 0.000000000000000000, -0.9929810960135178055 ) ) ;
#29333 = DIRECTION ( 'NONE',  ( -0.000000000000000000, 1.000000000000000000, -0.000000000000000000 ) ) ;
#29334 = DIRECTION ( 'NONE',  ( 0.000000000000000000, -0.000000000000000000, -1.000000000000000000 ) ) ;
#29335 = LINE ( 'NONE', #17781, #48379 ) ;
#29336 = VERTEX_POINT ( 'NONE', #32500 ) ;
#29337 = EDGE_CURVE ( 'NONE', #1331, #9353, #40620, .T. ) ;
#29338 = VECTOR ( 'NONE', #35353, 1000.000000000000000 ) ;
#29339 = DIRECTION ( 'NONE',  ( -0.000000000000000000, 1.000000000000000000, -0.000000000000000000 ) ) ;
#29340 = EDGE_LOOP ( 'NONE', ( #23264, #36181, #18655, #22381 ) ) ;
#29341 = FACE_OUTER_BOUND ( 'NONE', #731, .T. ) ;
#29342 = ORIENTED_EDGE ( 'NONE', *, *, #47325, .T. ) ;
#29343 = DIRECTION ( 'NONE',  ( 0.000000000000000000, 0.000000000000000000, 1.000000000000000000 ) ) ;
#29344 = VERTEX_POINT ( 'NONE', #4641 ) ;
#29345 = CARTESIAN_POINT ( 'NONE',  ( -339.1964088526558498, -123.5000000000000284, 0.000000000000000000 ) ) ;
#29346 = PLANE ( 'NONE',  #3289 ) ;
#29348 = VERTEX_POINT ( 'NONE', #20405 ) ;
#29347 = DIRECTION ( 'NONE',  ( 0.000000000000000000, -0.5680647467311596976, -0.8229838658936536877 ) ) ;
#29349 = EDGE_CURVE ( 'NONE', #7460, #45794, #11230, .T. ) ;
#29350 = DIRECTION ( 'NONE',  ( 0.000000000000000000, 0.000000000000000000, 1.000000000000000000 ) ) ;
#29351 = ORIENTED_EDGE ( 'NONE', *, *, #44543, .T. ) ;
#29352 = ORIENTED_EDGE ( 'NONE', *, *, #9633, .T. ) ;
#29353 = AXIS2_PLACEMENT_3D ( 'NONE', #51175, #10689, #2296 ) ;
#29355 = EDGE_LOOP ( 'NONE', ( #29416, #16638, #6917, #44030 ) ) ;
#29354 = AXIS2_PLACEMENT_3D ( 'NONE', #31083, #43171, #30563 ) ;
#29356 = CARTESIAN_POINT ( 'NONE',  ( -173.4291566779743050, -175.3837268820161057, 3.534122433558353205 ) ) ;
#29357 = CARTESIAN_POINT ( 'NONE',  ( -149.7090673587773040, -175.3837268820161057, -71.61357856150524981 ) ) ;
#29358 = ORIENTED_EDGE ( 'NONE', *, *, #42856, .T. ) ;
#29359 = LINE ( 'NONE', #12806, #9179 ) ;
#29360 = DIRECTION ( 'NONE',  ( 0.000000000000000000, 0.000000000000000000, -1.000000000000000000 ) ) ;
#29361 = CARTESIAN_POINT ( 'NONE',  ( -4.794493649713349015, -189.7472609257535510, -117.1181148702518726 ) ) ;
#29362 = ORIENTED_EDGE ( 'NONE', *, *, #29744, .T. ) ;
#29363 = DIRECTION ( 'NONE',  ( 0.4300652022765115712, 0.000000000000000000, 0.9027978299657477557 ) ) ;
#29364 = CARTESIAN_POINT ( 'NONE',  ( -305.0000000000000568, -69.63373947859463442, 26.42775013958025454 ) ) ;
#29365 = ORIENTED_EDGE ( 'NONE', *, *, #43632, .T. ) ;
#29368 = VERTEX_POINT ( 'NONE', #3871 ) ;
#29367 = CARTESIAN_POINT ( 'NONE',  ( 38.71172987070723082, -189.7472609257535510, -89.56983042009264295 ) ) ;
#29366 = LINE ( 'NONE', #40936, #3028 ) ;
#29369 = ORIENTED_EDGE ( 'NONE', *, *, #18374, .T. ) ;
#29370 = AXIS2_PLACEMENT_3D ( 'NONE', #15024, #31027, #43116 ) ;
#29371 = ORIENTED_EDGE ( 'NONE', *, *, #5757, .F. ) ;
#29372 = DIRECTION ( 'NONE',  ( -0.000000000000000000, 1.000000000000000000, -0.000000000000000000 ) ) ;
#29373 = ORIENTED_EDGE ( 'NONE', *, *, #17686, .T. ) ;
#29374 = EDGE_CURVE ( 'NONE', #2592, #31707, #15455, .T. ) ;
#29375 = FACE_OUTER_BOUND ( 'NONE', #16469, .T. ) ;
#29376 = LINE ( 'NONE', #40413, #13315 ) ;
#29377 = ORIENTED_EDGE ( 'NONE', *, *, #27298, .F. ) ;
#29378 = DIRECTION ( 'NONE',  ( -0.000000000000000000, 0.9927088740980538617, -0.1205366802553232974 ) ) ;
#29379 = VERTEX_POINT ( 'NONE', #31973 ) ;
#29380 = EDGE_CURVE ( 'NONE', #16447, #25328, #38081, .T. ) ;
#29381 = ORIENTED_EDGE ( 'NONE', *, *, #29448, .T. ) ;
#29382 = DIRECTION ( 'NONE',  ( -0.000000000000000000, -0.9927088740980530845, 0.1205366802553303057 ) ) ;
#29383 = DIRECTION ( 'NONE',  ( -0.3482016354344059095, 0.000000000000000000, 0.9374196611341183427 ) ) ;
#29384 = DIRECTION ( 'NONE',  ( -0.000000000000000000, 0.1205366802553095168, -0.9927088740980556381 ) ) ;
#29385 = CARTESIAN_POINT ( 'NONE',  ( -111.3904503173946381, -175.3837268820161057, -106.8558168688113454 ) ) ;
#29386 = EDGE_LOOP ( 'NONE', ( #17315, #38551, #27716, #50649 ) ) ;
#29387 = DIRECTION ( 'NONE',  ( -0.000000000000000000, 1.000000000000000000, -0.000000000000000000 ) ) ;
#29388 = CARTESIAN_POINT ( 'NONE',  ( 43.63512310656540905, -189.7472609257535510, 84.49831343337136502 ) ) ;
#29389 = DIRECTION ( 'NONE',  ( 0.000000000000000000, 0.7485107481711024136, 0.6631226582407937498 ) ) ;
#29390 = DIRECTION ( 'NONE',  ( 0.000000000000000000, -0.000000000000000000, -1.000000000000000000 ) ) ;
#29391 = ADVANCED_FACE ( 'NONE', ( #19634 ), #16479, .F. ) ;
#29392 = CARTESIAN_POINT ( 'NONE',  ( -160.9694636715425702, -175.3837268820161057, 54.50618404931039862 ) ) ;
#29393 = LINE ( 'NONE', #17594, #18135 ) ;
#29394 = ADVANCED_FACE ( 'NONE', ( #11995 ), #12257, .T. ) ;
#29395 = ADVANCED_FACE ( 'NONE', ( #707 ), #16754, .T. ) ;
#29396 = VECTOR ( 'NONE', #37870, 1000.000000000000000 ) ;
#29397 = LINE ( 'NONE', #42001, #13989 ) ;
#29398 = EDGE_LOOP ( 'NONE', ( #27539, #47957, #9061, #35822 ) ) ;
#29399 = ORIENTED_EDGE ( 'NONE', *, *, #16951, .F. ) ;
#29400 = EDGE_CURVE ( 'NONE', #51691, #6345, #51531, .T. ) ;
#29401 = DIRECTION ( 'NONE',  ( -0.000000000000000000, 1.000000000000000000, -0.000000000000000000 ) ) ;
#29402 = CARTESIAN_POINT ( 'NONE',  ( 16.59365244519689497, -183.6283474603465606, -105.5544085257710805 ) ) ;
#29403 = EDGE_LOOP ( 'NONE', ( #7773, #2616, #20408, #36474 ) ) ;
#29404 = ORIENTED_EDGE ( 'NONE', *, *, #41009, .F. ) ;
#29405 = ORIENTED_EDGE ( 'NONE', *, *, #15090, .F. ) ;
#29406 = DIRECTION ( 'NONE',  ( 0.000000000000000000, 1.000000000000000000, -0.000000000000000000 ) ) ;
#29407 = VECTOR ( 'NONE', #33035, 1000.000000000000000 ) ;
#29408 = LINE ( 'NONE', #16571, #27019 ) ;
#29409 = CARTESIAN_POINT ( 'NONE',  ( 53.62339707355158680, -193.5000000000000000, -70.36529243996335481 ) ) ;
#29410 = CARTESIAN_POINT ( 'NONE',  ( -305.0000000000000568, -102.6919536717973926, 56.27632902032055284 ) ) ;
#29411 = ORIENTED_EDGE ( 'NONE', *, *, #4561, .T. ) ;
#29412 = DIRECTION ( 'NONE',  ( 0.000000000000000000, 0.000000000000000000, -1.000000000000000000 ) ) ;
#29413 = DIRECTION ( 'NONE',  ( 0.000000000000000000, 0.000000000000000000, -1.000000000000000000 ) ) ;
#29414 = ORIENTED_EDGE ( 'NONE', *, *, #7183, .T. ) ;
#29415 = CARTESIAN_POINT ( 'NONE',  ( 74.95461934957532435, -193.5000000000000000, -11.83705339977242410 ) ) ;
#29416 = ORIENTED_EDGE ( 'NONE', *, *, #36282, .F. ) ;
#29417 = CARTESIAN_POINT ( 'NONE',  ( -173.2765435274470178, -177.1207230881787780, -7.113702696401505321 ) ) ;
#29418 = ORIENTED_EDGE ( 'NONE', *, *, #16293, .T. ) ;
#29419 = DIRECTION ( 'NONE',  ( 0.000000000000000000, 0.000000000000000000, -1.000000000000000000 ) ) ;
#29420 = VECTOR ( 'NONE', #24292, 1000.000000000000114 ) ;
#29421 = ORIENTED_EDGE ( 'NONE', *, *, #11456, .F. ) ;
#29422 = AXIS2_PLACEMENT_3D ( 'NONE', #27091, #31827, #15037 ) ;
#29423 = AXIS2_PLACEMENT_3D ( 'NONE', #501, #48623, #777 ) ;
#29424 = CARTESIAN_POINT ( 'NONE',  ( -172.4295958414655274, -193.5000000000000000, 3.504489105735796528 ) ) ;
#29425 = CARTESIAN_POINT ( 'NONE',  ( -152.3176060415594861, -177.1207230881787780, -69.58857822034968876 ) ) ;
#29426 = ORIENTED_EDGE ( 'NONE', *, *, #21349, .F. ) ;
#29429 = ORIENTED_EDGE ( 'NONE', *, *, #45972, .T. ) ;
#29428 = CARTESIAN_POINT ( 'NONE',  ( -305.0000000000000568, -171.9335100611925213, 35.41461708323791413 ) ) ;
#29427 = CARTESIAN_POINT ( 'NONE',  ( -48.47912675150885065, -183.6283474603465606, 6.938893903907228378E-15 ) ) ;
#29430 = CARTESIAN_POINT ( 'NONE',  ( -339.1964088526558498, -64.50000000000000000, -0.5000000000000457412 ) ) ;
#29431 = VERTEX_POINT ( 'NONE', #44848 ) ;
#29432 = PLANE ( 'NONE',  #43183 ) ;
#29433 = VERTEX_POINT ( 'NONE', #1206 ) ;
#29434 = EDGE_CURVE ( 'NONE', #13843, #21465, #45126, .T. ) ;
#29435 = ADVANCED_FACE ( 'NONE', ( #45898 ), #45381, .T. ) ;
#29436 = ADVANCED_FACE ( 'NONE', ( #13311 ), #9114, .T. ) ;
#29437 = CYLINDRICAL_SURFACE ( 'NONE', #27524, 125.0000000000000000 ) ;
#29440 = ORIENTED_EDGE ( 'NONE', *, *, #4843, .F. ) ;
#29439 = DIRECTION ( 'NONE',  ( 1.000000000000000000, -5.781354811211787559E-17, 6.525800561035047192E-17 ) ) ;
#29438 = LINE ( 'NONE', #41012, #9005 ) ;
#29441 = ORIENTED_EDGE ( 'NONE', *, *, #10578, .F. ) ;
#29442 = DIRECTION ( 'NONE',  ( -0.000000000000000000, -0.8854560256532126861, -0.4647231720437631775 ) ) ;
#29443 = CARTESIAN_POINT ( 'NONE',  ( -48.47912675150885065, -173.5000000000000284, 6.938893903907228378E-15 ) ) ;
#29445 = VECTOR ( 'NONE', #40586, 1000.000000000000000 ) ;
#29444 = CARTESIAN_POINT ( 'NONE',  ( -165.2002711502080672, -183.6283474603465606, 44.73448837594998651 ) ) ;
#29446 = ORIENTED_EDGE ( 'NONE', *, *, #51338, .F. ) ;
#29447 = FACE_OUTER_BOUND ( 'NONE', #34126, .T. ) ;
#29448 = EDGE_CURVE ( 'NONE', #2870, #45202, #33068, .T. ) ;
#29449 = CARTESIAN_POINT ( 'NONE',  ( -339.1964088526558498, -150.4759391377552618, 52.47426709956155122 ) ) ;
#29450 = DIRECTION ( 'NONE',  ( -0.000000000000000000, 1.000000000000000000, -0.000000000000000000 ) ) ;
#29451 = ORIENTED_EDGE ( 'NONE', *, *, #35030, .T. ) ;
#29452 = EDGE_CURVE ( 'NONE', #12962, #32782, #4917, .T. ) ;
#29453 = DIRECTION ( 'NONE',  ( 1.000000000000000000, -0.000000000000000000, -0.000000000000000000 ) ) ;
#29454 = CARTESIAN_POINT ( 'NONE',  ( 56.28386853063362594, -189.7472609257535510, 66.33788548805517848 ) ) ;
#29455 = EDGE_CURVE ( 'NONE', #37972, #23163, #1174, .T. ) ;
#29456 = LINE ( 'NONE', #45509, #51472 ) ;
#29457 = EDGE_LOOP ( 'NONE', ( #19005, #50419, #14301, #17961 ) ) ;
#29458 = ADVANCED_FACE ( 'NONE', ( #45640 ), #41936, .T. ) ;
#29459 = LINE ( 'NONE', #49711, #18924 ) ;
#29460 = PLANE ( 'NONE',  #5958 ) ;
#29461 = AXIS2_PLACEMENT_3D ( 'NONE', #40762, #4786, #36841 ) ;
#29462 = EDGE_CURVE ( 'NONE', #30840, #32017, #9891, .T. ) ;
#29463 = CARTESIAN_POINT ( 'NONE',  ( -339.1964088526558498, -138.1050951016783301, 57.16590939599346655 ) ) ;
#29464 = FACE_OUTER_BOUND ( 'NONE', #37503, .T. ) ;
#29465 = VECTOR ( 'NONE', #34886, 1000.000000000000000 ) ;
#29466 = CARTESIAN_POINT ( 'NONE',  ( -3.104056038602969636, -183.6283474603465606, -115.4006183233321536 ) ) ;
#29467 = CARTESIAN_POINT ( 'NONE',  ( -305.0000000000000568, -123.5000000000000284, -20.00000000000000355 ) ) ;
#29468 = CARTESIAN_POINT ( 'NONE',  ( -305.0000000000000568, -145.2430625708873322, -55.92172413327827485 ) ) ;
#29470 = ORIENTED_EDGE ( 'NONE', *, *, #18593, .T. ) ;
#29469 = CARTESIAN_POINT ( 'NONE',  ( -60.86541030502398542, -193.5000000000000000, -124.3848060646151623 ) ) ;
#29471 = EDGE_LOOP ( 'NONE', ( #50484, #39248, #2090, #4898 ) ) ;
#29472 = CARTESIAN_POINT ( 'NONE',  ( -93.85419746441394295, -177.1207230881787780, 115.4006183233324805 ) ) ;
#29473 = ADVANCED_FACE ( 'NONE', ( #37478 ), #37737, .F. ) ;
#29474 = FACE_OUTER_BOUND ( 'NONE', #5699, .T. ) ;
#29476 = VERTEX_POINT ( 'NONE', #34055 ) ;
#29475 = DIRECTION ( 'NONE',  ( -0.000000000000000000, 1.000000000000000000, -0.000000000000000000 ) ) ;
#29477 = VERTEX_POINT ( 'NONE', #49055 ) ;
#29478 = VECTOR ( 'NONE', #41846, 1000.000000000000000 ) ;
#29479 = ORIENTED_EDGE ( 'NONE', *, *, #45659, .T. ) ;
#29480 = CARTESIAN_POINT ( 'NONE',  ( -160.2705093830644216, -177.1207230881787780, -55.92572546981520532 ) ) ;
#29481 = CARTESIAN_POINT ( 'NONE',  ( 0.000000000000000000, -63.50000000000000000, 60.00000000000000711 ) ) ;
#29482 = FACE_OUTER_BOUND ( 'NONE', #44547, .T. ) ;
#29483 = ORIENTED_EDGE ( 'NONE', *, *, #21324, .F. ) ;
#29484 = ADVANCED_FACE ( 'NONE', ( #5950 ), #33790, .T. ) ;
#29485 = CARTESIAN_POINT ( 'NONE',  ( -330.4913330509368166, -167.9936954712156023, -38.74998146212117689 ) ) ;
#29487 = ORIENTED_EDGE ( 'NONE', *, *, #50302, .F. ) ;
#29486 = DIRECTION ( 'NONE',  ( 0.3482016354344059095, 0.000000000000000000, -0.9374196611341183427 ) ) ;
#29488 = CARTESIAN_POINT ( 'NONE',  ( 141.7825277784304205, -193.5000000000000000, -41.45482488023466061 ) ) ;
#29489 = ORIENTED_EDGE ( 'NONE', *, *, #49650, .F. ) ;
#29490 = CARTESIAN_POINT ( 'NONE',  ( -332.3517673607765914, -173.7880015656344312, -32.72792230702632565 ) ) ;
#29491 = VECTOR ( 'NONE', #23782, 1000.000000000000000 ) ;
#29492 = ORIENTED_EDGE ( 'NONE', *, *, #50142, .T. ) ;
#29493 = EDGE_CURVE ( 'NONE', #34044, #1914, #1991, .T. ) ;
#29494 = EDGE_CURVE ( 'NONE', #4854, #19952, #14618, .T. ) ;
#29495 = EDGE_CURVE ( 'NONE', #37735, #11736, #13563, .T. ) ;
#29496 = EDGE_CURVE ( 'NONE', #1914, #6500, #25912, .T. ) ;
#29497 = CARTESIAN_POINT ( 'NONE',  ( -164.2512865680372727, -175.3837268820161057, -47.13604789772046644 ) ) ;
#29498 = CARTESIAN_POINT ( 'NONE',  ( -158.0280232639029236, -175.3837268820161057, 60.19999396110247147 ) ) ;
#29499 = CIRCLE ( 'NONE', #16952, 125.0000000000000000 ) ;
#29500 = CARTESIAN_POINT ( 'NONE',  ( -336.3521761649654422, -118.8878589706978772, -59.82247199109903590 ) ) ;
#29501 = ADVANCED_FACE ( 'NONE', ( #12770 ), #1736, .T. ) ;
#29502 = VECTOR ( 'NONE', #15584, 1000.000000000000000 ) ;
#29503 = ORIENTED_EDGE ( 'NONE', *, *, #25662, .F. ) ;
#29504 = ORIENTED_EDGE ( 'NONE', *, *, #7964, .F. ) ;
#29505 = CARTESIAN_POINT ( 'NONE',  ( -339.1964088526558498, -151.3613951634092700, -52.00954392751739164 ) ) ;
#29506 = PLANE ( 'NONE',  #18292 ) ;
#29507 = ORIENTED_EDGE ( 'NONE', *, *, #16216, .F. ) ;
#29508 = ADVANCED_FACE ( 'NONE', ( #18032 ), #18544, .T. ) ;
#29509 = CARTESIAN_POINT ( 'NONE',  ( -330.4913330509368166, -109.6270296344155923, 58.37414404713457117 ) ) ;
#29510 = VERTEX_POINT ( 'NONE', #34558 ) ;
#29511 = CARTESIAN_POINT ( 'NONE',  ( -48.77118352214581876, -193.5000000000000000, -0.9564009842765195391 ) ) ;
#29512 = ADVANCED_FACE ( 'NONE', ( #50101, #42965, #47184, #18298 ), #14348, .T. ) ;
#29513 = VECTOR ( 'NONE', #11637, 1000.000000000000000 ) ;
#29514 = CARTESIAN_POINT ( 'NONE',  ( -330.4913330509368166, -162.9984922102920848, 43.83057281297495678 ) ) ;
#29515 = ADVANCED_FACE ( 'NONE', ( #51147 ), #14097, .T. ) ;
#29516 = CARTESIAN_POINT ( 'NONE',  ( -171.2399149993172500, -175.3837268820161057, -17.48697739784461547 ) ) ;
#29517 = VERTEX_POINT ( 'NONE', #10139 ) ;
#29518 = AXIS2_PLACEMENT_3D ( 'NONE', #985, #16784, #29360 ) ;
#29519 = DIRECTION ( 'NONE',  ( 0.000000000000000000, -1.191176786837407622E-13, -1.000000000000000000 ) ) ;
#29520 = EDGE_CURVE ( 'NONE', #48301, #34819, #32237, .T. ) ;
#29521 = DIRECTION ( 'NONE',  ( -0.000000000000000000, -0.6631226582407885317, 0.7485107481711069655 ) ) ;
#29522 = ORIENTED_EDGE ( 'NONE', *, *, #38198, .F. ) ;
#29523 = EDGE_CURVE ( 'NONE', #51107, #14767, #45689, .T. ) ;
#29524 = DIRECTION ( 'NONE',  ( 1.000000000000000000, -0.000000000000000000, -0.000000000000000000 ) ) ;
#29525 = CARTESIAN_POINT ( 'NONE',  ( 59.29945538372744096, -177.1207230881787780, 63.31490529818492519 ) ) ;
#29526 = DIRECTION ( 'NONE',  ( -0.000000000000000000, 1.000000000000000000, -0.000000000000000000 ) ) ;
#29527 = DIRECTION ( 'NONE',  ( -1.000000000000000000, 0.000000000000000000, -0.000000000000000000 ) ) ;
#29528 = EDGE_CURVE ( 'NONE', #51044, #11425, #46665, .T. ) ;
#29529 = ORIENTED_EDGE ( 'NONE', *, *, #30769, .T. ) ;
#29530 = LINE ( 'NONE', #44794, #44620 ) ;
#29531 = ORIENTED_EDGE ( 'NONE', *, *, #40290, .F. ) ;
#29532 = ORIENTED_EDGE ( 'NONE', *, *, #35206, .T. ) ;
#29533 = DIRECTION ( 'NONE',  ( -0.000000000000000000, 1.000000000000000000, -0.000000000000000000 ) ) ;
#29535 = ORIENTED_EDGE ( 'NONE', *, *, #13002, .F. ) ;
#29534 = CARTESIAN_POINT ( 'NONE',  ( -171.4462109067799247, -183.6283474603465606, 15.97798378892250426 ) ) ;
#29536 = CIRCLE ( 'NONE', #42138, 125.0000000000000000 ) ;
#29537 = ORIENTED_EDGE ( 'NONE', *, *, #32495, .F. ) ;
#29538 = CARTESIAN_POINT ( 'NONE',  ( -332.3517673607765914, -148.5878911270064009, 53.46519113769075204 ) ) ;
#29539 = CIRCLE ( 'NONE', #11895, 125.0000000000000000 ) ;
#29540 = EDGE_CURVE ( 'NONE', #29932, #39444, #46160, .T. ) ;
#29541 = VECTOR ( 'NONE', #37817, 1000.000000000000114 ) ;
#29542 = EDGE_CURVE ( 'NONE', #8048, #9084, #36432, .T. ) ;
#29543 = LINE ( 'NONE', #25105, #40515 ) ;
#29544 = EDGE_LOOP ( 'NONE', ( #48701, #7869, #21701, #13825 ) ) ;
#29545 = CARTESIAN_POINT ( 'NONE',  ( -166.9492939735806090, -175.3837268820161057, 39.87254040532603483 ) ) ;
#29546 = ORIENTED_EDGE ( 'NONE', *, *, #14633, .T. ) ;
#29547 = CARTESIAN_POINT ( 'NONE',  ( -332.3517673607765914, -119.0014323656137947, -58.88711093124865670 ) ) ;
#29548 = CARTESIAN_POINT ( 'NONE',  ( -48.98765787015805984, -177.1207230881787780, -0.8610436117673551104 ) ) ;
#29549 = FACE_OUTER_BOUND ( 'NONE', #43880, .T. ) ;
#29550 = CARTESIAN_POINT ( 'NONE',  ( -131.1972941934623975, -183.6283474603465606, 92.37913469314123915 ) ) ;
#29551 = ORIENTED_EDGE ( 'NONE', *, *, #50593, .F. ) ;
#29552 = CIRCLE ( 'NONE', #6865, 60.00000000000000000 ) ;
#29553 = ORIENTED_EDGE ( 'NONE', *, *, #19546, .T. ) ;
#29554 = ORIENTED_EDGE ( 'NONE', *, *, #857, .F. ) ;
#29555 = PLANE ( 'NONE',  #40863 ) ;
#29556 = FACE_OUTER_BOUND ( 'NONE', #19169, .T. ) ;
#29557 = CIRCLE ( 'NONE', #32063, 60.00000000000000000 ) ;
#29558 = VECTOR ( 'NONE', #33247, 1000.000000000000000 ) ;
#29559 = DIRECTION ( 'NONE',  ( 0.000000000000000000, 1.000000000000000000, 0.000000000000000000 ) ) ;
#29560 = FACE_OUTER_BOUND ( 'NONE', #49567, .T. ) ;
#29561 = ORIENTED_EDGE ( 'NONE', *, *, #20816, .F. ) ;
#29562 = EDGE_CURVE ( 'NONE', #30970, #43162, #46937, .T. ) ;
#29563 = PRODUCT_DEFINITION_CONTEXT ( 'detailed design', #5204, 'design' ) ;
#29564 = EDGE_CURVE ( 'NONE', #20792, #33649, #50356, .T. ) ;
#29565 = ADVANCED_FACE ( 'NONE', ( #38516 ), #2514, .F. ) ;
#29566 = ORIENTED_EDGE ( 'NONE', *, *, #48504, .T. ) ;
#29568 = EDGE_LOOP ( 'NONE', ( #14386, #3493, #49351, #29207 ) ) ;
#29567 = CARTESIAN_POINT ( 'NONE',  ( -339.1964088526558498, -180.9052250602807703, 13.63415328425337236 ) ) ;
#29569 = ORIENTED_EDGE ( 'NONE', *, *, #4343, .T. ) ;
#29570 = CARTESIAN_POINT ( 'NONE',  ( -336.3521761649654422, -87.81784868886214213, 47.06073758877343494 ) ) ;
#29571 = DIRECTION ( 'NONE',  ( 1.000000000000000000, -0.000000000000000000, 0.000000000000000000 ) ) ;
#29572 = CIRCLE ( 'NONE', #12797, 125.0000000000000000 ) ;
#29573 = DIRECTION ( 'NONE',  ( -0.000000000000000000, 1.000000000000000000, -0.000000000000000000 ) ) ;
#29574 = DIRECTION ( 'NONE',  ( 0.4566292373937140270, 0.000000000000000000, -0.8896570909947467687 ) ) ;
#29575 = ORIENTED_EDGE ( 'NONE', *, *, #45149, .T. ) ;
#29576 = CARTESIAN_POINT ( 'NONE',  ( -16.10442403432824321, -177.1207230881787780, -119.6996507684850428 ) ) ;
#29577 = ORIENTED_EDGE ( 'NONE', *, *, #1637, .F. ) ;
#29578 = VECTOR ( 'NONE', #11578, 1000.000000000000000 ) ;
#29579 = EDGE_LOOP ( 'NONE', ( #16683, #46825, #45632, #46053 ) ) ;
#29580 = DIRECTION ( 'NONE',  ( 1.000000000000000000, -0.000000000000000000, -0.000000000000000000 ) ) ;
#29581 = ADVANCED_FACE ( 'NONE', ( #42723 ), #34810, .F. ) ;
#29582 = LINE ( 'NONE', #33540, #6856 ) ;
#29583 = ORIENTED_EDGE ( 'NONE', *, *, #48758, .F. ) ;
#29584 = DIRECTION ( 'NONE',  ( 0.000000000000000000, 1.000000000000000000, -0.000000000000000000 ) ) ;
#29585 = DIRECTION ( 'NONE',  ( -0.000000000000000000, 0.3546048870425463906, 0.9350162426854107256 ) ) ;
#29586 = CARTESIAN_POINT ( 'NONE',  ( -123.4791267515088435, -198.5000000000000000, 70.00000000000000000 ) ) ;
#29587 = CARTESIAN_POINT ( 'NONE',  ( -46.00000000000000711, 20.00000000000000000, -46.00000000000000000 ) ) ;
#29588 = AXIS2_PLACEMENT_3D ( 'NONE', #48889, #28885, #9202 ) ;
#29589 = AXIS2_PLACEMENT_3D ( 'NONE', #24020, #98, #26540 ) ;
#29590 = EDGE_CURVE ( 'NONE', #13015, #45883, #40625, .T. ) ;
#29591 = LINE ( 'NONE', #41681, #14393 ) ;
#29592 = FACE_BOUND ( 'NONE', #48148, .T. ) ;
#29593 = ORIENTED_EDGE ( 'NONE', *, *, #7672, .F. ) ;
#29594 = AXIS2_PLACEMENT_3D ( 'NONE', #5951, #49582, #49839 ) ;
#29595 = AXIS2_PLACEMENT_3D ( 'NONE', #17727, #34506, #29782 ) ;
#29596 = DIRECTION ( 'NONE',  ( 0.4031234292879730674, 0.000000000000000000, -0.9151456172430181280 ) ) ;
#29597 = ORIENTED_EDGE ( 'NONE', *, *, #43632, .F. ) ;
#29598 = ORIENTED_EDGE ( 'NONE', *, *, #24700, .T. ) ;
#29599 = CARTESIAN_POINT ( 'NONE',  ( -170.0502155641509034, -183.6283474603465606, -29.07697310430886262 ) ) ;
#29600 = CIRCLE ( 'NONE', #33805, 125.0000000000000000 ) ;
#29601 = ORIENTED_EDGE ( 'NONE', *, *, #5069, .T. ) ;
#29602 = DIRECTION ( 'NONE',  ( 0.000000000000000000, 0.000000000000000000, -1.000000000000000000 ) ) ;
#29603 = DIRECTION ( 'NONE',  ( 0.000000000000000000, 0.000000000000000000, -1.000000000000000000 ) ) ;
#29605 = ORIENTED_EDGE ( 'NONE', *, *, #42175, .F. ) ;
#29604 = CARTESIAN_POINT ( 'NONE',  ( -47.49008656418669005, -175.3837268820161057, 0.1476465640024920423 ) ) ;
#29606 = CIRCLE ( 'NONE', #14508, 125.0000000000000000 ) ;
#29607 = PLANE ( 'NONE',  #43669 ) ;
#29608 = ORIENTED_EDGE ( 'NONE', *, *, #18134, .F. ) ;
#29609 = ORIENTED_EDGE ( 'NONE', *, *, #14789, .T. ) ;
#29610 = CIRCLE ( 'NONE', #48947, 125.0000000000000000 ) ;
#29611 = EDGE_LOOP ( 'NONE', ( #51410, #32223, #39278, #10441 ) ) ;
#29612 = LINE ( 'NONE', #9144, #46893 ) ;
#29613 = LINE ( 'NONE', #44877, #41929 ) ;
#29614 = ORIENTED_EDGE ( 'NONE', *, *, #45888, .T. ) ;
#29615 =( LENGTH_UNIT ( ) NAMED_UNIT ( * ) SI_UNIT ( .MILLI., .METRE. ) );
#29616 = CARTESIAN_POINT ( 'NONE',  ( 49.03269102277813829, 30.00000000000000355, -50.83217377521822300 ) ) ;
#29617 = FACE_OUTER_BOUND ( 'NONE', #41466, .T. ) ;
#29618 = ORIENTED_EDGE ( 'NONE', *, *, #20245, .F. ) ;
#29619 = EDGE_CURVE ( 'NONE', #31952, #21665, #8751, .T. ) ;
#29620 = AXIS2_PLACEMENT_3D ( 'NONE', #48673, #4780, #50 ) ;
#29621 = AXIS2_PLACEMENT_3D ( 'NONE', #1498, #36980, #49854 ) ;
#29622 = FACE_OUTER_BOUND ( 'NONE', #43330, .T. ) ;
#29623 = CARTESIAN_POINT ( 'NONE',  ( -48.24424070572787571, -175.3837268820161057, 0.9720229140804191870 ) ) ;
#29624 = ORIENTED_EDGE ( 'NONE', *, *, #8636, .T. ) ;
#29626 = VERTEX_POINT ( 'NONE', #3293 ) ;
#29625 = DIRECTION ( 'NONE',  ( -0.2348860457809842095, 0.000000000000000000, 0.9720229140804107493 ) ) ;
#29627 = AXIS2_PLACEMENT_3D ( 'NONE', #48418, #8458, #32368 ) ;
#29628 = ORIENTED_EDGE ( 'NONE', *, *, #43704, .F. ) ;
#29629 = ORIENTED_EDGE ( 'NONE', *, *, #29692, .F. ) ;
#29630 = LINE ( 'NONE', #31, #40033 ) ;
#29631 = FACE_OUTER_BOUND ( 'NONE', #37648, .T. ) ;
#29632 = ORIENTED_EDGE ( 'NONE', *, *, #50577, .F. ) ;
#29633 = CARTESIAN_POINT ( 'NONE',  ( -339.1964088526558498, -157.9941932480470541, -49.09328500076547641 ) ) ;
#29634 = AXIS2_PLACEMENT_3D ( 'NONE', #20420, #36440, #3615 ) ;
#29635 = CARTESIAN_POINT ( 'NONE',  ( -48.47912675150885065, -177.1207230881787780, 6.938893903907228378E-15 ) ) ;
#29636 = ORIENTED_EDGE ( 'NONE', *, *, #10840, .T. ) ;
#29637 = FACE_OUTER_BOUND ( 'NONE', #43119, .T. ) ;
#29638 = ORIENTED_EDGE ( 'NONE', *, *, #49998, .F. ) ;
#29639 = EDGE_LOOP ( 'NONE', ( #46962, #27067, #47431, #15828 ) ) ;
#29640 = CARTESIAN_POINT ( 'NONE',  ( -47.55243714407702527, -193.5000000000000000, 0.3758275821142491591 ) ) ;
#29641 = DIRECTION ( 'NONE',  ( -0.8610436117673548884, 0.000000000000000000, -0.5085311186492216251 ) ) ;
#29642 = ADVANCED_FACE ( 'NONE', ( #2764 ), #30891, .T. ) ;
#29643 = DIRECTION ( 'NONE',  ( 0.000000000000000000, 0.000000000000000000, 1.000000000000000000 ) ) ;
#29644 = PLANE ( 'NONE',  #48381 ) ;
#29645 = ORIENTED_EDGE ( 'NONE', *, *, #20210, .T. ) ;
#29646 = DIRECTION ( 'NONE',  ( 0.000000000000000000, -0.000000000000000000, -1.000000000000000000 ) ) ;
#29647 = CIRCLE ( 'NONE', #49813, 25.00456841203572722 ) ;
#29648 = LINE ( 'NONE', #28864, #36459 ) ;
#29649 = ITEM_DEFINED_TRANSFORMATION ( 'NONE', 'NONE', #13328,  #31742 ) ;
#29650 = DIRECTION ( 'NONE',  ( -0.000000000000000000, 1.000000000000000000, -0.000000000000000000 ) ) ;
#29651 = CARTESIAN_POINT ( 'NONE',  ( 11.52087324849114580, -173.5000000000000284, 60.00000000000002132 ) ) ;
#29652 = ORIENTED_EDGE ( 'NONE', *, *, #12124, .T. ) ;
#29653 = CARTESIAN_POINT ( 'NONE',  ( -165.5546359831674295, -177.1207230881787780, 43.79868877201493405 ) ) ;
#29654 = CARTESIAN_POINT ( 'NONE',  ( 36.84288420123322538, -183.6283474603465606, 91.35181687837501840 ) ) ;
#29655 = VECTOR ( 'NONE', #28947, 1000.000000000000114 ) ;
#29656 = CARTESIAN_POINT ( 'NONE',  ( -82.67254833784559764, -177.1207230881787780, -120.2323164553484105 ) ) ;
#29657 = ORIENTED_EDGE ( 'NONE', *, *, #30977, .F. ) ;
#29658 = ADVANCED_FACE ( 'NONE', ( #19067 ), #26154, .T. ) ;
#29659 = PLANE ( 'NONE',  #39512 ) ;
#29660 = DIRECTION ( 'NONE',  ( -0.000000000000000000, 1.000000000000000000, -0.000000000000000000 ) ) ;
#29661 = ORIENTED_EDGE ( 'NONE', *, *, #34328, .F. ) ;
#29662 = VERTEX_POINT ( 'NONE', #15643 ) ;
#29663 = EDGE_CURVE ( 'NONE', #4180, #1918, #34780, .T. ) ;
#29664 = VECTOR ( 'NONE', #9095, 1000.000000000000000 ) ;
#29665 = ORIENTED_EDGE ( 'NONE', *, *, #23098, .F. ) ;
#29666 = DIRECTION ( 'NONE',  ( 0.000000000000000000, -0.000000000000000000, -1.000000000000000000 ) ) ;
#29667 = CIRCLE ( 'NONE', #11091, 125.0000000000000568 ) ;
#29668 = ADVANCED_FACE ( 'NONE', ( #11933 ), #8002, .F. ) ;
#29669 = CARTESIAN_POINT ( 'NONE',  ( -49.30901192927175458, -193.5000000000000000, -124.9972451320097093 ) ) ;
#29670 = DIRECTION ( 'NONE',  ( 0.000000000000000000, -1.000000000000000000, 0.000000000000000000 ) ) ;
#29671 = DIRECTION ( 'NONE',  ( 0.000000000000000000, 1.000000000000000000, 0.000000000000000000 ) ) ;
#29672 = CARTESIAN_POINT ( 'NONE',  ( -332.3517673607765914, -76.43926241122620979, -35.68215131113738181 ) ) ;
#29673 = DIRECTION ( 'NONE',  ( 0.000000000000000000, 0.9927088740980556381, 0.1205366802553095307 ) ) ;
#29674 = ORIENTED_EDGE ( 'NONE', *, *, #16274, .F. ) ;
#29675 = LINE ( 'NONE', #17099, #8015 ) ;
#29676 = ADVANCED_FACE ( 'NONE', ( #11418 ), #47708, .F. ) ;
#29677 = ORIENTED_EDGE ( 'NONE', *, *, #26302, .T. ) ;
#29678 = CARTESIAN_POINT ( 'NONE',  ( -332.3517673607765914, -181.4155151828941825, -11.56382487286496463 ) ) ;
#29679 = EDGE_LOOP ( 'NONE', ( #36778, #8470, #28654, #31689 ) ) ;
#29680 = DIRECTION ( 'NONE',  ( -0.000000000000000000, 1.000000000000000000, 0.000000000000000000 ) ) ;
#29681 = CIRCLE ( 'NONE', #1999, 5.000000000000001776 ) ;
#29682 = ORIENTED_EDGE ( 'NONE', *, *, #17286, .F. ) ;
#29683 = ADVANCED_FACE ( 'NONE', ( #51918 ), #15907, .T. ) ;
#29684 = ADVANCED_FACE ( 'NONE', ( #15382 ), #27710, .F. ) ;
#29685 = VECTOR ( 'NONE', #17334, 1000.000000000000000 ) ;
#29686 = DIRECTION ( 'NONE',  ( 0.000000000000000000, 0.2393156642875582940, 0.9709418174260519008 ) ) ;
#29687 = CARTESIAN_POINT ( 'NONE',  ( -339.1964088526558498, -162.2499814621209850, 44.49369547121574442 ) ) ;
#29688 = ORIENTED_EDGE ( 'NONE', *, *, #5565, .T. ) ;
#29691 = VERTEX_POINT ( 'NONE', #35860 ) ;
#29690 = DIRECTION ( 'NONE',  ( -0.6068001458185834363, 0.000000000000000000, -0.7948544414133608127 ) ) ;
#29689 = CARTESIAN_POINT ( 'NONE',  ( -330.4913330509368166, -65.12585595286530804, -13.87297036558381080 ) ) ;
#29692 = EDGE_CURVE ( 'NONE', #47995, #51589, #7746, .T. ) ;
#29693 = DIRECTION ( 'NONE',  ( -0.000000000000000000, 1.000000000000000000, -0.000000000000000000 ) ) ;
#29694 = ORIENTED_EDGE ( 'NONE', *, *, #22634, .F. ) ;
#29695 = DIRECTION ( 'NONE',  ( -0.7175072570443395970, 0.000000000000000000, 0.6965510290629882695 ) ) ;
#29696 = ORIENTED_EDGE ( 'NONE', *, *, #27781, .F. ) ;
#29697 = CARTESIAN_POINT ( 'NONE',  ( -330.4913330509368166, -73.83865025250327108, -33.67120938215323633 ) ) ;
#29700 = ORIENTED_EDGE ( 'NONE', *, *, #36202, .T. ) ;
#29699 = PLANE ( 'NONE',  #28173 ) ;
#29698 = DIRECTION ( 'NONE',  ( 1.000000000000000000, -3.091579882402533631E-17, 8.151826190875940963E-17 ) ) ;
#29701 = AXIS2_PLACEMENT_3D ( 'NONE', #9657, #5732, #33823 ) ;
#29702 = ORIENTED_EDGE ( 'NONE', *, *, #9516, .F. ) ;
#29703 = DIRECTION ( 'NONE',  ( 0.9473263538541899509, 0.000000000000000000, 0.3202698538628415692 ) ) ;
#29704 = FACE_OUTER_BOUND ( 'NONE', #34998, .T. ) ;
#29705 = PLANE ( 'NONE',  #11402 ) ;
#29706 = ORIENTED_EDGE ( 'NONE', *, *, #22028, .T. ) ;
#29707 = ADVANCED_FACE ( 'NONE', ( #23776 ), #44525, .F. ) ;
#29708 = CARTESIAN_POINT ( 'NONE',  ( -47.92047998570519951, -193.5000000000000000, -0.8294056854501942189 ) ) ;
#29709 = CARTESIAN_POINT ( 'NONE',  ( -330.4913330509368166, -74.40671499923389831, 34.49419324804615172 ) ) ;
#29710 = DIRECTION ( 'NONE',  ( 0.000000000000000000, -1.000000000000000000, 0.000000000000000000 ) ) ;
#29711 = FACE_OUTER_BOUND ( 'NONE', #12575, .T. ) ;
#29712 = ORIENTED_EDGE ( 'NONE', *, *, #17844, .F. ) ;
#29713 = DIRECTION ( 'NONE',  ( 0.000000000000000000, 0.000000000000000000, 1.000000000000000000 ) ) ;
#29714 = PLANE ( 'NONE',  #23931 ) ;
#29715 = DIRECTION ( 'NONE',  ( 0.000000000000000000, 0.000000000000000000, -1.000000000000000000 ) ) ;
#29716 = ORIENTED_EDGE ( 'NONE', *, *, #22387, .F. ) ;
#29717 = CARTESIAN_POINT ( 'NONE',  ( -336.3521761649654422, -72.67320051506121104, 31.88473700876054551 ) ) ;
#29718 = DIRECTION ( 'NONE',  ( 1.000000000000000000, -2.086444717177429095E-17, 8.465038975556428342E-17 ) ) ;
#29719 = AXIS2_PLACEMENT_3D ( 'NONE', #47682, #24271, #43720 ) ;
#29720 = AXIS2_PLACEMENT_3D ( 'NONE', #16809, #9683, #29643 ) ;
#29721 = DIRECTION ( 'NONE',  ( 0.000000000000000000, 0.000000000000000000, 1.000000000000000000 ) ) ;
#29722 = LINE ( 'NONE', #49472, #35828 ) ;
#29723 = VECTOR ( 'NONE', #50871, 1000.000000000000114 ) ;
#29724 = PLANE ( 'NONE',  #24603 ) ;
#29725 = CARTESIAN_POINT ( 'NONE',  ( -48.47912675150885065, -189.7472609257535510, 6.938893903907228378E-15 ) ) ;
#29726 = CYLINDRICAL_SURFACE ( 'NONE', #46366, 125.0000000000000000 ) ;
#29728 = ORIENTED_EDGE ( 'NONE', *, *, #8682, .F. ) ;
#29727 = CARTESIAN_POINT ( 'NONE',  ( -339.1964088526558498, -95.63860483659040312, 52.00954392751717847 ) ) ;
#29729 = ORIENTED_EDGE ( 'NONE', *, *, #27507, .T. ) ;
#29730 = EDGE_CURVE ( 'NONE', #51023, #32303, #22195, .T. ) ;
#29731 = ADVANCED_FACE ( 'NONE', ( #51639 ), #7498, .T. ) ;
#29732 = LINE ( 'NONE', #49484, #17411 ) ;
#29733 = AXIS2_PLACEMENT_3D ( 'NONE', #16976, #1179, #5407 ) ;
#29734 = CARTESIAN_POINT ( 'NONE',  ( -172.9701362814535912, -193.5000000000000000, -11.26891947860193177 ) ) ;
#29736 = ORIENTED_EDGE ( 'NONE', *, *, #35634, .F. ) ;
#29735 = LINE ( 'NONE', #37888, #31237 ) ;
#29737 = ORIENTED_EDGE ( 'NONE', *, *, #19856, .T. ) ;
#29738 = ORIENTED_EDGE ( 'NONE', *, *, #14812, .T. ) ;
#29739 = CARTESIAN_POINT ( 'NONE',  ( -365.0000000000001137, -168.5000000000000284, 0.000000000000000000 ) ) ;
#29740 = EDGE_CURVE ( 'NONE', #48318, #42355, #7115, .T. ) ;
#29741 = CARTESIAN_POINT ( 'NONE',  ( -336.3521761649653854, -121.8677111499054320, 59.97779283292990016 ) ) ;
#29742 = DIRECTION ( 'NONE',  ( -0.000000000000000000, -1.000000000000000000, 0.000000000000000000 ) ) ;
#29743 = VERTEX_POINT ( 'NONE', #19826 ) ;
#29744 = EDGE_CURVE ( 'NONE', #43853, #14242, #23519, .T. ) ;
#29745 = CARTESIAN_POINT ( 'NONE',  ( -48.47912675150885065, -183.6283474603465606, 6.938893903907228378E-15 ) ) ;
#29747 = EDGE_LOOP ( 'NONE', ( #37777, #37254, #41482, #29813 ) ) ;
#29746 = CARTESIAN_POINT ( 'NONE',  ( -8.721998590732194856, -193.5000000000000000, -118.5089480183145270 ) ) ;
#29748 = ADVANCED_FACE ( 'NONE', ( #24547 ), #16158, .F. ) ;
#29749 = LINE ( 'NONE', #25822, #13842 ) ;
#29750 = AXIS2_PLACEMENT_3D ( 'NONE', #44969, #29695, #20783 ) ;
#29751 = EDGE_LOOP ( 'NONE', ( #27094, #19126, #29259, #14340 ) ) ;
#29752 = DIRECTION ( 'NONE',  ( -1.000000000000000000, -0.000000000000000000, -0.000000000000000000 ) ) ;
#29753 = ADVANCED_FACE ( 'NONE', ( #12194 ), #28227, .F. ) ;
#29754 = ORIENTED_EDGE ( 'NONE', *, *, #13833, .F. ) ;
#29755 = VECTOR ( 'NONE', #19687, 1000.000000000000114 ) ;
#29756 = DIRECTION ( 'NONE',  ( 0.000000000000000000, -0.000000000000000000, -1.000000000000000000 ) ) ;
#29757 = FACE_OUTER_BOUND ( 'NONE', #35235, .T. ) ;
#29758 = CARTESIAN_POINT ( 'NONE',  ( -339.1964088526558498, -102.1108035431478811, -54.98865587491830809 ) ) ;
#29759 = VECTOR ( 'NONE', #1682, 1000.000000000000000 ) ;
#29760 = VERTEX_POINT ( 'NONE', #36372 ) ;
#29761 = ORIENTED_EDGE ( 'NONE', *, *, #2236, .F. ) ;
#29762 = DIRECTION ( 'NONE',  ( 0.000000000000000000, 0.000000000000000000, -1.000000000000000000 ) ) ;
#29763 = LINE ( 'NONE', #21109, #17511 ) ;
#29764 = ORIENTED_EDGE ( 'NONE', *, *, #43692, .T. ) ;
#29765 = DIRECTION ( 'NONE',  ( 0.6068001458185834363, 0.000000000000000000, 0.7948544414133608127 ) ) ;
#29766 = ORIENTED_EDGE ( 'NONE', *, *, #13849, .T. ) ;
#29767 = DIRECTION ( 'NONE',  ( 1.000000000000000000, 4.051632851310648003E-17, -7.719741424018512503E-17 ) ) ;
#29768 = VECTOR ( 'NONE', #40273, 1000.000000000000000 ) ;
#29769 = LINE ( 'NONE', #37924, #8816 ) ;
#29770 = ORIENTED_EDGE ( 'NONE', *, *, #4152, .F. ) ;
#29771 = CARTESIAN_POINT ( 'NONE',  ( 76.37123734610607073, -177.1207230881787780, 6.114457023561872262 ) ) ;
#29772 = VERTEX_POINT ( 'NONE', #365 ) ;
#29773 = DIRECTION ( 'NONE',  ( -0.8610436117673621048, 0.000000000000000000, 0.5085311186492095237 ) ) ;
#29774 = CARTESIAN_POINT ( 'NONE',  ( 0.000000000000000000, -63.50000000000000000, 20.00000000000000000 ) ) ;
#29775 = FACE_OUTER_BOUND ( 'NONE', #26494, .T. ) ;
#29776 = VERTEX_POINT ( 'NONE', #40562 ) ;
#29777 = LINE ( 'NONE', #21913, #41622 ) ;
#29778 = PLANE ( 'NONE',  #50751 ) ;
#29779 = PLANE ( 'NONE',  #39166 ) ;
#29780 = DIRECTION ( 'NONE',  ( 1.000000000000000000, -0.000000000000000000, -0.000000000000000000 ) ) ;
#29781 = EDGE_LOOP ( 'NONE', ( #48951, #51237, #38227, #31176 ) ) ;
#29782 = DIRECTION ( 'NONE',  ( 0.000000000000000000, 0.000000000000000000, -1.000000000000000000 ) ) ;
#29783 = EDGE_CURVE ( 'NONE', #13545, #44193, #28736, .T. ) ;
#29784 = VERTEX_POINT ( 'NONE', #49780 ) ;
#29785 = VECTOR ( 'NONE', #9426, 1000.000000000000000 ) ;
#29786 = DIRECTION ( 'NONE',  ( 1.043714542225393381E-14, -0.8229838658936536877, 0.5680647467311596976 ) ) ;
#29788 = ORIENTED_EDGE ( 'NONE', *, *, #37215, .T. ) ;
#29787 = DIRECTION ( 'NONE',  ( -0.000000000000000000, 0.5680647467311540355, -0.8229838658936575735 ) ) ;
#29789 = AXIS2_PLACEMENT_3D ( 'NONE', #51131, #39272, #15622 ) ;
#29790 = VECTOR ( 'NONE', #4379, 1000.000000000000000 ) ;
#29791 = ADVANCED_FACE ( 'NONE', ( #25579 ), #21662, .T. ) ;
#29792 = ORIENTED_EDGE ( 'NONE', *, *, #51071, .T. ) ;
#29793 = EDGE_CURVE ( 'NONE', #24508, #1071, #13252, .T. ) ;
#29794 = ADVANCED_FACE ( 'NONE', ( #5641 ), #12708, .F. ) ;
#29795 = VECTOR ( 'NONE', #31592, 1000.000000000000000 ) ;
#29796 = EDGE_CURVE ( 'NONE', #23872, #16769, #28892, .T. ) ;
#29797 = CARTESIAN_POINT ( 'NONE',  ( 0.000000000000000000, -63.50000000000000000, 0.000000000000000000 ) ) ;
#29798 = EDGE_LOOP ( 'NONE', ( #4442, #45729, #51952, #11168 ) ) ;
#29799 = CARTESIAN_POINT ( 'NONE',  ( -85.48706473349325563, -193.5000000000000000, -118.3487137068146637 ) ) ;
#29800 = EDGE_CURVE ( 'NONE', #28470, #39299, #44790, .T. ) ;
#29801 = AXIS2_PLACEMENT_3D ( 'NONE', #17306, #5219, #33051 ) ;
#29802 = VERTEX_POINT ( 'NONE', #4858 ) ;
#29803 = CARTESIAN_POINT ( 'NONE',  ( 36.10886851198521441, -177.1207230881787780, 92.03190238880813467 ) ) ;
#29804 = CARTESIAN_POINT ( 'NONE',  ( -98.10897907742936752, -175.3837268820161057, 114.7252272087849292 ) ) ;
#29805 = CIRCLE ( 'NONE', #15561, 60.00000000000000000 ) ;
#29806 = ADVANCED_FACE ( 'NONE', ( #28996 ), #36904, .T. ) ;
#29808 = CIRCLE ( 'NONE', #20582, 125.0000000000000000 ) ;
#29807 = DIRECTION ( 'NONE',  ( -0.000000000000000000, 1.000000000000000000, -0.000000000000000000 ) ) ;
#29809 = FACE_OUTER_BOUND ( 'NONE', #45997, .T. ) ;
#29810 = VERTEX_POINT ( 'NONE', #17722 ) ;
#29811 = ORIENTED_EDGE ( 'NONE', *, *, #7024, .T. ) ;
#29812 = ADVANCED_FACE ( 'NONE', ( #21386 ), #16692, .T. ) ;
#29813 = ORIENTED_EDGE ( 'NONE', *, *, #39177, .T. ) ;
#29814 = VECTOR ( 'NONE', #7584, 1000.000000000000114 ) ;
#29815 = LINE ( 'NONE', #49557, #31635 ) ;
#29816 = CARTESIAN_POINT ( 'NONE',  ( -47.50057025920934706, -183.6283474603465606, 0.2059786187411091207 ) ) ;
#29817 = ADVANCED_FACE ( 'NONE', ( #21124 ), #29778, .T. ) ;
#29818 = DIRECTION ( 'NONE',  ( 0.5085311186492216251, 0.000000000000000000, -0.8610436117673548884 ) ) ;
#29819 = DIRECTION ( 'NONE',  ( 0.000000000000000000, 0.000000000000000000, -1.000000000000000000 ) ) ;
#29820 = ORIENTED_EDGE ( 'NONE', *, *, #19102, .F. ) ;
#29821 = EDGE_CURVE ( 'NONE', #31094, #10455, #17471, .T. ) ;
#29822 = EDGE_CURVE ( 'NONE', #32303, #28946, #48995, .T. ) ;
#29823 = VERTEX_POINT ( 'NONE', #9053 ) ;
#29825 = EDGE_LOOP ( 'NONE', ( #3715, #43962, #43294, #40132 ) ) ;
#29824 = CARTESIAN_POINT ( 'NONE',  ( -332.3517673607765914, -97.07224986041923387, -53.86626052140510978 ) ) ;
#29826 = ORIENTED_EDGE ( 'NONE', *, *, #38181, .T. ) ;
#29827 = VECTOR ( 'NONE', #18222, 1000.000000000000000 ) ;
#29828 = LINE ( 'NONE', #32987, #9062 ) ;
#29829 = LINE ( 'NONE', #5938, #32543 ) ;
#29830 = AXIS2_PLACEMENT_3D ( 'NONE', #24795, #4564, #27695 ) ;
#29831 = VECTOR ( 'NONE', #27654, 1000.000000000000114 ) ;
#29832 = LINE ( 'NONE', #25629, #30413 ) ;
#29833 = DIRECTION ( 'NONE',  ( 0.000000000000000000, -0.7485107481710977506, 0.6631226582407989678 ) ) ;
#29834 = ORIENTED_EDGE ( 'NONE', *, *, #17837, .F. ) ;
#29835 = CARTESIAN_POINT ( 'NONE',  ( 58.12687231399077348, -183.6283474603465606, -63.33473559879917758 ) ) ;
#29836 = ORIENTED_EDGE ( 'NONE', *, *, #8922, .F. ) ;
#29837 = EDGE_CURVE ( 'NONE', #10187, #44532, #35607, .T. ) ;
#29838 = VERTEX_POINT ( 'NONE', #20605 ) ;
#29839 = DIRECTION ( 'NONE',  ( 0.000000000000000000, 0.000000000000000000, 1.000000000000000000 ) ) ;
#29840 = AXIS2_PLACEMENT_3D ( 'NONE', #32482, #20648, #48530 ) ;
#29841 = DIRECTION ( 'NONE',  ( 0.3202698538628279690, 0.000000000000000000, 0.9473263538541946138 ) ) ;
#29842 = VERTEX_POINT ( 'NONE', #1419 ) ;
#29843 = AXIS2_PLACEMENT_3D ( 'NONE', #1578, #32842, #48896 ) ;
#29844 = DIRECTION ( 'NONE',  ( 0.000000000000000000, -1.000000000000000000, 0.000000000000000000 ) ) ;
#29845 = CARTESIAN_POINT ( 'NONE',  ( -162.9896759831413249, -177.1207230881787780, -50.12318939043961308 ) ) ;
#29846 = CARTESIAN_POINT ( 'NONE',  ( -47.92047998570519951, -183.6283474603465606, -0.8294056854501942189 ) ) ;
#29847 = AXIS2_PLACEMENT_3D ( 'NONE', #48593, #20448, #8111 ) ;
#29848 = CARTESIAN_POINT ( 'NONE',  ( 75.60865171534661044, -177.1207230881787780, -15.07392567185468302 ) ) ;
#29850 = CIRCLE ( 'NONE', #12212, 125.0000000000000000 ) ;
#29849 = DIRECTION ( 'NONE',  ( -0.9646355819083614058, 0.000000000000000000, 0.2635871660690581320 ) ) ;
#29851 = CARTESIAN_POINT ( 'NONE',  ( -305.0000000000000568, -133.3383340306578759, -59.18789727217212970 ) ) ;
#29852 = EDGE_CURVE ( 'NONE', #2274, #43146, #2042, .T. ) ;
#29853 = VERTEX_POINT ( 'NONE', #29525 ) ;
#29854 = DIRECTION ( 'NONE',  ( -0.000000000000000000, 1.000000000000000000, -0.000000000000000000 ) ) ;
#29855 = ORIENTED_EDGE ( 'NONE', *, *, #38040, .F. ) ;
#29856 = EDGE_CURVE ( 'NONE', #38723, #30858, #33212, .T. ) ;
#29857 = VERTEX_POINT ( 'NONE', #49260 ) ;
#29858 = EDGE_CURVE ( 'NONE', #14785, #48301, #29273, .T. ) ;
#29859 = DIRECTION ( 'NONE',  ( -1.000000000000000000, -0.000000000000000000, -0.000000000000000000 ) ) ;
#29860 = EDGE_LOOP ( 'NONE', ( #33508, #47318, #5173, #30185 ) ) ;
#29861 = EDGE_CURVE ( 'NONE', #14965, #22157, #41609, .T. ) ;
#29862 = EDGE_CURVE ( 'NONE', #49603, #17693, #46608, .T. ) ;
#29863 = CARTESIAN_POINT ( 'NONE',  ( -162.3451783319732442, -177.1207230881787780, 51.57055649762783389 ) ) ;
#29864 = CIRCLE ( 'NONE', #45822, 10.00000000000000000 ) ;
#29865 = CARTESIAN_POINT ( 'NONE',  ( -49.32472275501068282, -177.1207230881787780, 0.5338233779647895139 ) ) ;
#29867 = ORIENTED_EDGE ( 'NONE', *, *, #34902, .T. ) ;
#29866 = DIRECTION ( 'NONE',  ( -0.000000000000000000, -0.1205366802553268363, -0.9927088740980534176 ) ) ;
#29868 = AXIS2_PLACEMENT_3D ( 'NONE', #9489, #48920, #5556 ) ;
#29869 = CIRCLE ( 'NONE', #35751, 125.0000000000000000 ) ;
#29870 = LINE ( 'NONE', #25929, #22704 ) ;
#29871 = DIRECTION ( 'NONE',  ( -0.000000000000000000, 0.8229838658936634577, 0.5680647467311457088 ) ) ;
#29872 = VERTEX_POINT ( 'NONE', #19003 ) ;
#29873 = EDGE_LOOP ( 'NONE', ( #9967, #37642, #7363, #12232 ) ) ;
#29874 = EDGE_LOOP ( 'NONE', ( #32897, #13932, #31104, #9126 ) ) ;
#29875 = DIRECTION ( 'NONE',  ( 0.000000000000000000, -1.000000000000000000, -0.000000000000000000 ) ) ;
#29876 = DIRECTION ( 'NONE',  ( 1.000000000000000000, -0.000000000000000000, -0.000000000000000000 ) ) ;
#29877 = EDGE_CURVE ( 'NONE', #20319, #46485, #37306, .T. ) ;
#29878 = AXIS2_PLACEMENT_3D ( 'NONE', #48661, #36822, #4241 ) ;
#29879 = DIRECTION ( 'NONE',  ( 0.000000000000000000, 1.000000000000000000, -0.000000000000000000 ) ) ;
#29880 = AXIS2_PLACEMENT_3D ( 'NONE', #41348, #13507, #45576 ) ;
#29881 = DIRECTION ( 'NONE',  ( 0.000000000000000000, 0.000000000000000000, -1.000000000000000000 ) ) ;
#29882 = CARTESIAN_POINT ( 'NONE',  ( -339.1964088526558498, -96.52406086224361559, 52.47426709956096147 ) ) ;
#29883 = ORIENTED_EDGE ( 'NONE', *, *, #9468, .T. ) ;
#29884 = ADVANCED_FACE ( 'NONE', ( #47122 ), #2964, .F. ) ;
#29885 = ADVANCED_FACE ( 'NONE', ( #42656 ), #22946, .T. ) ;
#29886 = VECTOR ( 'NONE', #34292, 999.9999999999998863 ) ;
#29887 = FACE_OUTER_BOUND ( 'NONE', #7774, .T. ) ;
#29888 = VERTEX_POINT ( 'NONE', #10085 ) ;
#29890 = ORIENTED_EDGE ( 'NONE', *, *, #13599, .F. ) ;
#29889 = DIRECTION ( 'NONE',  ( 0.000000000000000000, 0.000000000000000000, 1.000000000000000000 ) ) ;
#29891 = VERTEX_POINT ( 'NONE', #50299 ) ;
#29892 = EDGE_LOOP ( 'NONE', ( #45077, #41066, #2865, #43893 ) ) ;
#29893 = LINE ( 'NONE', #26729, #44259 ) ;
#29894 = FACE_OUTER_BOUND ( 'NONE', #5902, .T. ) ;
#29895 = ORIENTED_EDGE ( 'NONE', *, *, #40725, .F. ) ;
#29896 = LINE ( 'NONE', #38034, #41411 ) ;
#29897 = CARTESIAN_POINT ( 'NONE',  ( -115.4536696835168641, -193.5000000000000000, -105.5434062319793185 ) ) ;
#29898 = ORIENTED_EDGE ( 'NONE', *, *, #17642, .T. ) ;
#29899 = CARTESIAN_POINT ( 'NONE',  ( -48.47912675150885065, -187.5000000000000284, 15.00000000000000711 ) ) ;
#29900 = ORIENTED_EDGE ( 'NONE', *, *, #37281, .F. ) ;
#29901 = ORIENTED_EDGE ( 'NONE', *, *, #13985, .F. ) ;
#29902 = CARTESIAN_POINT ( 'NONE',  ( 48.69345348225014192, -189.7472609257535510, -78.62880929222870918 ) ) ;
#29903 = AXIS2_PLACEMENT_3D ( 'NONE', #2767, #46411, #18034 ) ;
#29904 = CARTESIAN_POINT ( 'NONE',  ( -336.3521761649654422, -91.61526299123897843, -50.82679948493848343 ) ) ;
#29905 = VECTOR ( 'NONE', #19377, 1000.000000000000114 ) ;
#29906 = LINE ( 'NONE', #6781, #44846 ) ;
#29907 = DIRECTION ( 'NONE',  ( 0.000000000000000000, -0.000000000000000000, -1.000000000000000000 ) ) ;
#29908 = ORIENTED_EDGE ( 'NONE', *, *, #5028, .F. ) ;
#29909 = FACE_OUTER_BOUND ( 'NONE', #35593, .T. ) ;
#29910 = DIRECTION ( 'NONE',  ( 0.000000000000000000, 0.3546048870425396182, 0.9350162426854132791 ) ) ;
#29911 = AXIS2_PLACEMENT_3D ( 'NONE', #22353, #10786, #26546 ) ;
#29912 = ITEM_DEFINED_TRANSFORMATION ( 'NONE', 'NONE', #14173,  #31742 ) ;
#29913 = LINE ( 'NONE', #2051, #1972 ) ;
#29914 = FACE_OUTER_BOUND ( 'NONE', #32302, .T. ) ;
#29915 = ORIENTED_EDGE ( 'NONE', *, *, #2173, .F. ) ;
#29916 = DIRECTION ( 'NONE',  ( 0.000000000000000000, 0.000000000000000000, 1.000000000000000000 ) ) ;
#29917 = CARTESIAN_POINT ( 'NONE',  ( -47.50057025920934706, -189.7472609257535510, 0.2059786187411091207 ) ) ;
#29918 = FACE_OUTER_BOUND ( 'NONE', #8361, .T. ) ;
#29919 = ORIENTED_EDGE ( 'NONE', *, *, #16077, .F. ) ;
#29920 = VECTOR ( 'NONE', #14016, 1000.000000000000000 ) ;
#29921 = CIRCLE ( 'NONE', #14821, 60.00000000000000000 ) ;
#29922 = CARTESIAN_POINT ( 'NONE',  ( -101.0675409952200283, -177.1207230881787780, 113.3995532942340958 ) ) ;
#29923 = AXIS2_PLACEMENT_3D ( 'NONE', #17842, #13899, #13382 ) ;
#29924 = CIRCLE ( 'NONE', #9786, 125.0000000000000000 ) ;
#29925 = FACE_OUTER_BOUND ( 'NONE', #23506, .T. ) ;
#29926 = DIRECTION ( 'NONE',  ( 0.000000000000000000, 1.000000000000000000, 0.000000000000000000 ) ) ;
#29927 = ORIENTED_EDGE ( 'NONE', *, *, #4927, .T. ) ;
#29928 = EDGE_CURVE ( 'NONE', #46169, #38032, #5439, .T. ) ;
#29929 = EDGE_CURVE ( 'NONE', #33549, #18186, #23055, .T. ) ;
#29930 = CARTESIAN_POINT ( 'NONE',  ( -63.43218022845228887, -175.3837268820161057, 124.1024020384604540 ) ) ;
#29931 = VECTOR ( 'NONE', #16717, 1000.000000000000000 ) ;
#29932 = VERTEX_POINT ( 'NONE', #2460 ) ;
#29933 = CARTESIAN_POINT ( 'NONE',  ( -69.77312546433408613, -189.7472609257535510, 123.1729094355499967 ) ) ;
#29934 = FACE_OUTER_BOUND ( 'NONE', #42099, .T. ) ;
#29935 = CARTESIAN_POINT ( 'NONE',  ( -49.21696003055057389, -183.6283474603465606, -0.6749830015182127774 ) ) ;
#29936 = CARTESIAN_POINT ( 'NONE',  ( -336.3521761649654422, -145.9479049231020440, -54.58714071513102795 ) ) ;
#29937 = DIRECTION ( 'NONE',  ( 0.000000000000000000, 1.000000000000000000, -0.000000000000000000 ) ) ;
#29938 = ORIENTED_EDGE ( 'NONE', *, *, #29852, .F. ) ;
#29939 = DIRECTION ( 'NONE',  ( -0.000000000000000000, 1.000000000000000000, -0.000000000000000000 ) ) ;
#29940 = ORIENTED_EDGE ( 'NONE', *, *, #24208, .T. ) ;
#29941 = FACE_OUTER_BOUND ( 'NONE', #13349, .T. ) ;
#29942 = AXIS2_PLACEMENT_3D ( 'NONE', #20344, #8775, #28738 ) ;
#29943 = VECTOR ( 'NONE', #37413, 1000.000000000000000 ) ;
#29944 = EDGE_LOOP ( 'NONE', ( #43433, #20443, #12599, #1589 ) ) ;
#29945 = EDGE_CURVE ( 'NONE', #1430, #13839, #51086, .T. ) ;
#29946 = FACE_OUTER_BOUND ( 'NONE', #2377, .T. ) ;
#29947 = AXIS2_PLACEMENT_3D ( 'NONE', #18754, #14829, #18249 ) ;
#29948 = VERTEX_POINT ( 'NONE', #38183 ) ;
#29949 = ADVANCED_FACE ( 'NONE', ( #33986 ), #26100, .F. ) ;
#29950 = CARTESIAN_POINT ( 'NONE',  ( -34.51936650669028239, -175.3837268820161057, -124.2180546213278092 ) ) ;
#29951 = LINE ( 'NONE', #42034, #48282 ) ;
#29952 = EDGE_LOOP ( 'NONE', ( #24153, #30154, #24205, #23929 ) ) ;
#29955 = EDGE_LOOP ( 'NONE', ( #43591, #49287, #45468, #21341 ) ) ;
#29954 = LINE ( 'NONE', #17632, #44059 ) ;
#29953 = LINE ( 'NONE', #2612, #7397 ) ;
#29956 = VECTOR ( 'NONE', #33476, 1000.000000000000000 ) ;
#29957 = AXIS2_PLACEMENT_3D ( 'NONE', #2632, #26802, #18671 ) ;
#29958 = CIRCLE ( 'NONE', #9824, 125.0000000000000000 ) ;
#29959 = LINE ( 'NONE', #9476, #46635 ) ;
#29961 = ORIENTED_EDGE ( 'NONE', *, *, #39104, .T. ) ;
#29960 = VECTOR ( 'NONE', #14283, 1000.000000000000000 ) ;
#29962 = CARTESIAN_POINT ( 'NONE',  ( -23.99795575808071035, -183.6283474603465606, -122.5792489240757703 ) ) ;
#29963 = EDGE_LOOP ( 'NONE', ( #9620, #18362, #13781, #28406 ) ) ;
#29964 = EDGE_CURVE ( 'NONE', #41179, #38255, #22435, .T. ) ;
#29965 = CIRCLE ( 'NONE', #586, 125.0000000000000000 ) ;
#29966 = CARTESIAN_POINT ( 'NONE',  ( -336.3521761649653854, -175.8491356171901145, 29.31839013542587935 ) ) ;
#29969 = ORIENTED_EDGE ( 'NONE', *, *, #1149, .T. ) ;
#29968 = DIRECTION ( 'NONE',  ( -0.000000000000000000, 0.000000000000000000, -1.000000000000000000 ) ) ;
#29967 = DIRECTION ( 'NONE',  ( -0.000000000000000000, 1.000000000000000000, 0.000000000000000000 ) ) ;
#29970 = ORIENTED_EDGE ( 'NONE', *, *, #25944, .F. ) ;
#29971 = CIRCLE ( 'NONE', #37504, 125.0000000000000000 ) ;
#29972 = CARTESIAN_POINT ( 'NONE',  ( -86.93810158023210022, -177.1207230881787780, 117.8859915627477335 ) ) ;
#29973 = ORIENTED_EDGE ( 'NONE', *, *, #32778, .T. ) ;
#29974 = PLANE ( 'NONE',  #44664 ) ;
#29975 = DIRECTION ( 'NONE',  ( 0.000000000000000000, 0.3546048870425463906, 0.9350162426854107256 ) ) ;
#29976 = EDGE_LOOP ( 'NONE', ( #1964, #42052, #25635, #21741 ) ) ;
#29977 = PLANE ( 'NONE',  #45975 ) ;
#29978 = PRESENTATION_STYLE_ASSIGNMENT (( #13953 ) ) ;
#29979 = LINE ( 'NONE', #9750, #36038 ) ;
#29980 = CARTESIAN_POINT ( 'NONE',  ( -158.0280232639029236, -175.3837268820161057, 60.19999396110247147 ) ) ;
#29981 = ORIENTED_EDGE ( 'NONE', *, *, #8851, .T. ) ;
#29982 =( LENGTH_UNIT ( ) NAMED_UNIT ( * ) SI_UNIT ( .MILLI., .METRE. ) );
#29983 = CARTESIAN_POINT ( 'NONE',  ( -305.0000000000000568, -163.6602333390095509, 44.57752413668021774 ) ) ;
#29984 = FACE_OUTER_BOUND ( 'NONE', #51941, .T. ) ;
#29985 = EDGE_CURVE ( 'NONE', #21253, #17026, #46354, .T. ) ;
#29986 = CARTESIAN_POINT ( 'NONE',  ( 47.04848625005566731, -193.5000000000000000, 80.61932246194658092 ) ) ;
#29987 = ORIENTED_EDGE ( 'NONE', *, *, #286, .T. ) ;
#29988 = AXIS2_PLACEMENT_3D ( 'NONE', #22263, #29183, #38290 ) ;
#29989 = VECTOR ( 'NONE', #1354, 1000.000000000000114 ) ;
#29990 = LINE ( 'NONE', #10030, #16419 ) ;
#29991 = DIRECTION ( 'NONE',  ( 0.000000000000000000, 1.000000000000000000, 0.000000000000000000 ) ) ;
#29992 = VECTOR ( 'NONE', #36795, 1000.000000000000227 ) ;
#29993 = CARTESIAN_POINT ( 'NONE',  ( -96.65280530915691770, -183.6283474603465606, -115.3442529744087324 ) ) ;
#29994 = CARTESIAN_POINT ( 'NONE',  ( -180.0000000000000568, -123.5000000000000284, -37.63467731922663972 ) ) ;
#29995 = EDGE_CURVE ( 'NONE', #35424, #15652, #48233, .T. ) ;
#29996 = EDGE_CURVE ( 'NONE', #49741, #14193, #26870, .T. ) ;
#29997 = CARTESIAN_POINT ( 'NONE',  ( -151.5051191635538146, -177.1207230881787780, -69.00559874123518966 ) ) ;
#29998 = CIRCLE ( 'NONE', #9858, 125.0000000000000000 ) ;
#29999 = ADVANCED_FACE ( 'NONE', ( #30305 ), #38954, .F. ) ;
#30000 = AXIS2_PLACEMENT_3D ( 'NONE', #51049, #15040, #3699 ) ;
#30001 = DIRECTION ( 'NONE',  ( 0.000000000000000000, 0.000000000000000000, 1.000000000000000000 ) ) ;
#30002 = CARTESIAN_POINT ( 'NONE',  ( -159.0901268547125653, -193.5000000000000000, 58.22548115875957109 ) ) ;
#30003 = DIRECTION ( 'NONE',  ( 0.9473263538541876194, 0.000000000000000000, 0.3202698538628486746 ) ) ;
#30004 = AXIS2_PLACEMENT_3D ( 'NONE', #35641, #156, #3586 ) ;
#30005 = ORIENTED_EDGE ( 'NONE', *, *, #5701, .F. ) ;
#30006 = VECTOR ( 'NONE', #36769, 1000.000000000000000 ) ;
#30007 = AXIS2_PLACEMENT_3D ( 'NONE', #27812, #28069, #4185 ) ;
#30008 = DIRECTION ( 'NONE',  ( 0.000000000000000000, -0.6631226582407863113, 0.7485107481711089639 ) ) ;
#30010 = ORIENTED_EDGE ( 'NONE', *, *, #2477, .F. ) ;
#30009 = CARTESIAN_POINT ( 'NONE',  ( -154.0877180371535928, -175.3837268820161057, -66.87170886601927577 ) ) ;
#30011 = ORIENTED_EDGE ( 'NONE', *, *, #21388, .T. ) ;
#30012 = EDGE_LOOP ( 'NONE', ( #28218, #14556, #23718, #22755 ) ) ;
#30013 = ADVANCED_FACE ( 'NONE', ( #37936 ), #18485, .T. ) ;
#30014 = CARTESIAN_POINT ( 'NONE',  ( -49.13194886969936448, -175.3837268820161057, -0.7575112421616214675 ) ) ;
#30015 = DIRECTION ( 'NONE',  ( -0.9266896074318370369, 0.000000000000000000, 0.3758275821142292306 ) ) ;
#30016 = DIRECTION ( 'NONE',  ( -0.000000000000000000, -1.000000000000000000, 0.000000000000000000 ) ) ;
#30017 = ORIENTED_EDGE ( 'NONE', *, *, #22112, .T. ) ;
#30018 = DIRECTION ( 'NONE',  ( 0.000000000000000000, 1.000000000000000000, 0.000000000000000000 ) ) ;
#30019 = LINE ( 'NONE', #30791, #21869 ) ;
#30020 = AXIS2_PLACEMENT_3D ( 'NONE', #9546, #5879, #36887 ) ;
#30022 = ORIENTED_EDGE ( 'NONE', *, *, #14626, .T. ) ;
#30021 = CARTESIAN_POINT ( 'NONE',  ( 60.00000000000001421, -173.5000000000000284, 60.00000000000000000 ) ) ;
#30023 = AXIS2_PLACEMENT_3D ( 'NONE', #22608, #25770, #21835 ) ;
#30024 = DIRECTION ( 'NONE',  ( 0.000000000000000000, 1.000000000000000000, -0.000000000000000000 ) ) ;
#30025 = ORIENTED_EDGE ( 'NONE', *, *, #15598, .T. ) ;
#30026 = DIRECTION ( 'NONE',  ( 0.000000000000000000, 0.000000000000000000, 1.000000000000000000 ) ) ;
#30027 = VECTOR ( 'NONE', #9585, 1000.000000000000000 ) ;
#30028 = ORIENTED_EDGE ( 'NONE', *, *, #26972, .F. ) ;
#30029 = LINE ( 'NONE', #25557, #45924 ) ;
#30030 = DIRECTION ( 'NONE',  ( -0.000000000000000000, -0.8854560256532126861, -0.4647231720437631775 ) ) ;
#30031 = CARTESIAN_POINT ( 'NONE',  ( 60.00000000000000000, -93.50000000000002842, 51.54700538379266561 ) ) ;
#30032 = ORIENTED_EDGE ( 'NONE', *, *, #24630, .F. ) ;
#30033 = AXIS2_PLACEMENT_3D ( 'NONE', #12485, #8292, #51937 ) ;
#30034 = ORIENTED_EDGE ( 'NONE', *, *, #14472, .T. ) ;
#30035 = FACE_OUTER_BOUND ( 'NONE', #3893, .T. ) ;
#30036 = CARTESIAN_POINT ( 'NONE',  ( -336.3521761649654422, -67.40061919120938683, 18.46045550523129819 ) ) ;
#30037 = ORIENTED_EDGE ( 'NONE', *, *, #25103, .F. ) ;
#30038 = CARTESIAN_POINT ( 'NONE',  ( -165.2002711502080672, -183.6283474603465606, 44.73448837594995098 ) ) ;
#30039 = EDGE_CURVE ( 'NONE', #19848, #51884, #14551, .T. ) ;
#30040 = ORIENTED_EDGE ( 'NONE', *, *, #14390, .F. ) ;
#30041 = CARTESIAN_POINT ( 'NONE',  ( -336.3521761649654422, -78.25545813661345562, 37.90245108779119931 ) ) ;
#30042 = DIRECTION ( 'NONE',  ( -0.6528221181905174975, 0.000000000000000000, -0.7575112421616236880 ) ) ;
#30043 = AXIS2_PLACEMENT_3D ( 'NONE', #26780, #11001, #38862 ) ;
#30044 = ORIENTED_EDGE ( 'NONE', *, *, #33425, .F. ) ;
#30045 = CARTESIAN_POINT ( 'NONE',  ( 46.01898237923986557, -177.1207230881787780, -81.82363577055902226 ) ) ;
#30046 = ORIENTED_EDGE ( 'NONE', *, *, #28354, .F. ) ;
#30047 = CARTESIAN_POINT ( 'NONE',  ( -108.6269575285487576, -193.5000000000000000, -108.4360005853207127 ) ) ;
#30048 = LINE ( 'NONE', #8834, #42402 ) ;
#30049 = LINE ( 'NONE', #10591, #10973 ) ;
#30050 = VERTEX_POINT ( 'NONE', #14034 ) ;
#30051 = CARTESIAN_POINT ( 'NONE',  ( 72.31641062551800303, -189.7472609257535510, 32.14713283941989630 ) ) ;
#30052 = LINE ( 'NONE', #15848, #33142 ) ;
#30053 = DIRECTION ( 'NONE',  ( 0.000000000000000000, 0.3546048870425396182, 0.9350162426854132791 ) ) ;
#30054 = EDGE_CURVE ( 'NONE', #34274, #31867, #30052, .T. ) ;
#30055 = EDGE_CURVE ( 'NONE', #17649, #51370, #31333, .T. ) ;
#30056 = ORIENTED_EDGE ( 'NONE', *, *, #50136, .F. ) ;
#30057 = DIRECTION ( 'NONE',  ( 0.000000000000000000, 0.000000000000000000, 1.000000000000000000 ) ) ;
#30058 = VERTEX_POINT ( 'NONE', #23466 ) ;
#30059 = VECTOR ( 'NONE', #22415, 1000.000000000000000 ) ;
#30060 = CIRCLE ( 'NONE', #41808, 60.00000000000000000 ) ;
#30061 = ADVANCED_FACE ( 'NONE', ( #44205 ), #12396, .T. ) ;
#30062 = VECTOR ( 'NONE', #27863, 1000.000000000000000 ) ;
#30063 = DIRECTION ( 'NONE',  ( 0.000000000000000000, -0.000000000000000000, 1.000000000000000000 ) ) ;
#30065 = VERTEX_POINT ( 'NONE', #27389 ) ;
#30064 = LINE ( 'NONE', #42399, #15269 ) ;
#30066 = AXIS2_PLACEMENT_3D ( 'NONE', #48901, #21290, #1311 ) ;
#30067 = ORIENTED_EDGE ( 'NONE', *, *, #34317, .F. ) ;
#30068 = LINE ( 'NONE', #10350, #11485 ) ;
#30069 = FACE_OUTER_BOUND ( 'NONE', #18569, .T. ) ;
#30070 = VECTOR ( 'NONE', #42277, 1000.000000000000114 ) ;
#30071 = ORIENTED_EDGE ( 'NONE', *, *, #14983, .F. ) ;
#30072 = DIRECTION ( 'NONE',  ( 0.000000000000000000, 0.000000000000000000, -1.000000000000000000 ) ) ;
#30073 = EDGE_LOOP ( 'NONE', ( #24554, #10343, #43341, #20644 ) ) ;
#30074 = LINE ( 'NONE', #30851, #46002 ) ;
#30075 = CARTESIAN_POINT ( 'NONE',  ( 64.29733702426838704, -189.7472609257535510, 53.91167979418565182 ) ) ;
#30076 = CARTESIAN_POINT ( 'NONE',  ( -336.3521761649654422, -148.5878911270064009, 53.46519113769075204 ) ) ;
#30077 = DIRECTION ( 'NONE',  ( 1.000000000000000000, -0.000000000000000000, -0.000000000000000000 ) ) ;
#30078 = EDGE_LOOP ( 'NONE', ( #6548, #3641, #4079, #30010 ) ) ;
#30079 = VERTEX_POINT ( 'NONE', #11630 ) ;
#30080 = ORIENTED_EDGE ( 'NONE', *, *, #19214, .T. ) ;
#30081 = LINE ( 'NONE', #26128, #6489 ) ;
#30082 = DIRECTION ( 'NONE',  ( -0.9266896074318343723, 0.000000000000000000, 0.3758275821142357809 ) ) ;
#30083 = CARTESIAN_POINT ( 'NONE',  ( -48.47912675150885065, -175.3837268820161057, 6.938893903907228378E-15 ) ) ;
#30084 = CARTESIAN_POINT ( 'NONE',  ( -48.47912675150885065, -175.3837268820161057, 6.938893903907228378E-15 ) ) ;
#30085 = ORIENTED_EDGE ( 'NONE', *, *, #39317, .T. ) ;
#30086 = VERTEX_POINT ( 'NONE', #39982 ) ;
#30088 = ORIENTED_EDGE ( 'NONE', *, *, #49642, .F. ) ;
#30087 = DIRECTION ( 'NONE',  ( -0.2348860457809707758, 0.000000000000000000, -0.9720229140804138579 ) ) ;
#30089 = ORIENTED_EDGE ( 'NONE', *, *, #15406, .T. ) ;
#30090 = AXIS2_PLACEMENT_3D ( 'NONE', #51903, #4062, #28468 ) ;
#30091 = DIRECTION ( 'NONE',  ( 0.000000000000000000, 0.000000000000000000, -1.000000000000000000 ) ) ;
#30093 = AXIS2_PLACEMENT_3D ( 'NONE', #4170, #7583, #19931 ) ;
#30092 = PLANE ( 'NONE',  #45120 ) ;
#30094 = CARTESIAN_POINT ( 'NONE',  ( -330.4913330509368166, -157.4273119900852578, -48.27201571436002325 ) ) ;
#30095 = AXIS2_PLACEMENT_3D ( 'NONE', #20705, #9148, #45163 ) ;
#30096 = EDGE_CURVE ( 'NONE', #39429, #40001, #23090, .T. ) ;
#30097 = CARTESIAN_POINT ( 'NONE',  ( -339.1964088526558498, -168.7406467949209059, -39.41172259083857909 ) ) ;
#30098 = ADVANCED_FACE ( 'NONE', ( #27905 ), #47648, .T. ) ;
#30099 = EDGE_CURVE ( 'NONE', #51271, #1772, #35793, .T. ) ;
#30100 = DIRECTION ( 'NONE',  ( -1.000000000000000000, 0.000000000000000000, 0.000000000000000000 ) ) ;
#30101 = ORIENTED_EDGE ( 'NONE', *, *, #23406, .T. ) ;
#30102 = LINE ( 'NONE', #46149, #20879 ) ;
#30103 = ORIENTED_EDGE ( 'NONE', *, *, #7951, .F. ) ;
#30104 = EDGE_CURVE ( 'NONE', #9410, #3078, #23711, .T. ) ;
#30105 = ORIENTED_EDGE ( 'NONE', *, *, #48841, .F. ) ;
#30106 = DIRECTION ( 'NONE',  ( 0.9982437317643217956, 0.000000000000000000, -0.05924062789370748011 ) ) ;
#30107 = AXIS2_PLACEMENT_3D ( 'NONE', #10688, #22777, #38786 ) ;
#30108 = EDGE_CURVE ( 'NONE', #41848, #20319, #43941, .T. ) ;
#30109 = DIRECTION ( 'NONE',  ( 0.000000000000000000, 0.000000000000000000, -1.000000000000000000 ) ) ;
#30110 = ORIENTED_EDGE ( 'NONE', *, *, #13550, .T. ) ;
#30111 = EDGE_CURVE ( 'NONE', #18537, #17442, #36057, .T. ) ;
#30112 = CARTESIAN_POINT ( 'NONE',  ( 15.80042947435468470, -175.3837268820161057, 107.2060569716377927 ) ) ;
#30113 = DIRECTION ( 'NONE',  ( 0.000000000000000000, 0.000000000000000000, 1.000000000000000000 ) ) ;
#30114 = CARTESIAN_POINT ( 'NONE',  ( -130.7087404384255080, -193.5000000000000000, -94.14505102712755047 ) ) ;
#30115 = EDGE_CURVE ( 'NONE', #9866, #2431, #43164, .T. ) ;
#30116 = FACE_OUTER_BOUND ( 'NONE', #31189, .T. ) ;
#30117 = EDGE_CURVE ( 'NONE', #13092, #47587, #47896, .T. ) ;
#30118 = VECTOR ( 'NONE', #49881, 1000.000000000000000 ) ;
#30119 = CARTESIAN_POINT ( 'NONE',  ( 71.87891646118019651, -189.7472609257535510, -33.74820638215423685 ) ) ;
#30120 = ORIENTED_EDGE ( 'NONE', *, *, #22749, .F. ) ;
#30121 = EDGE_CURVE ( 'NONE', #30483, #40790, #24237, .T. ) ;
#30122 = DIRECTION ( 'NONE',  ( -0.000000000000000000, 1.000000000000000000, -0.000000000000000000 ) ) ;
#30123 = VERTEX_POINT ( 'NONE', #11871 ) ;
#30124 = ADVANCED_FACE ( 'NONE', ( #15577 ), #7931, .T. ) ;
#30125 = ORIENTED_EDGE ( 'NONE', *, *, #906, .F. ) ;
#30126 = FACE_OUTER_BOUND ( 'NONE', #923, .T. ) ;
#30127 = ORIENTED_EDGE ( 'NONE', *, *, #11823, .T. ) ;
#30128 = CARTESIAN_POINT ( 'NONE',  ( -330.4913330509368166, -78.25935320507949200, -39.41172259083896279 ) ) ;
#30129 = VECTOR ( 'NONE', #17607, 1000.000000000000227 ) ;
#30130 = CARTESIAN_POINT ( 'NONE',  ( -339.1964088526558498, -123.5000000000000284, 0.000000000000000000 ) ) ;
#30132 = VERTEX_POINT ( 'NONE', #56 ) ;
#30131 = CARTESIAN_POINT ( 'NONE',  ( -339.1964088526558498, -157.1712093821534211, -49.66134974749665076 ) ) ;
#30133 = DIRECTION ( 'NONE',  ( 0.000000000000000000, -0.000000000000000000, 1.000000000000000000 ) ) ;
#30134 = VECTOR ( 'NONE', #21882, 1000.000000000000000 ) ;
#30135 = FACE_OUTER_BOUND ( 'NONE', #46369, .T. ) ;
#30136 = PLANE ( 'NONE',  #23183 ) ;
#30137 = EDGE_CURVE ( 'NONE', #6231, #25260, #15522, .T. ) ;
#30138 = ORIENTED_EDGE ( 'NONE', *, *, #36577, .T. ) ;
#30139 = ORIENTED_EDGE ( 'NONE', *, *, #43704, .T. ) ;
#30140 = ORIENTED_EDGE ( 'NONE', *, *, #22506, .F. ) ;
#30141 = DIRECTION ( 'NONE',  ( 0.000000000000000000, 1.000000000000000000, -0.000000000000000000 ) ) ;
#30142 = VECTOR ( 'NONE', #46174, 1000.000000000000227 ) ;
#30143 = CARTESIAN_POINT ( 'NONE',  ( -336.3521761649654422, -154.8494888031386836, 50.05135858667791382 ) ) ;
#30144 = CARTESIAN_POINT ( 'NONE',  ( 74.77174840718836890, -183.6283474603465606, 20.83798868929603643 ) ) ;
#30145 = LINE ( 'NONE', #1766, #6869 ) ;
#30146 = CARTESIAN_POINT ( 'NONE',  ( -330.4913330509368166, -180.9052250602809693, -13.63415328425256945 ) ) ;
#30147 = ORIENTED_EDGE ( 'NONE', *, *, #48637, .F. ) ;
#30148 = AXIS2_PLACEMENT_3D ( 'NONE', #45628, #13816, #34043 ) ;
#30149 = CARTESIAN_POINT ( 'NONE',  ( 48.06131630543706734, -193.5000000000000000, -79.40367028273054473 ) ) ;
#30150 = EDGE_CURVE ( 'NONE', #10649, #51653, #7170, .T. ) ;
#30151 = EDGE_LOOP ( 'NONE', ( #42440, #14410, #13848, #33230 ) ) ;
#30153 = ORIENTED_EDGE ( 'NONE', *, *, #25321, .F. ) ;
#30152 = CARTESIAN_POINT ( 'NONE',  ( -330.4913330509368166, -138.1050951016791544, -57.16590939599326049 ) ) ;
#30154 = ORIENTED_EDGE ( 'NONE', *, *, #41666, .F. ) ;
#30155 = DIRECTION ( 'NONE',  ( 0.000000000000000000, -1.000000000000000000, 0.000000000000000000 ) ) ;
#30156 = ORIENTED_EDGE ( 'NONE', *, *, #43929, .T. ) ;
#30157 = DIRECTION ( 'NONE',  ( 0.9027978299657387629, 0.000000000000000000, 0.4300652022765304450 ) ) ;
#30158 = VERTEX_POINT ( 'NONE', #28157 ) ;
#30159 = EDGE_CURVE ( 'NONE', #28018, #34611, #3760, .T. ) ;
#30160 = ADVANCED_FACE ( 'NONE', ( #3236 ), #19272, .T. ) ;
#30161 = CARTESIAN_POINT ( 'NONE',  ( 11.52087324849114580, -132.5479369270331915, -186.7953921478704729 ) ) ;
#30162 = EDGE_CURVE ( 'NONE', #3300, #10662, #574, .T. ) ;
#30163 = EDGE_CURVE ( 'NONE', #7450, #5492, #44999, .T. ) ;
#30164 = CARTESIAN_POINT ( 'NONE',  ( 3.686287386450715076E-15, 20.00000000000000000, -46.00000000000000711 ) ) ;
#30165 = EDGE_LOOP ( 'NONE', ( #26124, #49723, #23756, #4563 ) ) ;
#30166 = FACE_OUTER_BOUND ( 'NONE', #43696, .T. ) ;
#30167 = VERTEX_POINT ( 'NONE', #12914 ) ;
#30168 = EDGE_CURVE ( 'NONE', #17256, #14634, #10477, .T. ) ;
#30169 = VERTEX_POINT ( 'NONE', #17845 ) ;
#30170 = DIRECTION ( 'NONE',  ( 0.3482016354343995812, 0.000000000000000000, -0.9374196611341205632 ) ) ;
#30171 = DIRECTION ( 'NONE',  ( 0.000000000000000000, -1.000000000000000000, 1.047444401652940007E-14 ) ) ;
#30172 = AXIS2_PLACEMENT_3D ( 'NONE', #13329, #34068, #45917 ) ;
#30173 = ADVANCED_FACE ( 'NONE', ( #8716, #36571 ), #8988, .T. ) ;
#30174 = ADVANCED_FACE ( 'NONE', ( #25983 ), #18370, .T. ) ;
#30175 = CARTESIAN_POINT ( 'NONE',  ( 62.43652093785069468, -177.1207230881787780, 55.44293326708522329 ) ) ;
#30176 = DIRECTION ( 'NONE',  ( -0.2635871660690783380, 0.000000000000000000, 0.9646355819083558547 ) ) ;
#30177 = EDGE_LOOP ( 'NONE', ( #39884, #28103, #29164, #45208 ) ) ;
#30178 = FACE_OUTER_BOUND ( 'NONE', #24094, .T. ) ;
#30179 = CIRCLE ( 'NONE', #25156, 125.0000000000000000 ) ;
#30180 = LINE ( 'NONE', #22562, #2113 ) ;
#30181 = CONTEXT_DEPENDENT_SHAPE_REPRESENTATION ( #26976, #37316 ) ;
#30182 = FACE_OUTER_BOUND ( 'NONE', #50770, .T. ) ;
#30183 = CARTESIAN_POINT ( 'NONE',  ( -332.3517673607765914, -171.3361784870343740, 36.21739951675979086 ) ) ;
#30184 = EDGE_CURVE ( 'NONE', #12871, #48304, #51602, .T. ) ;
#30185 = ORIENTED_EDGE ( 'NONE', *, *, #20427, .T. ) ;
#30186 = CARTESIAN_POINT ( 'NONE',  ( -65.47874029382339245, -193.5000000000000000, 122.8300162461137006 ) ) ;
#30187 = DIRECTION ( 'NONE',  ( 0.000000000000000000, 0.000000000000000000, -1.000000000000000000 ) ) ;
#30188 = EDGE_CURVE ( 'NONE', #25229, #38006, #16627, .T. ) ;
#30189 = CARTESIAN_POINT ( 'NONE',  ( -330.4913330509368166, -71.02573290043841325, 26.97593913775512320 ) ) ;
#30190 = VERTEX_POINT ( 'NONE', #29922 ) ;
#30191 = EDGE_CURVE ( 'NONE', #17270, #47175, #28674, .T. ) ;
#30192 = DIRECTION ( 'NONE',  ( 0.000000000000000000, 0.000000000000000000, 1.000000000000000000 ) ) ;
#30193 = FACE_BOUND ( 'NONE', #8412, .T. ) ;
#30194 = ADVANCED_FACE ( 'NONE', ( #24752 ), #9971, .T. ) ;
#30195 = ORIENTED_EDGE ( 'NONE', *, *, #6041, .T. ) ;
#30196 = DIRECTION ( 'NONE',  ( -0.000000000000000000, 1.000000000000000000, -0.000000000000000000 ) ) ;
#30197 = EDGE_LOOP ( 'NONE', ( #45676, #1221, #10417, #47601 ) ) ;
#30198 = ADVANCED_FACE ( 'NONE', ( #26225 ), #4789, .T. ) ;
#30199 = VECTOR ( 'NONE', #2548, 1000.000000000000000 ) ;
#30200 = CARTESIAN_POINT ( 'NONE',  ( -123.4791267515088435, -198.5000000000000000, 60.00000000000001421 ) ) ;
#30201 = DIRECTION ( 'NONE',  ( 1.000000000000000000, 0.000000000000000000, 0.000000000000000000 ) ) ;
#30202 = CARTESIAN_POINT ( 'NONE',  ( -169.8550585387150136, -189.7472609257535510, 25.37485791684378711 ) ) ;
#30203 = DIRECTION ( 'NONE',  ( -0.000000000000000000, 1.000000000000000000, 0.000000000000000000 ) ) ;
#30204 = CARTESIAN_POINT ( 'NONE',  ( -48.47912675150885065, -189.7472609257535510, 6.938893903907228378E-15 ) ) ;
#30205 = ORIENTED_EDGE ( 'NONE', *, *, #45781, .T. ) ;
#30207 = EDGE_CURVE ( 'NONE', #40028, #15743, #12985, .T. ) ;
#30206 = CYLINDRICAL_SURFACE ( 'NONE', #17257, 125.0000000000000000 ) ;
#30208 = ORIENTED_EDGE ( 'NONE', *, *, #51138, .F. ) ;
#30209 = CYLINDRICAL_SURFACE ( 'NONE', #10749, 124.9999999999999858 ) ;
#30210 = VECTOR ( 'NONE', #13651, 1000.000000000000114 ) ;
#30211 = ORIENTED_EDGE ( 'NONE', *, *, #21136, .F. ) ;
#30212 = DIRECTION ( 'NONE',  ( -0.000000000000000000, -1.000000000000000000, -0.000000000000000000 ) ) ;
#30213 = DIRECTION ( 'NONE',  ( 0.000000000000000000, 0.7485107481710953081, -0.6631226582408016323 ) ) ;
#30214 = PRODUCT ( 'bin', 'bin', '', ( #29132 ) ) ;
#30215 = DIRECTION ( 'NONE',  ( 1.000000000000000000, 0.000000000000000000, 0.000000000000000000 ) ) ;
#30216 = VERTEX_POINT ( 'NONE', #48935 ) ;
#30219 = VERTEX_POINT ( 'NONE', #34129 ) ;
#30218 = CARTESIAN_POINT ( 'NONE',  ( -336.3521761649654422, -170.5607375887735770, 35.68215131113770155 ) ) ;
#30217 = DIRECTION ( 'NONE',  ( 0.9785564922995046988, 0.000000000000000000, -0.2059786187410953262 ) ) ;
#30220 = CARTESIAN_POINT ( 'NONE',  ( -332.3517673607765914, -173.5513585866778214, -31.34948880313881503 ) ) ;
#30221 = EDGE_LOOP ( 'NONE', ( #27674, #41960, #19482, #51172 ) ) ;
#30222 = LINE ( 'NONE', #14712, #44014 ) ;
#30223 = EDGE_LOOP ( 'NONE', ( #4000, #33058, #30540, #26762 ) ) ;
#30224 = ADVANCED_FACE ( 'NONE', ( #28938 ), #40505, .F. ) ;
#30225 = EDGE_CURVE ( 'NONE', #25185, #18665, #37804, .T. ) ;
#30226 = CARTESIAN_POINT ( 'NONE',  ( -336.3521761649654422, -123.5000000000000284, 0.000000000000000000 ) ) ;
#30229 = EDGE_LOOP ( 'NONE', ( #21994, #16093, #27460, #51212 ) ) ;
#30228 = CARTESIAN_POINT ( 'NONE',  ( 0.000000000000000000, 20.00000000000000355, 0.000000000000000000 ) ) ;
#30227 = DIRECTION ( 'NONE',  ( 0.000000000000000000, 0.000000000000000000, 1.000000000000000000 ) ) ;
#30230 = EDGE_LOOP ( 'NONE', ( #37329, #16120, #29371, #49137 ) ) ;
#30231 = AXIS2_PLACEMENT_3D ( 'NONE', #31364, #47406, #27419 ) ;
#30232 = AXIS2_PLACEMENT_3D ( 'NONE', #14886, #34565, #30898 ) ;
#30233 = CARTESIAN_POINT ( 'NONE',  ( -48.47912675150885065, -188.5000000000000284, 6.938893903907228378E-15 ) ) ;
#30234 = VERTEX_POINT ( 'NONE', #6276 ) ;
#30235 = CARTESIAN_POINT ( 'NONE',  ( -332.3517673607765914, -68.91285928486892942, -22.44790492310182017 ) ) ;
#30236 = DIRECTION ( 'NONE',  ( 0.000000000000000000, 1.000000000000000000, 0.000000000000000000 ) ) ;
#30237 = EDGE_LOOP ( 'NONE', ( #25363, #4585, #6715, #42737 ) ) ;
#30238 = LINE ( 'NONE', #46792, #38121 ) ;
#30239 = DIRECTION ( 'NONE',  ( 0.4566292373937140270, 0.000000000000000000, -0.8896570909947467687 ) ) ;
#30240 = LINE ( 'NONE', #50481, #9821 ) ;
#30241 = DIRECTION ( 'NONE',  ( 0.000000000000000000, -0.7485107481710999711, 0.6631226582407964143 ) ) ;
#30242 = CARTESIAN_POINT ( 'NONE',  ( 64.29733702426838704, -189.7472609257535510, 53.91167979418565182 ) ) ;
#30243 = ORIENTED_EDGE ( 'NONE', *, *, #20417, .T. ) ;
#30244 = DIRECTION ( 'NONE',  ( 0.4827922027307366970, 0.000000000000000000, 0.8757349421956412971 ) ) ;
#30245 = PLANE ( 'NONE',  #41563 ) ;
#30246 = FACE_OUTER_BOUND ( 'NONE', #1241, .T. ) ;
#30247 = EDGE_LOOP ( 'NONE', ( #24104, #48172, #12620, #39631 ) ) ;
#30248 = VECTOR ( 'NONE', #5968, 1000.000000000000000 ) ;
#30249 = DIRECTION ( 'NONE',  ( 0.000000000000000000, 0.000000000000000000, -1.000000000000000000 ) ) ;
#30250 = LINE ( 'NONE', #34192, #10146 ) ;
#30251 = EDGE_CURVE ( 'NONE', #1515, #35357, #43227, .T. ) ;
#30252 = FACE_OUTER_BOUND ( 'NONE', #29976, .T. ) ;
#30253 = DIRECTION ( 'NONE',  ( 0.000000000000000000, 0.000000000000000000, -1.000000000000000000 ) ) ;
#30254 = ADVANCED_FACE ( 'NONE', ( #8455 ), #24483, .T. ) ;
#30255 = CARTESIAN_POINT ( 'NONE',  ( 48.66843973345087448, 30.00000000000000355, -40.95752564483601788 ) ) ;
#30256 = DIRECTION ( 'NONE',  ( 0.000000000000000000, -0.000000000000000000, 1.000000000000000000 ) ) ;
#30257 = CARTESIAN_POINT ( 'NONE',  ( 14.37129481273060172, -189.7472609257535510, -108.0501018472328099 ) ) ;
#30258 = DIRECTION ( 'NONE',  ( -0.8896570909947467687, 0.000000000000000000, -0.4566292373937140270 ) ) ;
#30259 = VERTEX_POINT ( 'NONE', #2588 ) ;
#30260 = CARTESIAN_POINT ( 'NONE',  ( -336.3521761649654422, -80.42027357919624819, -40.34602258462219027 ) ) ;
#30261 = VECTOR ( 'NONE', #10305, 1000.000000000000000 ) ;
#30262 = AXIS2_PLACEMENT_3D ( 'NONE', #9505, #32366, #48678 ) ;
#30263 = DIRECTION ( 'NONE',  ( 0.000000000000000000, 1.000000000000000000, 0.000000000000000000 ) ) ;
#30265 = ORIENTED_EDGE ( 'NONE', *, *, #28901, .T. ) ;
#30264 = DIRECTION ( 'NONE',  ( 0.8455960035018234011, 0.000000000000000000, 0.5338233779647948429 ) ) ;
#30266 = VERTEX_POINT ( 'NONE', #14952 ) ;
#30267 = EDGE_LOOP ( 'NONE', ( #49223, #32215, #22336, #19987 ) ) ;
#30268 = PLANE ( 'NONE',  #6598 ) ;
#30269 = FACE_OUTER_BOUND ( 'NONE', #43284, .T. ) ;
#30270 = CARTESIAN_POINT ( 'NONE',  ( -18.95304271317703382, -193.5000000000000000, -121.4627941443854837 ) ) ;
#30271 = VERTEX_POINT ( 'NONE', #38584 ) ;
#30272 = CARTESIAN_POINT ( 'NONE',  ( -336.3521761649654422, -123.5000000000000284, 0.000000000000000000 ) ) ;
#30273 = CARTESIAN_POINT ( 'NONE',  ( -48.07600332222088468, -175.3837268820161057, 0.9151456172430280089 ) ) ;
#30276 = VERTEX_POINT ( 'NONE', #34633 ) ;
#30275 = DIRECTION ( 'NONE',  ( -0.000000000000000000, 1.000000000000000000, -0.000000000000000000 ) ) ;
#30274 = DIRECTION ( 'NONE',  ( 0.000000000000000000, 1.000000000000000000, -0.000000000000000000 ) ) ;
#30277 = AXIS2_PLACEMENT_3D ( 'NONE', #36667, #40855, #8029 ) ;
#30278 = PLANE ( 'NONE',  #44068 ) ;
#30279 = VERTEX_POINT ( 'NONE', #18620 ) ;
#30280 = LINE ( 'NONE', #26847, #22189 ) ;
#30281 = VERTEX_POINT ( 'NONE', #18863 ) ;
#30282 = EDGE_CURVE ( 'NONE', #19235, #51805, #30685, .T. ) ;
#30283 = CARTESIAN_POINT ( 'NONE',  ( -120.5074237604784315, -183.6283474603465606, 100.9358816284415923 ) ) ;
#30284 = CARTESIAN_POINT ( 'NONE',  ( 75.78974234412359579, -183.6283474603465606, 13.49993235881449394 ) ) ;
#30285 = DIRECTION ( 'NONE',  ( 0.000000000000000000, -0.9927088740980535286, 0.1205366802553268502 ) ) ;
#30286 = EDGE_LOOP ( 'NONE', ( #14218, #6730, #35705, #37050 ) ) ;
#30287 = DIRECTION ( 'NONE',  ( 0.2920567706369628924, 0.000000000000000000, 0.9564009842765264224 ) ) ;
#30288 = CARTESIAN_POINT ( 'NONE',  ( -339.1964088526558498, -74.40671499923440990, -34.49419324804689779 ) ) ;
#30289 = VERTEX_POINT ( 'NONE', #47262 ) ;
#30290 = CARTESIAN_POINT ( 'NONE',  ( -102.0975050429524771, -193.5000000000000000, -111.8087531435654114 ) ) ;
#30291 = VECTOR ( 'NONE', #6607, 1000.000000000000000 ) ;
#30292 = LINE ( 'NONE', #11086, #6408 ) ;
#30293 = ORIENTED_EDGE ( 'NONE', *, *, #7208, .T. ) ;
#30294 = CARTESIAN_POINT ( 'NONE',  ( -340.0000000000000568, -78.50000000000002842, 0.000000000000000000 ) ) ;
#30295 = DIRECTION ( 'NONE',  ( 0.5829794791144650157, 0.000000000000000000, 0.8124868780056864193 ) ) ;
#30296 = AXIS2_PLACEMENT_3D ( 'NONE', #2341, #21535, #10461 ) ;
#30297 = ORIENTED_EDGE ( 'NONE', *, *, #4412, .F. ) ;
#30298 = LINE ( 'NONE', #50291, #29960 ) ;
#30299 = ORIENTED_EDGE ( 'NONE', *, *, #40850, .F. ) ;
#30300 = DIRECTION ( 'NONE',  ( 0.000000000000000000, -1.000000000000000000, 0.000000000000000000 ) ) ;
#30301 = LINE ( 'NONE', #17719, #21901 ) ;
#30302 = EDGE_CURVE ( 'NONE', #14589, #1636, #46743, .T. ) ;
#30303 = ORIENTED_EDGE ( 'NONE', *, *, #44246, .F. ) ;
#30304 = DIRECTION ( 'NONE',  ( 1.000000000000000000, -0.000000000000000000, -0.000000000000000000 ) ) ;
#30305 = FACE_OUTER_BOUND ( 'NONE', #51971, .T. ) ;
#30306 = CARTESIAN_POINT ( 'NONE',  ( -48.47912675150885065, -189.7472609257535510, 6.938893903907228378E-15 ) ) ;
#30307 = ORIENTED_EDGE ( 'NONE', *, *, #42309, .T. ) ;
#30308 = CARTESIAN_POINT ( 'NONE',  ( -47.48307690889363641, -183.6283474603465606, 0.08879589532294547560 ) ) ;
#30309 = VERTEX_POINT ( 'NONE', #39085 ) ;
#30310 = VECTOR ( 'NONE', #5599, 1000.000000000000000 ) ;
#30311 = LINE ( 'NONE', #6158, #19406 ) ;
#30312 = DIRECTION ( 'NONE',  ( 0.000000000000000000, 5.319818659662208160E-15, -1.000000000000000000 ) ) ;
#30314 = ORIENTED_EDGE ( 'NONE', *, *, #34960, .F. ) ;
#30313 = CARTESIAN_POINT ( 'NONE',  ( -332.3517673607765914, -63.52220716707010695, -1.632288850093980725 ) ) ;
#30315 = VERTEX_POINT ( 'NONE', #10732 ) ;
#30316 = CARTESIAN_POINT ( 'NONE',  ( -339.1964088526558498, -64.86990808808704401, 6.615309698014191220 ) ) ;
#30317 = CARTESIAN_POINT ( 'NONE',  ( -59.86929868745821182, -177.1207230881787780, -124.4799742258549600 ) ) ;
#30318 = ORIENTED_EDGE ( 'NONE', *, *, #47325, .F. ) ;
#30319 = DIRECTION ( 'NONE',  ( -0.000000000000000000, -1.000000000000000000, 0.000000000000000000 ) ) ;
#30320 = VERTEX_POINT ( 'NONE', #50949 ) ;
#30321 = DIRECTION ( 'NONE',  ( 0.000000000000000000, -1.000000000000000000, 0.000000000000000000 ) ) ;
#30322 = CARTESIAN_POINT ( 'NONE',  ( 48.06131630543706734, -193.5000000000000000, -79.40367028273054473 ) ) ;
#30323 = AXIS2_PLACEMENT_3D ( 'NONE', #44008, #40055, #48222 ) ;
#30324 = AXIS2_PLACEMENT_3D ( 'NONE', #47452, #8017, #24053 ) ;
#30325 = EDGE_CURVE ( 'NONE', #40382, #14358, #38835, .T. ) ;
#30326 = DIRECTION ( 'NONE',  ( 0.000000000000000000, 1.000000000000000000, 0.000000000000000000 ) ) ;
#30327 = ORIENTED_EDGE ( 'NONE', *, *, #43847, .F. ) ;
#30328 = ORIENTED_EDGE ( 'NONE', *, *, #31088, .F. ) ;
#30330 = ORIENTED_EDGE ( 'NONE', *, *, #27458, .T. ) ;
#30329 = CIRCLE ( 'NONE', #7676, 60.00000000000000000 ) ;
#30331 = EDGE_CURVE ( 'NONE', #50673, #45478, #41538, .T. ) ;
#30332 = CARTESIAN_POINT ( 'NONE',  ( -330.4913330509368166, -64.99044476834247064, -7.608018572113060429 ) ) ;
#30333 = DIRECTION ( 'NONE',  ( 0.000000000000000000, 0.000000000000000000, -1.000000000000000000 ) ) ;
#30334 = DIRECTION ( 'NONE',  ( -0.4827922027307551267, 0.000000000000000000, 0.8757349421956311941 ) ) ;
#30335 = LINE ( 'NONE', #34027, #20502 ) ;
#30336 = EDGE_LOOP ( 'NONE', ( #21221, #18761, #21371, #37957 ) ) ;
#30337 = EDGE_CURVE ( 'NONE', #30190, #4219, #20531, .T. ) ;
#30338 = PLANE ( 'NONE',  #6386 ) ;
#30339 = AXIS2_PLACEMENT_3D ( 'NONE', #20226, #43876, #51786 ) ;
#30340 = EDGE_CURVE ( 'NONE', #40028, #787, #26756, .T. ) ;
#30341 = EDGE_LOOP ( 'NONE', ( #20749, #10882, #14892, #324 ) ) ;
#30342 = EDGE_LOOP ( 'NONE', ( #23222, #49544, #33460, #36661 ) ) ;
#30343 = CARTESIAN_POINT ( 'NONE',  ( -47.64924157374594671, -189.7472609257535510, 124.9972451320097377 ) ) ;
#30344 = EDGE_CURVE ( 'NONE', #33832, #18089, #33961, .T. ) ;
#30345 = VECTOR ( 'NONE', #14639, 1000.000000000000000 ) ;
#30346 = DIRECTION ( 'NONE',  ( -0.000000000000000000, 1.000000000000000000, 0.000000000000000000 ) ) ;
#30347 = LINE ( 'NONE', #46395, #28333 ) ;
#30348 = CARTESIAN_POINT ( 'NONE',  ( -167.1580984288390823, -189.7472609257535510, -39.24667733211878584 ) ) ;
#30349 = DIRECTION ( 'NONE',  ( 0.000000000000000000, 0.000000000000000000, -1.000000000000000000 ) ) ;
#30350 = EDGE_LOOP ( 'NONE', ( #37261, #35999, #40184, #46406 ) ) ;
#30351 = CARTESIAN_POINT ( 'NONE',  ( -92.78132261338706144, -189.7472609257535510, -116.8859077982276631 ) ) ;
#30352 = APPLICATION_CONTEXT ( 'automotive_design' ) ;
#30353 = ORIENTED_EDGE ( 'NONE', *, *, #25830, .F. ) ;
#30354 = DIRECTION ( 'NONE',  ( -0.000000000000000000, 0.7485107481711089639, 0.6631226582407863113 ) ) ;
#30355 = DIRECTION ( 'NONE',  ( 0.000000000000000000, -1.000000000000000000, 0.000000000000000000 ) ) ;
#30356 = EDGE_CURVE ( 'NONE', #19079, #50975, #14425, .T. ) ;
#30357 = ORIENTED_EDGE ( 'NONE', *, *, #18425, .T. ) ;
#30358 = VECTOR ( 'NONE', #28404, 1000.000000000000000 ) ;
#30359 = CARTESIAN_POINT ( 'NONE',  ( -101.9736325116273576, -183.6283474603465606, 112.9749434763330527 ) ) ;
#30360 = CARTESIAN_POINT ( 'NONE',  ( -81.70897914701313880, -177.1207230881787780, -120.5021863277716534 ) ) ;
#30361 = DIRECTION ( 'NONE',  ( 0.000000000000000000, 1.000000000000000000, 0.000000000000000000 ) ) ;
#30362 = VECTOR ( 'NONE', #12524, 999.9999999999998863 ) ;
#30363 = CIRCLE ( 'NONE', #17779, 125.0000000000000000 ) ;
#30364 = ORIENTED_EDGE ( 'NONE', *, *, #34592, .F. ) ;
#30365 = CARTESIAN_POINT ( 'NONE',  ( -49.46816693883101834, -193.5000000000000000, 0.1476465640024780257 ) ) ;
#30366 = ORIENTED_EDGE ( 'NONE', *, *, #10244, .F. ) ;
#30367 = VERTEX_POINT ( 'NONE', #30431 ) ;
#30368 = FACE_OUTER_BOUND ( 'NONE', #9282, .T. ) ;
#30369 = EDGE_LOOP ( 'NONE', ( #37554, #36549, #42960, #27485 ) ) ;
#30370 = AXIS2_PLACEMENT_3D ( 'NONE', #32641, #36317, #24758 ) ;
#30371 = CARTESIAN_POINT ( 'NONE',  ( -170.0000000000000284, -123.5000000000000284, 15.24495751795539000 ) ) ;
#30372 = VECTOR ( 'NONE', #22125, 1000.000000000000000 ) ;
#30373 = CIRCLE ( 'NONE', #17831, 125.0000000000000000 ) ;
#30374 = ORIENTED_EDGE ( 'NONE', *, *, #7672, .T. ) ;
#30375 = LINE ( 'NONE', #38004, #30142 ) ;
#30376 = DIRECTION ( 'NONE',  ( -0.9027978299657477557, 0.000000000000000000, 0.4300652022765115712 ) ) ;
#30377 = VERTEX_POINT ( 'NONE', #27006 ) ;
#30378 = DIRECTION ( 'NONE',  ( -0.9995608365087944591, 0.000000000000000000, 0.02963332782255633305 ) ) ;
#30379 = EDGE_CURVE ( 'NONE', #26602, #38101, #43563, .T. ) ;
#30380 = EDGE_CURVE ( 'NONE', #10133, #47358, #30959, .T. ) ;
#30381 = CARTESIAN_POINT ( 'NONE',  ( -336.3521761649653854, -100.7053649598255163, 55.50139289590170222 ) ) ;
#30382 = CARTESIAN_POINT ( 'NONE',  ( 65.38692482895591240, -193.5000000000000000, -51.57055649762701677 ) ) ;
#30383 = ORIENTED_EDGE ( 'NONE', *, *, #28475, .T. ) ;
#30384 = ORIENTED_EDGE ( 'NONE', *, *, #41857, .F. ) ;
#30385 = ORIENTED_EDGE ( 'NONE', *, *, #15412, .T. ) ;
#30386 = DIRECTION ( 'NONE',  ( 1.000000000000000000, -0.000000000000000000, -0.000000000000000000 ) ) ;
#30387 = CARTESIAN_POINT ( 'NONE',  ( -336.3521761649654422, -141.9604555052315220, 56.09938080879057765 ) ) ;
#30388 =( LENGTH_UNIT ( ) NAMED_UNIT ( * ) SI_UNIT ( .MILLI., .METRE. ) );
#30389 = DIRECTION ( 'NONE',  ( 0.000000000000000000, 0.000000000000000000, -1.000000000000000000 ) ) ;
#30390 = DIRECTION ( 'NONE',  ( 0.000000000000000000, -1.000000000000000000, 0.000000000000000000 ) ) ;
#30391 = AXIS2_PLACEMENT_3D ( 'NONE', #2883, #18666, #50729 ) ;
#30392 = VERTEX_POINT ( 'NONE', #6546 ) ;
#30393 = EDGE_CURVE ( 'NONE', #5531, #45414, #7052, .T. ) ;
#30394 = ADVANCED_FACE ( 'NONE', ( #23076 ), #3098, .T. ) ;
#30395 = VECTOR ( 'NONE', #25800, 1000.000000000000000 ) ;
#30396 = DIRECTION ( 'NONE',  ( -1.000000000000000000, -0.000000000000000000, 0.000000000000000000 ) ) ;
#30397 = ORIENTED_EDGE ( 'NONE', *, *, #9938, .F. ) ;
#30399 = ORIENTED_EDGE ( 'NONE', *, *, #48967, .F. ) ;
#30398 = DIRECTION ( 'NONE',  ( 0.000000000000000000, 0.000000000000000000, 1.000000000000000000 ) ) ;
#30400 = ORIENTED_EDGE ( 'NONE', *, *, #37169, .F. ) ;
#30401 = EDGE_CURVE ( 'NONE', #7429, #41297, #39353, .T. ) ;
#30402 = CARTESIAN_POINT ( 'NONE',  ( 1.734723475976807094E-15, 0.000000000000000000, 46.00000000000000711 ) ) ;
#30403 = EDGE_LOOP ( 'NONE', ( #36341, #5966, #6683, #35096 ) ) ;
#30404 = CARTESIAN_POINT ( 'NONE',  ( -339.1964088526558498, -123.0000000000002700, -59.99791663049643375 ) ) ;
#30405 = ORIENTED_EDGE ( 'NONE', *, *, #6777, .F. ) ;
#30406 = EDGE_CURVE ( 'NONE', #5648, #39766, #27527, .T. ) ;
#30407 = DIRECTION ( 'NONE',  ( 0.000000000000000000, -1.000000000000000000, 0.000000000000000000 ) ) ;
#30408 = DIRECTION ( 'NONE',  ( -0.000000000000000000, -1.000000000000000000, -0.000000000000000000 ) ) ;
#30409 = EDGE_LOOP ( 'NONE', ( #8166, #37451, #41708, #24767 ) ) ;
#30410 = DIRECTION ( 'NONE',  ( -1.000000000000000000, 0.000000000000000000, 0.000000000000000000 ) ) ;
#30411 = VERTEX_POINT ( 'NONE', #47775 ) ;
#30412 = VECTOR ( 'NONE', #14757, 1000.000000000000000 ) ;
#30413 = VECTOR ( 'NONE', #14594, 1000.000000000000114 ) ;
#30414 = EDGE_LOOP ( 'NONE', ( #1941, #47719, #4688, #30022 ) ) ;
#30415 = DIRECTION ( 'NONE',  ( -0.9266896074318370369, 0.000000000000000000, 0.3758275821142292306 ) ) ;
#30416 = AXIS2_PLACEMENT_3D ( 'NONE', #29330, #8333, #8837 ) ;
#30418 = VECTOR ( 'NONE', #18493, 1000.000000000000000 ) ;
#30417 = CARTESIAN_POINT ( 'NONE',  ( -163.0741914257288272, -193.5000000000000000, 47.37063079638402030 ) ) ;
#30419 = DIRECTION ( 'NONE',  ( -0.2348860457809911206, 0.000000000000000000, 0.9720229140804089729 ) ) ;
#30420 = DIRECTION ( 'NONE',  ( 0.000000000000000000, 1.000000000000000000, 0.000000000000000000 ) ) ;
#30421 = ORIENTED_EDGE ( 'NONE', *, *, #155, .F. ) ;
#30422 = CARTESIAN_POINT ( 'NONE',  ( 40.29886924377099433, 30.00000000000000355, -46.21030057994576623 ) ) ;
#30423 = CARTESIAN_POINT ( 'NONE',  ( -238.7407812814481076, -213.5000000000000000, 41.45482488023466772 ) ) ;
#30424 = DIRECTION ( 'NONE',  ( -0.000000000000000000, 1.000000000000000000, 0.000000000000000000 ) ) ;
#30425 = LINE ( 'NONE', #21783, #45517 ) ;
#30426 = ORIENTED_EDGE ( 'NONE', *, *, #39112, .F. ) ;
#30427 = CARTESIAN_POINT ( 'NONE',  ( 24.63024857337166296, -177.1207230881787780, 101.3904297239426597 ) ) ;
#30428 = CARTESIAN_POINT ( 'NONE',  ( -47.49008656418669005, -193.5000000000000000, 0.1476465640024920423 ) ) ;
#30429 = CARTESIAN_POINT ( 'NONE',  ( -108.0638572795231624, -193.5000000000000000, 108.7464374498172788 ) ) ;
#30430 = ORIENTED_EDGE ( 'NONE', *, *, #29092, .F. ) ;
#30431 = CARTESIAN_POINT ( 'NONE',  ( 1.150725574412429175, -189.7472609257535510, -114.7252272087845739 ) ) ;
#30432 = CARTESIAN_POINT ( 'NONE',  ( 72.71365293123227502, -177.1207230881787780, -30.61552143554913030 ) ) ;
#30433 = EDGE_LOOP ( 'NONE', ( #43489, #14643, #4911, #39491 ) ) ;
#30434 = FACE_OUTER_BOUND ( 'NONE', #36872, .T. ) ;
#30435 = EDGE_LOOP ( 'NONE', ( #37262, #44105, #19996, #13182 ) ) ;
#30436 = VECTOR ( 'NONE', #17919, 1000.000000000000000 ) ;
#30437 = EDGE_CURVE ( 'NONE', #49553, #11600, #12785, .T. ) ;
#30438 = DIRECTION ( 'NONE',  ( 0.000000000000000000, 0.000000000000000000, -1.000000000000000000 ) ) ;
#30439 = DIRECTION ( 'NONE',  ( 0.000000000000000000, 0.000000000000000000, -1.000000000000000000 ) ) ;
#30440 = CARTESIAN_POINT ( 'NONE',  ( -123.4791267515088435, -198.5000000000000000, 70.00000000000000000 ) ) ;
#30441 = ADVANCED_FACE ( 'NONE', ( #717 ), #28808, .T. ) ;
#30442 = EDGE_CURVE ( 'NONE', #30079, #39568, #19906, .T. ) ;
#30443 = CARTESIAN_POINT ( 'NONE',  ( -330.4913330509368166, -162.2499814621210419, 44.49369547121568758 ) ) ;
#30444 = ADVANCED_FACE ( 'NONE', ( #44598 ), #12536, .T. ) ;
#30446 = AXIS2_PLACEMENT_3D ( 'NONE', #37864, #38384, #38114 ) ;
#30445 = DIRECTION ( 'NONE',  ( 0.000000000000000000, 0.000000000000000000, 1.000000000000000000 ) ) ;
#30447 = AXIS2_PLACEMENT_3D ( 'NONE', #16238, #23593, #27788 ) ;
#30448 = ORIENTED_EDGE ( 'NONE', *, *, #3159, .F. ) ;
#30449 = EDGE_CURVE ( 'NONE', #47538, #8253, #16763, .T. ) ;
#30450 = CARTESIAN_POINT ( 'NONE',  ( 57.61256176024323139, -177.1207230881787780, -64.19309449102733822 ) ) ;
#30451 = VERTEX_POINT ( 'NONE', #32511 ) ;
#30452 = DIRECTION ( 'NONE',  ( 0.000000000000000000, -1.000000000000000000, 0.000000000000000000 ) ) ;
#30453 = AXIS2_PLACEMENT_3D ( 'NONE', #26940, #51652, #15656 ) ;
#30454 = AXIS2_PLACEMENT_3D ( 'NONE', #3480, #19508, #43443 ) ;
#30455 = ORIENTED_EDGE ( 'NONE', *, *, #32272, .T. ) ;
#30456 = ADVANCED_FACE ( 'NONE', ( #40905 ), #8587, .F. ) ;
#30457 = CARTESIAN_POINT ( 'NONE',  ( -305.0000000000000568, -151.8251501453679850, 52.89315522109039591 ) ) ;
#30458 = EDGE_CURVE ( 'NONE', #5935, #15465, #48560, .T. ) ;
#30459 = EDGE_CURVE ( 'NONE', #51292, #17406, #36182, .T. ) ;
#30460 = CARTESIAN_POINT ( 'NONE',  ( 37.99238433767461487, -175.3837268820161057, -90.26448786734027863 ) ) ;
#30461 = FACE_OUTER_BOUND ( 'NONE', #37585, .T. ) ;
#30462 = ORIENTED_EDGE ( 'NONE', *, *, #29523, .T. ) ;
#30465 = ORIENTED_EDGE ( 'NONE', *, *, #33241, .F. ) ;
#30464 = DIRECTION ( 'NONE',  ( -0.000000000000000000, -0.7485107481710953081, 0.6631226582408016323 ) ) ;
#30463 = CARTESIAN_POINT ( 'NONE',  ( -0.2952669786863603152, 50.59471834446340921, -21.36672353920344847 ) ) ;
#30466 = EDGE_CURVE ( 'NONE', #15488, #8881, #40630, .T. ) ;
#30467 = DIRECTION ( 'NONE',  ( 0.000000000000000000, -0.000000000000000000, 1.000000000000000000 ) ) ;
#30468 = ORIENTED_EDGE ( 'NONE', *, *, #26912, .T. ) ;
#30469 = LINE ( 'NONE', #29962, #42357 ) ;
#30470 = AXIS2_PLACEMENT_3D ( 'NONE', #9244, #17903, #29713 ) ;
#30471 = VERTEX_POINT ( 'NONE', #15973 ) ;
#30472 = EDGE_CURVE ( 'NONE', #42957, #43466, #31981, .T. ) ;
#30473 = CARTESIAN_POINT ( 'NONE',  ( -330.4913330509368166, -182.1300919119129560, -6.615309698014691264 ) ) ;
#30476 = ORIENTED_EDGE ( 'NONE', *, *, #43744, .T. ) ;
#30475 = CARTESIAN_POINT ( 'NONE',  ( 43.12693905415815721, -189.7472609257535510, -83.57229767764155781 ) ) ;
#30474 = CARTESIAN_POINT ( 'NONE',  ( -490.0000000000001137, -78.50000000000002842, 0.000000000000000000 ) ) ;
#30477 = VERTEX_POINT ( 'NONE', #11749 ) ;
#30478 = EDGE_CURVE ( 'NONE', #15102, #39679, #4928, .T. ) ;
#30479 = DIRECTION ( 'NONE',  ( 0.000000000000000000, -1.000000000000000000, 0.000000000000000000 ) ) ;
#30480 = ORIENTED_EDGE ( 'NONE', *, *, #22922, .T. ) ;
#30481 = DIRECTION ( 'NONE',  ( -1.000000000000000000, 0.000000000000000000, 0.000000000000000000 ) ) ;
#30482 = DIRECTION ( 'NONE',  ( 0.000000000000000000, 1.000000000000000000, 0.000000000000000000 ) ) ;
#30483 = VERTEX_POINT ( 'NONE', #51718 ) ;
#30484 = DIRECTION ( 'NONE',  ( -0.000000000000000000, -0.9709418174260502354, 0.2393156642875652051 ) ) ;
#30485 = CARTESIAN_POINT ( 'NONE',  ( -71.40672220061267694, -175.3837268820161057, -122.8793122007208751 ) ) ;
#30486 = CARTESIAN_POINT ( 'NONE',  ( 0.000000000000000000, -68.33404168156053515, -20.92168833550964990 ) ) ;
#30487 = LINE ( 'NONE', #38107, #28446 ) ;
#30488 = CARTESIAN_POINT ( 'NONE',  ( -148.6149069237406195, -183.6283474603465606, -74.81861753132355375 ) ) ;
#30489 = ORIENTED_EDGE ( 'NONE', *, *, #49889, .F. ) ;
#30490 = VECTOR ( 'NONE', #28129, 1000.000000000000114 ) ;
#30491 = DIRECTION ( 'NONE',  ( 0.000000000000000000, -1.000000000000000000, 0.000000000000000000 ) ) ;
#30492 = EDGE_CURVE ( 'NONE', #27780, #22881, #42406, .T. ) ;
#30493 = CARTESIAN_POINT ( 'NONE',  ( -134.7293151056888121, -189.7472609257535510, -89.08931047202582931 ) ) ;
#30494 = LINE ( 'NONE', #26042, #17085 ) ;
#30495 = ORIENTED_EDGE ( 'NONE', *, *, #22399, .F. ) ;
#30496 = VECTOR ( 'NONE', #16203, 1000.000000000000000 ) ;
#30497 = DIRECTION ( 'NONE',  ( 0.000000000000000000, -0.000000000000000000, -1.000000000000000000 ) ) ;
#30498 = DIRECTION ( 'NONE',  ( -1.000000000000000000, 0.000000000000000000, 0.000000000000000000 ) ) ;
#30499 = CARTESIAN_POINT ( 'NONE',  ( -65.47874029382337824, -177.1207230881787780, 122.8300162461137006 ) ) ;
#30500 = DIRECTION ( 'NONE',  ( -0.000000000000000000, -0.4647231720437724478, -0.8854560256532078011 ) ) ;
#30501 = VECTOR ( 'NONE', #20355, 1000.000000000000227 ) ;
#30502 = ORIENTED_EDGE ( 'NONE', *, *, #28902, .T. ) ;
#30503 = CARTESIAN_POINT ( 'NONE',  ( 46.00000000000000711, 35.00000000000000000, -37.00000000000000000 ) ) ;
#30504 = DIRECTION ( 'NONE',  ( 0.000000000000000000, 0.000000000000000000, 1.000000000000000000 ) ) ;
#30505 = PLANE ( 'NONE',  #47202 ) ;
#30506 = VECTOR ( 'NONE', #36430, 1000.000000000000000 ) ;
#30507 = ORIENTED_EDGE ( 'NONE', *, *, #902, .T. ) ;
#30508 = EDGE_CURVE ( 'NONE', #24657, #23768, #3803, .T. ) ;
#30509 = ADVANCED_FACE ( 'NONE', ( #32767 ), #27775, .T. ) ;
#30510 = DIRECTION ( 'NONE',  ( 0.000000000000000000, 0.000000000000000000, 1.000000000000000000 ) ) ;
#30511 = CIRCLE ( 'NONE', #51497, 125.0000000000000000 ) ;
#30512 = EDGE_CURVE ( 'NONE', #18084, #32311, #20414, .T. ) ;
#30513 = EDGE_CURVE ( 'NONE', #50350, #23163, #4149, .T. ) ;
#30514 = LINE ( 'NONE', #22896, #38911 ) ;
#30515 = VERTEX_POINT ( 'NONE', #12267 ) ;
#30516 = ORIENTED_EDGE ( 'NONE', *, *, #21536, .T. ) ;
#30517 = ORIENTED_EDGE ( 'NONE', *, *, #32622, .T. ) ;
#30518 = DIRECTION ( 'NONE',  ( -1.000000000000000000, -0.000000000000000000, -0.000000000000000000 ) ) ;
#30519 = CARTESIAN_POINT ( 'NONE',  ( 35.45604639379470058, -193.5000000000000000, 91.27439114664650788 ) ) ;
#30520 = LINE ( 'NONE', #42348, #25471 ) ;
#30522 = ORIENTED_EDGE ( 'NONE', *, *, #31727, .F. ) ;
#30521 = VECTOR ( 'NONE', #739, 1000.000000000000000 ) ;
#30523 = DIRECTION ( 'NONE',  ( 0.000000000000000000, 1.000000000000000000, 0.000000000000000000 ) ) ;
#30524 = LINE ( 'NONE', #34723, #14326 ) ;
#30527 = ORIENTED_EDGE ( 'NONE', *, *, #46911, .F. ) ;
#30526 = LINE ( 'NONE', #42354, #9859 ) ;
#30525 = DIRECTION ( 'NONE',  ( -0.000000000000000000, -1.000000000000000000, 0.000000000000000000 ) ) ;
#30528 = ADVANCED_FACE ( 'NONE', ( #21975 ), #37997, .T. ) ;
#30529 = DIRECTION ( 'NONE',  ( 0.000000000000000000, 1.000000000000000000, 0.000000000000000000 ) ) ;
#30530 = ORIENTED_EDGE ( 'NONE', *, *, #23356, .T. ) ;
#30531 = DIRECTION ( 'NONE',  ( -1.000000000000000000, 7.812315528781935576E-15, 6.921107616850706142E-15 ) ) ;
#30532 = VERTEX_POINT ( 'NONE', #14106 ) ;
#30533 = PLANE ( 'NONE',  #22432 ) ;
#30534 = DIRECTION ( 'NONE',  ( -0.000000000000000000, 1.000000000000000000, -0.000000000000000000 ) ) ;
#30535 = DIRECTION ( 'NONE',  ( -0.000000000000000000, 0.9350162426854194964, 0.3546048870425235200 ) ) ;
#30536 = ADVANCED_FACE ( 'NONE', ( #42193 ), #41943, .T. ) ;
#30537 = ORIENTED_EDGE ( 'NONE', *, *, #22155, .T. ) ;
#30538 = CARTESIAN_POINT ( 'NONE',  ( -49.25565061422688728, -183.6283474603465606, -0.6300878435817132139 ) ) ;
#30539 = DIRECTION ( 'NONE',  ( -0.000000000000000000, 1.000000000000000000, 0.000000000000000000 ) ) ;
#30540 = ORIENTED_EDGE ( 'NONE', *, *, #140, .F. ) ;
#30541 = CYLINDRICAL_SURFACE ( 'NONE', #44208, 16.00000000000000711 ) ;
#30542 = AXIS2_PLACEMENT_3D ( 'NONE', #24877, #51611, #40537 ) ;
#30543 = CARTESIAN_POINT ( 'NONE',  ( -332.3517673607765914, -177.7325358280884586, 23.38292116578760726 ) ) ;
#30544 = VECTOR ( 'NONE', #7859, 1000.000000000000000 ) ;
#30545 = EDGE_LOOP ( 'NONE', ( #42596, #35894, #7230, #32318 ) ) ;
#30546 = LINE ( 'NONE', #46597, #40175 ) ;
#30548 = VECTOR ( 'NONE', #18608, 1000.000000000000000 ) ;
#30547 = DIRECTION ( 'NONE',  ( 0.8124868780056863082, 0.000000000000000000, -0.5829794791144649047 ) ) ;
#30549 = ORIENTED_EDGE ( 'NONE', *, *, #20088, .T. ) ;
#30550 = FACE_OUTER_BOUND ( 'NONE', #14207, .T. ) ;
#30551 = ORIENTED_EDGE ( 'NONE', *, *, #39576, .T. ) ;
#30552 = DIRECTION ( 'NONE',  ( -0.9266896074318291543, 0.000000000000000000, -0.3758275821142488260 ) ) ;
#30553 = CARTESIAN_POINT ( 'NONE',  ( 74.49773146996547268, -193.5000000000000000, -22.39848972532282190 ) ) ;
#30554 = ORIENTED_EDGE ( 'NONE', *, *, #49403, .T. ) ;
#30555 = CARTESIAN_POINT ( 'NONE',  ( 0.000000000000000000, -96.08133284941780516, -52.24190551353947143 ) ) ;
#30556 = CARTESIAN_POINT ( 'NONE',  ( 76.04209377433248562, -175.3837268820161057, -10.93003379476866677 ) ) ;
#30557 = DIRECTION ( 'NONE',  ( 0.000000000000000000, -0.000000000000000000, 1.000000000000000000 ) ) ;
#30558 = VECTOR ( 'NONE', #50389, 1000.000000000000000 ) ;
#30559 = ORIENTED_EDGE ( 'NONE', *, *, #38805, .F. ) ;
#30560 = PLANE ( 'NONE',  #22886 ) ;
#30561 = ORIENTED_EDGE ( 'NONE', *, *, #18905, .F. ) ;
#30562 = PLANE ( 'NONE',  #21105 ) ;
#30563 = DIRECTION ( 'NONE',  ( 0.000000000000000000, 0.7485107481711089639, 0.6631226582407863113 ) ) ;
#30565 = ORIENTED_EDGE ( 'NONE', *, *, #13978, .F. ) ;
#30564 = LINE ( 'NONE', #50559, #10234 ) ;
#30566 = ORIENTED_EDGE ( 'NONE', *, *, #7143, .T. ) ;
#30567 = EDGE_CURVE ( 'NONE', #48304, #12908, #49845, .T. ) ;
#30568 = DIRECTION ( 'NONE',  ( -0.9785564922995060311, 0.000000000000000000, 0.2059786187410889424 ) ) ;
#30569 = FACE_OUTER_BOUND ( 'NONE', #19584, .T. ) ;
#30570 = EDGE_LOOP ( 'NONE', ( #32032, #30755, #13012, #6068 ) ) ;
#30571 = FACE_OUTER_BOUND ( 'NONE', #44310, .T. ) ;
#30572 = ORIENTED_EDGE ( 'NONE', *, *, #37450, .T. ) ;
#30573 = DIRECTION ( 'NONE',  ( -0.000000000000000000, -0.9927088740980548609, -0.1205366802553164696 ) ) ;
#30574 = CARTESIAN_POINT ( 'NONE',  ( -48.47912675150885065, -183.6283474603465606, 6.938893903907228378E-15 ) ) ;
#30575 = VECTOR ( 'NONE', #25766, 1000.000000000000000 ) ;
#30576 = VECTOR ( 'NONE', #23473, 1000.000000000000000 ) ;
#30577 = LINE ( 'NONE', #6935, #12704 ) ;
#30578 = PLANE ( 'NONE',  #18193 ) ;
#30579 = ORIENTED_EDGE ( 'NONE', *, *, #40435, .F. ) ;
#30580 = VERTEX_POINT ( 'NONE', #25656 ) ;
#30581 = VECTOR ( 'NONE', #18797, 1000.000000000000000 ) ;
#30582 = ORIENTED_EDGE ( 'NONE', *, *, #51775, .F. ) ;
#30583 = DIRECTION ( 'NONE',  ( 0.000000000000000000, -1.000000000000000000, 0.000000000000000000 ) ) ;
#30584 = DIRECTION ( 'NONE',  ( -0.000000000000000000, -1.000000000000000000, -0.000000000000000000 ) ) ;
#30585 = EDGE_CURVE ( 'NONE', #15918, #32858, #31481, .T. ) ;
#30586 = DIRECTION ( 'NONE',  ( 0.4031234292879665171, 0.000000000000000000, 0.9151456172430210145 ) ) ;
#30587 = CARTESIAN_POINT ( 'NONE',  ( 48.33059356687144970, -175.3837268820161057, 77.48473115145309009 ) ) ;
#30588 = ORIENTED_EDGE ( 'NONE', *, *, #32045, .T. ) ;
#30589 = VECTOR ( 'NONE', #7271, 1000.000000000000000 ) ;
#30590 = CARTESIAN_POINT ( 'NONE',  ( -330.4913330509368166, -167.9936954712150339, 38.74998146212178796 ) ) ;
#30591 = CARTESIAN_POINT ( 'NONE',  ( 60.00000000000000000, -63.50000000000000000, 60.00000000000000711 ) ) ;
#30592 = EDGE_CURVE ( 'NONE', #52027, #34819, #41688, .T. ) ;
#30593 = VERTEX_POINT ( 'NONE', #961 ) ;
#30594 = ORIENTED_EDGE ( 'NONE', *, *, #24527, .F. ) ;
#30595 = FACE_OUTER_BOUND ( 'NONE', #10787, .T. ) ;
#30596 = CARTESIAN_POINT ( 'NONE',  ( -336.3521761649653854, -149.9277501395804677, 53.86626052140529453 ) ) ;
#30597 = CARTESIAN_POINT ( 'NONE',  ( -7.223120065443615623, -193.5000000000000000, 117.9955164924470523 ) ) ;
#30598 = CARTESIAN_POINT ( 'NONE',  ( -48.47912675150885065, -189.7472609257535510, 6.938893903907228378E-15 ) ) ;
#30599 = ORIENTED_EDGE ( 'NONE', *, *, #51160, .F. ) ;
#30601 = EDGE_CURVE ( 'NONE', #23160, #27018, #5710, .T. ) ;
#30600 = DIRECTION ( 'NONE',  ( 0.000000000000000000, 0.000000000000000000, 1.000000000000000000 ) ) ;
#30602 = ORIENTED_EDGE ( 'NONE', *, *, #15519, .F. ) ;
#30603 = DIRECTION ( 'NONE',  ( 0.000000000000000000, -0.2393156642875547968, 0.9709418174260527890 ) ) ;
#30604 = VECTOR ( 'NONE', #34870, 1000.000000000000000 ) ;
#30605 = DIRECTION ( 'NONE',  ( 0.000000000000000000, -3.491481338843133355E-15, -1.000000000000000000 ) ) ;
#30606 = EDGE_LOOP ( 'NONE', ( #7894, #8133, #673, #35363 ) ) ;
#30607 = CIRCLE ( 'NONE', #44884, 15.00000000000000000 ) ;
#30608 = DIRECTION ( 'NONE',  ( -0.000000000000000000, 1.000000000000000000, -0.000000000000000000 ) ) ;
#30609 = CARTESIAN_POINT ( 'NONE',  ( -46.00000000000000711, 0.000000000000000000, 46.00000000000000000 ) ) ;
#30610 = DIRECTION ( 'NONE',  ( 0.000000000000000000, -0.1205366802553337752, -0.9927088740980526405 ) ) ;
#30611 = CARTESIAN_POINT ( 'NONE',  ( -280.0000000000000000, -123.5000000000000284, 6.938893903907228378E-15 ) ) ;
#30612 = AXIS2_PLACEMENT_3D ( 'NONE', #22294, #38322, #28420 ) ;
#30613 = ADVANCED_FACE ( 'NONE', ( #5445 ), #46167, .T. ) ;
#30614 = CARTESIAN_POINT ( 'NONE',  ( -49.45768324380835423, -193.5000000000000000, -0.2059786187411025149 ) ) ;
#30615 = EDGE_LOOP ( 'NONE', ( #29927, #47734, #22696, #40252 ) ) ;
#30616 = CIRCLE ( 'NONE', #421, 125.0000000000000000 ) ;
#30617 = CARTESIAN_POINT ( 'NONE',  ( -332.3517673607765914, -75.66382151296542702, -36.21739951675945690 ) ) ;
#30618 = ORIENTED_EDGE ( 'NONE', *, *, #20787, .F. ) ;
#30619 = CIRCLE ( 'NONE', #33149, 5.000000000000001776 ) ;
#30620 = ORIENTED_EDGE ( 'NONE', *, *, #37871, .F. ) ;
#30621 = DIRECTION ( 'NONE',  ( 0.2920567706369694982, 0.000000000000000000, 0.9564009842765243130 ) ) ;
#30622 = EDGE_CURVE ( 'NONE', #43863, #42973, #21726, .T. ) ;
#30623 = CIRCLE ( 'NONE', #47411, 60.00000000000000000 ) ;
#30624 = ORIENTED_EDGE ( 'NONE', *, *, #39424, .F. ) ;
#30625 = AXIS2_PLACEMENT_3D ( 'NONE', #14705, #10756, #38860 ) ;
#30626 = PRODUCT_DEFINITION_SHAPE ( 'NONE', 'NONE',  #36651 ) ;
#30627 = DIRECTION ( 'NONE',  ( -0.000000000000000000, 1.000000000000000000, -0.000000000000000000 ) ) ;
#30628 = EDGE_CURVE ( 'NONE', #13250, #28174, #45909, .T. ) ;
#30629 = EDGE_LOOP ( 'NONE', ( #48993, #2444, #43048, #27947 ) ) ;
#30630 = CARTESIAN_POINT ( 'NONE',  ( 64.72501964220592185, -175.3837268820161057, 53.00774697410174952 ) ) ;
#30631 = LINE ( 'NONE', #38536, #35507 ) ;
#30632 = VERTEX_POINT ( 'NONE', #9631 ) ;
#30633 = DIRECTION ( 'NONE',  ( 0.000000000000000000, 0.1205366802553233113, 0.9927088740980538617 ) ) ;
#30634 = CARTESIAN_POINT ( 'NONE',  ( -330.4913330509368166, -137.1341532842523918, 57.40522506028099770 ) ) ;
#30635 = DIRECTION ( 'NONE',  ( -1.000000000000000000, -0.000000000000000000, -0.000000000000000000 ) ) ;
#30636 = EDGE_LOOP ( 'NONE', ( #38293, #17633, #11503, #43781 ) ) ;
#30637 = VERTEX_POINT ( 'NONE', #33551 ) ;
#30638 = EDGE_LOOP ( 'NONE', ( #18646, #17867, #23525, #2565 ) ) ;
#30639 = CARTESIAN_POINT ( 'NONE',  ( 72.95485052494852596, -183.6283474603465606, -29.64437826672758192 ) ) ;
#30640 = CARTESIAN_POINT ( 'NONE',  ( 65.79610465833508215, -177.1207230881787780, -50.65739320401928580 ) ) ;
#30641 = VECTOR ( 'NONE', #36836, 1000.000000000000227 ) ;
#30642 = ADVANCED_FACE ( 'NONE', ( #26161 ), #9125, .T. ) ;
#30643 = CARTESIAN_POINT ( 'NONE',  ( -330.4913330509368166, -122.9999999999994600, 59.00000000000002132 ) ) ;
#30644 = AXIS2_PLACEMENT_3D ( 'NONE', #37005, #29114, #16529 ) ;
#30645 = DIRECTION ( 'NONE',  ( 0.000000000000000000, -1.000000000000000000, 1.541976423090494894E-16 ) ) ;
#30646 = DIRECTION ( 'NONE',  ( 0.000000000000000000, -0.9709418174260511236, 0.2393156642875615969 ) ) ;
#30647 = VERTEX_POINT ( 'NONE', #5186 ) ;
#30648 = AXIS2_PLACEMENT_3D ( 'NONE', #18227, #28538, #44584 ) ;
#30649 = VECTOR ( 'NONE', #44075, 999.9999999999998863 ) ;
#30650 = CARTESIAN_POINT ( 'NONE',  ( -37.67038537088846084, -177.1207230881787780, -124.5318076226586470 ) ) ;
#30651 = EDGE_LOOP ( 'NONE', ( #11965, #48216, #31658, #27861 ) ) ;
#30653 = VERTEX_POINT ( 'NONE', #13838 ) ;
#30652 = DIRECTION ( 'NONE',  ( 0.000000000000000000, 0.000000000000000000, 1.000000000000000000 ) ) ;
#30654 = ORIENTED_EDGE ( 'NONE', *, *, #436, .T. ) ;
#30655 = CARTESIAN_POINT ( 'NONE',  ( 72.35619569422320296, -193.5000000000000000, 27.83926365844748574 ) ) ;
#30656 = CIRCLE ( 'NONE', #27283, 125.0000000000000000 ) ;
#30657 = ORIENTED_EDGE ( 'NONE', *, *, #40446, .F. ) ;
#30658 = CARTESIAN_POINT ( 'NONE',  ( -365.0000000000001137, -78.50000000000002842, 0.000000000000000000 ) ) ;
#30659 = VECTOR ( 'NONE', #32758, 1000.000000000000000 ) ;
#30660 = DIRECTION ( 'NONE',  ( 1.000000000000000000, -0.000000000000000000, -0.000000000000000000 ) ) ;
#30661 = CARTESIAN_POINT ( 'NONE',  ( -159.5526844214375615, -177.1207230881787780, 57.33816169485226055 ) ) ;
#30662 = EDGE_LOOP ( 'NONE', ( #13557, #13390, #36946, #5510 ) ) ;
#30663 = DIRECTION ( 'NONE',  ( -0.000000000000000000, -1.000000000000000000, -0.000000000000000000 ) ) ;
#30664 = AXIS2_PLACEMENT_3D ( 'NONE', #47348, #43408, #31560 ) ;
#30665 = ORIENTED_EDGE ( 'NONE', *, *, #36446, .F. ) ;
#30666 = AXIS2_PLACEMENT_3D ( 'NONE', #49613, #35068, #11140 ) ;
#30667 = ORIENTED_EDGE ( 'NONE', *, *, #28579, .T. ) ;
#30668 = DIRECTION ( 'NONE',  ( 0.000000000000000000, 1.000000000000000000, 0.000000000000000000 ) ) ;
#30669 = DIRECTION ( 'NONE',  ( -0.000000000000000000, 1.000000000000000000, -0.000000000000000000 ) ) ;
#30670 = DIRECTION ( 'NONE',  ( 0.000000000000000000, 0.000000000000000000, 1.000000000000000000 ) ) ;
#30671 = DIRECTION ( 'NONE',  ( -0.000000000000000000, 1.000000000000000000, -0.000000000000000000 ) ) ;
#30672 = VERTEX_POINT ( 'NONE', #45137 ) ;
#30673 = DIRECTION ( 'NONE',  ( 0.000000000000000000, -1.000000000000000000, 0.000000000000000000 ) ) ;
#30674 = FACE_OUTER_BOUND ( 'NONE', #13366, .T. ) ;
#30675 = EDGE_CURVE ( 'NONE', #19021, #33918, #17014, .T. ) ;
#30676 = EDGE_CURVE ( 'NONE', #14977, #32186, #6213, .T. ) ;
#30677 = CARTESIAN_POINT ( 'NONE',  ( -339.1964088526558498, -178.8432607619606358, 20.45418021416736565 ) ) ;
#30678 = LINE ( 'NONE', #25976, #6944 ) ;
#30679 = ORIENTED_EDGE ( 'NONE', *, *, #24893, .T. ) ;
#30680 = DIRECTION ( 'NONE',  ( 0.000000000000000000, 0.3546048870425463906, 0.9350162426854107256 ) ) ;
#30681 = CYLINDRICAL_SURFACE ( 'NONE', #19764, 125.0000000000000000 ) ;
#30682 = FACE_BOUND ( 'NONE', #5165, .T. ) ;
#30683 = VERTEX_POINT ( 'NONE', #41166 ) ;
#30684 = AXIS2_PLACEMENT_3D ( 'NONE', #47316, #51510, #48343 ) ;
#30685 = LINE ( 'NONE', #22573, #5474 ) ;
#30686 = CIRCLE ( 'NONE', #11365, 125.0000000000000000 ) ;
#30687 = VECTOR ( 'NONE', #34499, 1000.000000000000114 ) ;
#30688 = CARTESIAN_POINT ( 'NONE',  ( -156.2577088867455473, -177.1207230881787780, -63.31490529818419333 ) ) ;
#30689 = VERTEX_POINT ( 'NONE', #49331 ) ;
#30690 = DIRECTION ( 'NONE',  ( 0.000000000000000000, -0.8854560256532141294, -0.4647231720437604574 ) ) ;
#30691 = EDGE_CURVE ( 'NONE', #2959, #8311, #44088, .T. ) ;
#30692 = ORIENTED_EDGE ( 'NONE', *, *, #15427, .T. ) ;
#30693 = EDGE_CURVE ( 'NONE', #21286, #47980, #29071, .T. ) ;
#30694 = CARTESIAN_POINT ( 'NONE',  ( -339.1964088526558498, -178.8432607619609485, -20.45418021416653076 ) ) ;
#30695 = ADVANCED_FACE ( 'NONE', ( #18040 ), #25154, .F. ) ;
#30696 = DIRECTION ( 'NONE',  ( 1.000000000000000000, 0.000000000000000000, 0.000000000000000000 ) ) ;
#30697 = CIRCLE ( 'NONE', #34894, 125.0000000000000000 ) ;
#30698 = DIRECTION ( 'NONE',  ( -0.000000000000000000, -1.000000000000000000, 0.000000000000000000 ) ) ;
#30699 = CARTESIAN_POINT ( 'NONE',  ( -158.1873290247468447, -183.6283474603465606, 57.79541595648306185 ) ) ;
#30700 = AXIS2_PLACEMENT_3D ( 'NONE', #11932, #8001, #24035 ) ;
#30701 = FACE_OUTER_BOUND ( 'NONE', #38583, .T. ) ;
#30702 = CIRCLE ( 'NONE', #41583, 60.00000000000000000 ) ;
#30703 = CARTESIAN_POINT ( 'NONE',  ( -339.1964088526558498, -115.8919814278871598, -58.50955523165758621 ) ) ;
#30704 = ORIENTED_EDGE ( 'NONE', *, *, #29013, .F. ) ;
#30705 = DIRECTION ( 'NONE',  ( 1.000000000000000000, -0.000000000000000000, 0.000000000000000000 ) ) ;
#30706 = ORIENTED_EDGE ( 'NONE', *, *, #26620, .T. ) ;
#30707 = VECTOR ( 'NONE', #7234, 1000.000000000000000 ) ;
#30708 = LINE ( 'NONE', #3373, #701 ) ;
#30709 = VERTEX_POINT ( 'NONE', #51400 ) ;
#30710 = CARTESIAN_POINT ( 'NONE',  ( -162.4844509910036265, -177.1207230881787780, -48.77484799213895172 ) ) ;
#30711 = DIRECTION ( 'NONE',  ( 0.000000000000000000, 0.000000000000000000, 1.000000000000000000 ) ) ;
#30712 = DIRECTION ( 'NONE',  ( 0.000000000000000000, 0.000000000000000000, 1.000000000000000000 ) ) ;
#30713 = ORIENTED_EDGE ( 'NONE', *, *, #16889, .T. ) ;
#30716 = ORIENTED_EDGE ( 'NONE', *, *, #33303, .F. ) ;
#30715 = CARTESIAN_POINT ( 'NONE',  ( -77.03256798524175508, -193.5000000000000000, 121.6951149130964893 ) ) ;
#30714 = CARTESIAN_POINT ( 'NONE',  ( -3.556303009769684831, 56.50711438170559120, -17.15815478421502505 ) ) ;
#30717 = AXIS2_PLACEMENT_3D ( 'NONE', #13566, #24361, #45130 ) ;
#30718 = CIRCLE ( 'NONE', #44156, 125.0000000000000000 ) ;
#30719 = CARTESIAN_POINT ( 'NONE',  ( -332.3517673607765914, -82.40546666720629787, 42.41660376256258047 ) ) ;
#30720 = AXIS2_PLACEMENT_3D ( 'NONE', #27311, #43354, #7096 ) ;
#30721 = EDGE_LOOP ( 'NONE', ( #3053, #33575, #42741, #7239 ) ) ;
#30722 = CARTESIAN_POINT ( 'NONE',  ( -336.3521761649654422, -98.41210887299327226, -53.46519113769058151 ) ) ;
#30723 = ORIENTED_EDGE ( 'NONE', *, *, #31239, .F. ) ;
#30724 = AXIS2_PLACEMENT_3D ( 'NONE', #8400, #498, #48346 ) ;
#30725 = DIRECTION ( 'NONE',  ( 0.8124868780056783146, 0.000000000000000000, 0.5829794791144762289 ) ) ;
#30728 = ORIENTED_EDGE ( 'NONE', *, *, #29822, .T. ) ;
#30727 = DIRECTION ( 'NONE',  ( 1.043714542225393381E-14, 1.000000000000000000, -1.047444401652940007E-14 ) ) ;
#30726 = DIRECTION ( 'NONE',  ( 0.000000000000000000, -1.000000000000000000, -0.000000000000000000 ) ) ;
#30729 = ORIENTED_EDGE ( 'NONE', *, *, #38154, .F. ) ;
#30730 = CARTESIAN_POINT ( 'NONE',  ( -47.74129347246712740, -189.7472609257535510, -0.6749830015182022303 ) ) ;
#30731 = VERTEX_POINT ( 'NONE', #34817 ) ;
#30732 = PLANE ( 'NONE',  #3496 ) ;
#30733 = AXIS2_PLACEMENT_3D ( 'NONE', #18218, #14274, #17457 ) ;
#30734 = CARTESIAN_POINT ( 'NONE',  ( 72.05536924052414349, -175.3837268820161057, 33.11246405730899056 ) ) ;
#30735 = ORIENTED_EDGE ( 'NONE', *, *, #6740, .F. ) ;
#30736 = PRESENTATION_LAYER_ASSIGNMENT (  '', '', ( #1372 ) ) ;
#30737 = DIRECTION ( 'NONE',  ( 0.000000000000000000, 0.000000000000000000, 1.000000000000000000 ) ) ;
#30738 = FACE_OUTER_BOUND ( 'NONE', #29579, .T. ) ;
#30739 = PLANE ( 'NONE',  #25761 ) ;
#30740 = DIRECTION ( 'NONE',  ( 0.000000000000000000, 0.1205366802553233113, 0.9927088740980538617 ) ) ;
#30741 = AXIS2_PLACEMENT_3D ( 'NONE', #46476, #46738, #35403 ) ;
#30742 = VECTOR ( 'NONE', #10969, 1000.000000000000000 ) ;
#30743 = PLANE ( 'NONE',  #34118 ) ;
#30744 = ADVANCED_FACE ( 'NONE', ( #50616 ), #15392, .T. ) ;
#30745 = EDGE_CURVE ( 'NONE', #35288, #46710, #14353, .T. ) ;
#30746 = EDGE_LOOP ( 'NONE', ( #23278, #20069, #44556, #19797 ) ) ;
#30747 = ADVANCED_FACE ( 'NONE', ( #18305 ), #31401, .T. ) ;
#30748 = VECTOR ( 'NONE', #28656, 1000.000000000000000 ) ;
#30749 = LINE ( 'NONE', #11029, #36360 ) ;
#30750 = DIRECTION ( 'NONE',  ( 0.000000000000000000, -0.000000000000000000, -1.000000000000000000 ) ) ;
#30751 = EDGE_CURVE ( 'NONE', #43088, #121, #46944, .T. ) ;
#30752 = AXIS2_PLACEMENT_3D ( 'NONE', #48194, #44504, #4559 ) ;
#30753 = EDGE_CURVE ( 'NONE', #44939, #24499, #11331, .T. ) ;
#30754 = DIRECTION ( 'NONE',  ( 0.000000000000000000, 0.000000000000000000, -1.000000000000000000 ) ) ;
#30755 = ORIENTED_EDGE ( 'NONE', *, *, #19246, .F. ) ;
#30756 = PLANE ( 'NONE',  #42435 ) ;
#30757 = EDGE_CURVE ( 'NONE', #43961, #37405, #47446, .T. ) ;
#30758 = CARTESIAN_POINT ( 'NONE',  ( -48.24424070572787571, -183.6283474603465606, 0.9720229140804191870 ) ) ;
#30759 = EDGE_CURVE ( 'NONE', #4224, #23080, #6483, .T. ) ;
#30760 = CARTESIAN_POINT ( 'NONE',  ( -89.73513343757491612, -183.6283474603465606, -117.9955164924467397 ) ) ;
#30761 = CARTESIAN_POINT ( 'NONE',  ( -121.1142239062970276, -183.6283474603465606, 101.7307360698549417 ) ) ;
#30762 = LINE ( 'NONE', #27065, #8150 ) ;
#30763 = VERTEX_POINT ( 'NONE', #2523 ) ;
#30764 = EDGE_CURVE ( 'NONE', #34791, #18286, #14609, .T. ) ;
#30765 = EDGE_CURVE ( 'NONE', #8260, #29691, #22256, .T. ) ;
#30766 = VECTOR ( 'NONE', #24039, 1000.000000000000000 ) ;
#30767 = LINE ( 'NONE', #25131, #27900 ) ;
#30768 = AXIS2_PLACEMENT_3D ( 'NONE', #41884, #21663, #14035 ) ;
#30769 = EDGE_CURVE ( 'NONE', #3044, #30683, #18552, .T. ) ;
#30770 = CARTESIAN_POINT ( 'NONE',  ( -339.1964088526558498, -68.51134412508150717, 21.38919645685156112 ) ) ;
#30771 = CARTESIAN_POINT ( 'NONE',  ( -305.0000000000000568, -90.77207769297352513, -50.28800156563429624 ) ) ;
#30772 = AXIS2_PLACEMENT_3D ( 'NONE', #25781, #41815, #2391 ) ;
#30773 = EDGE_CURVE ( 'NONE', #17455, #47251, #10397, .T. ) ;
#30774 = ORIENTED_EDGE ( 'NONE', *, *, #32115, .F. ) ;
#30775 = LINE ( 'NONE', #26054, #20983 ) ;
#30776 = LINE ( 'NONE', #46307, #26312 ) ;
#30777 = ORIENTED_EDGE ( 'NONE', *, *, #39998, .F. ) ;
#30778 = AXIS2_PLACEMENT_3D ( 'NONE', #27643, #26608, #19490 ) ;
#30779 = ORIENTED_EDGE ( 'NONE', *, *, #9895, .F. ) ;
#30780 = VECTOR ( 'NONE', #31624, 1000.000000000000000 ) ;
#30781 = VERTEX_POINT ( 'NONE', #30617 ) ;
#30782 = FACE_OUTER_BOUND ( 'NONE', #28992, .T. ) ;
#30783 = AXIS2_PLACEMENT_3D ( 'NONE', #46078, #6381, #22404 ) ;
#30784 = AXIS2_PLACEMENT_3D ( 'NONE', #46346, #2451, #18479 ) ;
#30785 = DIRECTION ( 'NONE',  ( -0.3758275821142488260, 0.000000000000000000, 0.9266896074318291543 ) ) ;
#30786 = FACE_OUTER_BOUND ( 'NONE', #27107, .T. ) ;
#30787 = EDGE_LOOP ( 'NONE', ( #49107, #16304, #31575, #1322 ) ) ;
#30788 = ADVANCED_FACE ( 'NONE', ( #27464 ), #31146, .T. ) ;
#30789 = AXIS2_PLACEMENT_3D ( 'NONE', #24162, #23877, #48063 ) ;
#30790 = CARTESIAN_POINT ( 'NONE',  ( -339.1964088526558498, -102.1108035431478811, -54.98865587491830809 ) ) ;
#30791 = CARTESIAN_POINT ( 'NONE',  ( 47.91692961953209817, -193.5000000000000000, -77.99872144864701795 ) ) ;
#30794 = ORIENTED_EDGE ( 'NONE', *, *, #48206, .F. ) ;
#30793 = CARTESIAN_POINT ( 'NONE',  ( 75.95066919219054569, -193.5000000000000000, -11.92584929509534852 ) ) ;
#30792 = CARTESIAN_POINT ( 'NONE',  ( -157.4685091425930636, -189.7472609257535510, -59.13814366165043168 ) ) ;
#30795 = FACE_OUTER_BOUND ( 'NONE', #51820, .T. ) ;
#30796 = ORIENTED_EDGE ( 'NONE', *, *, #6675, .F. ) ;
#30797 = CARTESIAN_POINT ( 'NONE',  ( -330.4913330509368166, -144.3080463282014989, 56.27632902032097917 ) ) ;
#30798 = ORIENTED_EDGE ( 'NONE', *, *, #42140, .F. ) ;
#30799 = CARTESIAN_POINT ( 'NONE',  ( 75.17589904515342880, -189.7472609257535510, -18.28755301364250840 ) ) ;
#30800 = FACE_OUTER_BOUND ( 'NONE', #16581, .T. ) ;
#30801 = VERTEX_POINT ( 'NONE', #47192 ) ;
#30802 = ADVANCED_FACE ( 'NONE', ( #11171 ), #22230, .T. ) ;
#30803 = AXIS2_PLACEMENT_3D ( 'NONE', #47997, #11979, #40605 ) ;
#30804 = ORIENTED_EDGE ( 'NONE', *, *, #27851, .T. ) ;
#30805 = CARTESIAN_POINT ( 'NONE',  ( -7.223120065443615623, -193.5000000000000000, 117.9955164924470523 ) ) ;
#30806 = CIRCLE ( 'NONE', #47628, 60.00000000000000000 ) ;
#30807 = CARTESIAN_POINT ( 'NONE',  ( 32.49319223169170812, -189.7472609257535510, -95.22858582633060109 ) ) ;
#30808 = EDGE_LOOP ( 'NONE', ( #1665, #38608, #48495, #14151 ) ) ;
#30809 = DIRECTION ( 'NONE',  ( 0.000000000000000000, -0.000000000000000000, 1.000000000000000000 ) ) ;
#30810 = VECTOR ( 'NONE', #15591, 1000.000000000000000 ) ;
#30811 = DIRECTION ( 'NONE',  ( -0.1768902751225592818, 0.000000000000000000, -0.9842305779475992722 ) ) ;
#30812 = ADVANCED_FACE ( 'NONE', ( #46416 ), #42731, .F. ) ;
#30813 = EDGE_CURVE ( 'NONE', #3759, #41311, #39297, .T. ) ;
#30814 = ORIENTED_EDGE ( 'NONE', *, *, #37537, .F. ) ;
#30815 = EDGE_CURVE ( 'NONE', #16981, #30632, #2271, .T. ) ;
#30816 = CARTESIAN_POINT ( 'NONE',  ( -339.1964088526558498, -178.4886558749184076, -21.38919645685194837 ) ) ;
#30817 = DIRECTION ( 'NONE',  ( 0.000000000000000000, -3.491481338843133355E-15, -1.000000000000000000 ) ) ;
#30818 = ADVANCED_FACE ( 'NONE', ( #35596 ), #51926, .T. ) ;
#30819 = ORIENTED_EDGE ( 'NONE', *, *, #5692, .T. ) ;
#30820 = DIRECTION ( 'NONE',  ( -0.000000000000000000, -0.8854560256532126861, -0.4647231720437631775 ) ) ;
#30821 = ORIENTED_EDGE ( 'NONE', *, *, #9188, .T. ) ;
#30822 = CIRCLE ( 'NONE', #48464, 60.00000000000000000 ) ;
#30823 = DIRECTION ( 'NONE',  ( 0.000000000000000000, -0.2393156642875652051, -0.9709418174260502354 ) ) ;
#30824 = VECTOR ( 'NONE', #26906, 999.9999999999998863 ) ;
#30825 = DIRECTION ( 'NONE',  ( 1.043714542225393223E-14, 0.9927088740980551940, 0.1205366802553130001 ) ) ;
#30826 = EDGE_LOOP ( 'NONE', ( #45522, #52023, #39590, #41862 ) ) ;
#30827 = AXIS2_PLACEMENT_3D ( 'NONE', #7789, #35911, #3073 ) ;
#30828 = DIRECTION ( 'NONE',  ( 0.000000000000000000, 1.000000000000000000, 0.000000000000000000 ) ) ;
#30829 = CARTESIAN_POINT ( 'NONE',  ( -336.3521761649654422, -180.1556192733800117, 16.67542351306693149 ) ) ;
#30830 = DIRECTION ( 'NONE',  ( 0.4566292373937077542, 0.000000000000000000, 0.8896570909947499883 ) ) ;
#30831 = AXIS2_PLACEMENT_3D ( 'NONE', #327, #1379, #16374 ) ;
#30832 = EDGE_CURVE ( 'NONE', #1307, #10059, #15655, .T. ) ;
#30833 = ORIENTED_EDGE ( 'NONE', *, *, #14695, .F. ) ;
#30835 = AXIS2_PLACEMENT_3D ( 'NONE', #2429, #42872, #35240 ) ;
#30834 = LINE ( 'NONE', #5646, #46385 ) ;
#30836 = EDGE_CURVE ( 'NONE', #51603, #14259, #21006, .T. ) ;
#30837 = CARTESIAN_POINT ( 'NONE',  ( -48.47912675150885065, -188.5000000000000284, 6.938893903907228378E-15 ) ) ;
#30838 = DIRECTION ( 'NONE',  ( -0.000000000000000000, 1.000000000000000000, -0.000000000000000000 ) ) ;
#30840 = VERTEX_POINT ( 'NONE', #15915 ) ;
#30839 = CARTESIAN_POINT ( 'NONE',  ( -339.1964088526558498, -178.4886558749180949, 21.38919645685277970 ) ) ;
#30841 = EDGE_CURVE ( 'NONE', #30907, #13637, #27719, .T. ) ;
#30842 = ORIENTED_EDGE ( 'NONE', *, *, #27851, .F. ) ;
#30843 = CARTESIAN_POINT ( 'NONE',  ( 61.38599058177057799, -175.3837268820161057, 59.62093586438192006 ) ) ;
#30844 = EDGE_CURVE ( 'NONE', #41127, #27780, #3810, .T. ) ;
#30845 = LINE ( 'NONE', #46892, #7818 ) ;
#30846 = VECTOR ( 'NONE', #2244, 1000.000000000000114 ) ;
#30847 = VECTOR ( 'NONE', #10768, 1000.000000000000000 ) ;
#30848 = VERTEX_POINT ( 'NONE', #48226 ) ;
#30849 = LINE ( 'NONE', #6931, #49971 ) ;
#30850 = ORIENTED_EDGE ( 'NONE', *, *, #35555, .F. ) ;
#30851 = CARTESIAN_POINT ( 'NONE',  ( -339.1964088526558498, -116.8846903019852164, -58.63009191191289915 ) ) ;
#30852 = CARTESIAN_POINT ( 'NONE',  ( -48.47912675150885065, -183.6283474603465606, 6.938893903907228378E-15 ) ) ;
#30853 = AXIS2_PLACEMENT_3D ( 'NONE', #24834, #3830, #8026 ) ;
#30854 = DIRECTION ( 'NONE',  ( 0.000000000000000000, 0.000000000000000000, 1.000000000000000000 ) ) ;
#30855 = PLANE ( 'NONE',  #39997 ) ;
#30856 = ORIENTED_EDGE ( 'NONE', *, *, #17844, .T. ) ;
#30857 = EDGE_LOOP ( 'NONE', ( #22078, #47905, #28459, #44087 ) ) ;
#30858 = VERTEX_POINT ( 'NONE', #44283 ) ;
#30859 = EDGE_CURVE ( 'NONE', #47574, #12090, #24046, .T. ) ;
#30860 = PLANE ( 'NONE',  #21606 ) ;
#30861 = CARTESIAN_POINT ( 'NONE',  ( -47.66663987350317910, -177.1207230881787780, 0.5829794791144832233 ) ) ;
#30862 = CIRCLE ( 'NONE', #19937, 125.0000000000000000 ) ;
#30863 = CARTESIAN_POINT ( 'NONE',  ( -98.10897907742933910, -193.5000000000000000, 114.7252272087849434 ) ) ;
#30864 = CIRCLE ( 'NONE', #28220, 20.00000000000001776 ) ;
#30865 = DIRECTION ( 'NONE',  ( 0.000000000000000000, 1.000000000000000000, 0.000000000000000000 ) ) ;
#30866 = LINE ( 'NONE', #14072, #35619 ) ;
#30867 = ORIENTED_EDGE ( 'NONE', *, *, #989, .F. ) ;
#30868 = FACE_OUTER_BOUND ( 'NONE', #30826, .T. ) ;
#30869 = CARTESIAN_POINT ( 'NONE',  ( -166.1003692892502102, -193.5000000000000000, -42.31126686685032467 ) ) ;
#30870 = VECTOR ( 'NONE', #40403, 1000.000000000000000 ) ;
#30871 = ORIENTED_EDGE ( 'NONE', *, *, #32453, .F. ) ;
#30872 = ORIENTED_EDGE ( 'NONE', *, *, #23117, .F. ) ;
#30873 = CARTESIAN_POINT ( 'NONE',  ( -238.7407812814481076, -193.5000000000000000, 41.45482488023466772 ) ) ;
#30874 = DIRECTION ( 'NONE',  ( 0.000000000000000000, -1.000000000000000000, 0.000000000000000000 ) ) ;
#30875 = CARTESIAN_POINT ( 'NONE',  ( 48.47907891923915003, -189.7472609257535510, 78.89300572996904748 ) ) ;
#30876 = DIRECTION ( 'NONE',  ( 1.000000000000000000, -0.000000000000000000, -0.000000000000000000 ) ) ;
#30877 = LINE ( 'NONE', #19055, #36301 ) ;
#30878 = EDGE_CURVE ( 'NONE', #42173, #26071, #19581, .T. ) ;
#30880 = EDGE_CURVE ( 'NONE', #17876, #11338, #24445, .T. ) ;
#30879 = DIRECTION ( 'NONE',  ( -0.000000000000000000, 1.000000000000000000, -0.000000000000000000 ) ) ;
#30881 = VERTEX_POINT ( 'NONE', #24306 ) ;
#30882 = FACE_OUTER_BOUND ( 'NONE', #34628, .T. ) ;
#30883 = ORIENTED_EDGE ( 'NONE', *, *, #43217, .T. ) ;
#30884 = LINE ( 'NONE', #49833, #27915 ) ;
#30885 = AXIS2_PLACEMENT_3D ( 'NONE', #18727, #10841, #26855 ) ;
#30886 = VECTOR ( 'NONE', #41405, 1000.000000000000000 ) ;
#30887 = CARTESIAN_POINT ( 'NONE',  ( -336.3521761649654422, -97.52665284734005979, -53.00046796564681983 ) ) ;
#30888 = ORIENTED_EDGE ( 'NONE', *, *, #7626, .F. ) ;
#30889 = AXIS2_PLACEMENT_3D ( 'NONE', #45530, #45019, #5595 ) ;
#30890 = DIRECTION ( 'NONE',  ( -0.5085311186492273983, 0.000000000000000000, 0.8610436117673514467 ) ) ;
#30891 = PLANE ( 'NONE',  #13832 ) ;
#30892 = LINE ( 'NONE', #10917, #46671 ) ;
#30893 = CARTESIAN_POINT ( 'NONE',  ( -339.1964088526558498, -162.9117225908384796, 45.24064679492099117 ) ) ;
#30894 = LINE ( 'NONE', #50876, #47145 ) ;
#30895 = VERTEX_POINT ( 'NONE', #31923 ) ;
#30896 = CIRCLE ( 'NONE', #16655, 4.999999999999997335 ) ;
#30897 = EDGE_CURVE ( 'NONE', #45491, #49617, #40572, .T. ) ;
#30898 = DIRECTION ( 'NONE',  ( 0.000000000000000000, -0.000000000000000000, 1.000000000000000000 ) ) ;
#30900 = EDGE_LOOP ( 'NONE', ( #1716, #34184, #18963, #24745 ) ) ;
#30899 = FACE_OUTER_BOUND ( 'NONE', #38084, .T. ) ;
#30901 = ORIENTED_EDGE ( 'NONE', *, *, #26615, .T. ) ;
#30902 = CARTESIAN_POINT ( 'NONE',  ( 41.41233698655026529, -177.1207230881787780, 86.85922373029363541 ) ) ;
#30903 = ORIENTED_EDGE ( 'NONE', *, *, #12656, .F. ) ;
#30904 = ADVANCED_FACE ( 'NONE', ( #11942 ), #27979, .T. ) ;
#30905 = AXIS2_PLACEMENT_3D ( 'NONE', #25193, #8116, #40948 ) ;
#30906 = DIRECTION ( 'NONE',  ( -1.000000000000000000, 0.000000000000000000, 0.000000000000000000 ) ) ;
#30907 = VERTEX_POINT ( 'NONE', #4587 ) ;
#30908 = CARTESIAN_POINT ( 'NONE',  ( -46.00000000000000711, 20.00000000000000000, 41.00000000000000000 ) ) ;
#30909 = DIRECTION ( 'NONE',  ( 1.000000000000000000, 0.000000000000000000, 0.000000000000000000 ) ) ;
#30910 = VERTEX_POINT ( 'NONE', #36381 ) ;
#30911 = PLANE ( 'NONE',  #22427 ) ;
#30912 = CARTESIAN_POINT ( 'NONE',  ( -336.3521761649654422, -104.1045282520827300, -55.74477592174792306 ) ) ;
#30913 = DIRECTION ( 'NONE',  ( 0.8896570909947499883, 0.000000000000000000, -0.4566292373937077542 ) ) ;
#30914 = ORIENTED_EDGE ( 'NONE', *, *, #33781, .T. ) ;
#30915 = ORIENTED_EDGE ( 'NONE', *, *, #42927, .T. ) ;
#30916 = ORIENTED_EDGE ( 'NONE', *, *, #50645, .F. ) ;
#30917 = DIRECTION ( 'NONE',  ( -0.000000000000000000, 1.000000000000000000, -0.000000000000000000 ) ) ;
#30918 = DIRECTION ( 'NONE',  ( -1.000000000000000000, 0.000000000000000000, -0.000000000000000000 ) ) ;
#30919 = VECTOR ( 'NONE', #11924, 1000.000000000000000 ) ;
#30920 = AXIS2_PLACEMENT_3D ( 'NONE', #8149, #24188, #12601 ) ;
#30921 = FACE_OUTER_BOUND ( 'NONE', #39792, .T. ) ;
#30922 = DIRECTION ( 'NONE',  ( 0.000000000000000000, 1.000000000000000000, 0.000000000000000000 ) ) ;
#30923 = CARTESIAN_POINT ( 'NONE',  ( -330.4913330509368166, -66.09477493971897388, 13.63415328425216622 ) ) ;
#30924 = ORIENTED_EDGE ( 'NONE', *, *, #10219, .T. ) ;
#30925 = VECTOR ( 'NONE', #23164, 1000.000000000000000 ) ;
#30926 = CARTESIAN_POINT ( 'NONE',  ( -170.7514454179067798, -193.5000000000000000, -20.63201007055400282 ) ) ;
#30927 = ORIENTED_EDGE ( 'NONE', *, *, #35320, .F. ) ;
#30929 = ORIENTED_EDGE ( 'NONE', *, *, #15630, .F. ) ;
#30928 = CARTESIAN_POINT ( 'NONE',  ( -37.78865854180983774, -193.5000000000000000, -123.5388265266451242 ) ) ;
#30930 = VECTOR ( 'NONE', #12555, 1000.000000000000227 ) ;
#30931 = ORIENTED_EDGE ( 'NONE', *, *, #47380, .T. ) ;
#30932 = CARTESIAN_POINT ( 'NONE',  ( -137.9639882952644143, -177.1207230881787780, 87.27805883780241913 ) ) ;
#30933 = DIRECTION ( 'NONE',  ( 0.000000000000000000, 0.000000000000000000, 1.000000000000000000 ) ) ;
#30934 = DIRECTION ( 'NONE',  ( 0.000000000000000000, 0.6631226582407937498, -0.7485107481711024136 ) ) ;
#30935 = ADVANCED_FACE ( 'NONE', ( #8012 ), #32184, .T. ) ;
#30936 = CARTESIAN_POINT ( 'NONE',  ( -124.9871112439422092, -189.7472609257535510, -98.85104101073275729 ) ) ;
#30937 = ORIENTED_EDGE ( 'NONE', *, *, #34012, .F. ) ;
#30938 = CARTESIAN_POINT ( 'NONE',  ( -47.48307690889363641, -177.1207230881787780, -0.08879589532292464504 ) ) ;
#30939 = ORIENTED_EDGE ( 'NONE', *, *, #39163, .T. ) ;
#30940 = AXIS2_PLACEMENT_3D ( 'NONE', #10961, #15439, #43790 ) ;
#30941 = ORIENTED_EDGE ( 'NONE', *, *, #46397, .F. ) ;
#30942 = DIRECTION ( 'NONE',  ( -1.000000000000000000, 0.000000000000000000, 0.000000000000000000 ) ) ;
#30943 = CARTESIAN_POINT ( 'NONE',  ( -105.8382074681672975, -175.3837268820161057, -109.9360785596604728 ) ) ;
#30944 = LINE ( 'NONE', #4064, #15683 ) ;
#30945 = VERTEX_POINT ( 'NONE', #656 ) ;
#30946 = CARTESIAN_POINT ( 'NONE',  ( -164.3791542526839180, -193.5000000000000000, 46.82076062204521349 ) ) ;
#30947 = DIRECTION ( 'NONE',  ( 0.000000000000000000, 0.000000000000000000, 1.000000000000000000 ) ) ;
#30948 = CARTESIAN_POINT ( 'NONE',  ( -5.142695285147754980, -193.5000000000000000, -116.1806952091177578 ) ) ;
#30949 = CARTESIAN_POINT ( 'NONE',  ( 12.99855592850622799, -183.6283474603465606, 108.8370090194295017 ) ) ;
#30950 = ORIENTED_EDGE ( 'NONE', *, *, #18302, .T. ) ;
#30951 = CARTESIAN_POINT ( 'NONE',  ( -11.47118876952529121, -193.5000000000000000, 118.3487137068149053 ) ) ;
#30952 = PLANE ( 'NONE',  #8075 ) ;
#30953 = LINE ( 'NONE', #30429, #31602 ) ;
#30954 = PRODUCT_DEFINITION_FORMATION_WITH_SPECIFIED_SOURCE ( 'ANY', '', #26430, .NOT_KNOWN. ) ;
#30955 = ORIENTED_EDGE ( 'NONE', *, *, #12613, .T. ) ;
#30956 = VECTOR ( 'NONE', #34116, 1000.000000000000000 ) ;
#30957 = AXIS2_PLACEMENT_3D ( 'NONE', #991, #17565, #1244 ) ;
#30958 = EDGE_CURVE ( 'NONE', #5217, #50146, #4328, .T. ) ;
#30959 = LINE ( 'NONE', #47002, #2940 ) ;
#30960 = VECTOR ( 'NONE', #1049, 1000.000000000000000 ) ;
#30961 = DIRECTION ( 'NONE',  ( -1.000000000000000000, -0.000000000000000000, -0.000000000000000000 ) ) ;
#30962 = ORIENTED_EDGE ( 'NONE', *, *, #20503, .T. ) ;
#30963 = LINE ( 'NONE', #18866, #48937 ) ;
#30964 = EDGE_LOOP ( 'NONE', ( #36981, #51050, #34490, #41930 ) ) ;
#30965 = VECTOR ( 'NONE', #8594, 1000.000000000000114 ) ;
#30966 = PLANE ( 'NONE',  #36846 ) ;
#30967 = FACE_BOUND ( 'NONE', #16164, .T. ) ;
#30968 = CARTESIAN_POINT ( 'NONE',  ( -170.6250538923603131, -193.5000000000000000, 26.55884942729649723 ) ) ;
#30969 = CARTESIAN_POINT ( 'NONE',  ( -169.0136227435421006, -175.3837268820161057, -33.11246405730812370 ) ) ;
#30970 = VERTEX_POINT ( 'NONE', #32448 ) ;
#30971 = CIRCLE ( 'NONE', #1651, 125.0000000000000000 ) ;
#30972 = VERTEX_POINT ( 'NONE', #12468 ) ;
#30973 = FACE_OUTER_BOUND ( 'NONE', #9714, .T. ) ;
#30974 = VERTEX_POINT ( 'NONE', #28489 ) ;
#30975 = CYLINDRICAL_SURFACE ( 'NONE', #20884, 125.0000000000000000 ) ;
#30976 = EDGE_CURVE ( 'NONE', #39640, #17102, #44536, .T. ) ;
#30977 = EDGE_CURVE ( 'NONE', #48594, #4839, #40256, .T. ) ;
#30978 = PLANE ( 'NONE',  #9134 ) ;
#30979 = LINE ( 'NONE', #47024, #4649 ) ;
#30980 = VERTEX_POINT ( 'NONE', #3548 ) ;
#30983 = ORIENTED_EDGE ( 'NONE', *, *, #2080, .T. ) ;
#30982 = CARTESIAN_POINT ( 'NONE',  ( -25.55153130240594450, -175.3837268820161057, 122.8793122007210599 ) ) ;
#30981 = FACE_OUTER_BOUND ( 'NONE', #23842, .T. ) ;
#30984 = VECTOR ( 'NONE', #18628, 1000.000000000000000 ) ;
#30985 = CARTESIAN_POINT ( 'NONE',  ( -138.3705904895685705, -193.5000000000000000, -86.85922373029296750 ) ) ;
#30986 = ORIENTED_EDGE ( 'NONE', *, *, #16324, .T. ) ;
#30987 = CARTESIAN_POINT ( 'NONE',  ( 52.98246549829696761, -175.3837268820161057, 73.01058346660533971 ) ) ;
#30988 = AXIS2_PLACEMENT_3D ( 'NONE', #36676, #20640, #4890 ) ;
#30989 = ORIENTED_EDGE ( 'NONE', *, *, #8869, .F. ) ;
#30990 = ADVANCED_FACE ( 'NONE', ( #36913 ), #33220, .F. ) ;
#30991 = DIRECTION ( 'NONE',  ( 0.000000000000000000, 0.000000000000000000, 1.000000000000000000 ) ) ;
#30992 = ORIENTED_EDGE ( 'NONE', *, *, #32595, .F. ) ;
#30995 = ORIENTED_EDGE ( 'NONE', *, *, #27606, .T. ) ;
#30994 = CARTESIAN_POINT ( 'NONE',  ( -84.19171550243319757, -175.3837268820161057, 119.7898618611247628 ) ) ;
#30993 = CARTESIAN_POINT ( 'NONE',  ( -48.47912675150885065, -175.3837268820161057, 6.938893903907228378E-15 ) ) ;
#30996 = ORIENTED_EDGE ( 'NONE', *, *, #9880, .T. ) ;
#30997 = EDGE_CURVE ( 'NONE', #11130, #49730, #17481, .T. ) ;
#30998 = CARTESIAN_POINT ( 'NONE',  ( 49.27559354810669134, -193.5000000000000000, -76.29032973288636299 ) ) ;
#30999 = ORIENTED_EDGE ( 'NONE', *, *, #661, .T. ) ;
#31000 = DIRECTION ( 'NONE',  ( 1.000000000000000000, 0.000000000000000000, -0.000000000000000000 ) ) ;
#31001 = EDGE_CURVE ( 'NONE', #28894, #18907, #25098, .T. ) ;
#31002 = CARTESIAN_POINT ( 'NONE',  ( 21.21056010634072564, -193.5000000000000000, 103.7706487676302061 ) ) ;
#31003 = ORIENTED_EDGE ( 'NONE', *, *, #48755, .T. ) ;
#31004 = CARTESIAN_POINT ( 'NONE',  ( -172.4422607493951602, -183.6283474603465606, 16.06677968424543934 ) ) ;
#31005 = CARTESIAN_POINT ( 'NONE',  ( -330.4913330509368166, -67.22367097967895688, 20.80804632820126443 ) ) ;
#31006 = FACE_OUTER_BOUND ( 'NONE', #39991, .T. ) ;
#31007 = PLANE ( 'NONE',  #5585 ) ;
#31008 = ORIENTED_EDGE ( 'NONE', *, *, #39458, .F. ) ;
#31009 = DIRECTION ( 'NONE',  ( 0.000000000000000000, 0.000000000000000000, -1.000000000000000000 ) ) ;
#31010 = DIRECTION ( 'NONE',  ( -0.8757349421956310831, 0.000000000000000000, -0.4827922027307550712 ) ) ;
#31011 = AXIS2_PLACEMENT_3D ( 'NONE', #37977, #5687, #41661 ) ;
#31012 = CARTESIAN_POINT ( 'NONE',  ( 71.09073365861578964, -175.3837268820161057, 32.84887689123991095 ) ) ;
#31013 = ORIENTED_EDGE ( 'NONE', *, *, #31999, .F. ) ;
#31014 = DIRECTION ( 'NONE',  ( 0.000000000000000000, 0.000000000000000000, -1.000000000000000000 ) ) ;
#31015 = CARTESIAN_POINT ( 'NONE',  ( -118.1688136093591908, -175.3837268820161057, -103.7706487676296661 ) ) ;
#31016 = DIRECTION ( 'NONE',  ( -0.000000000000000000, 0.4647231720437789981, 0.8854560256532044704 ) ) ;
#31017 = LINE ( 'NONE', #23643, #45397 ) ;
#31018 = CARTESIAN_POINT ( 'NONE',  ( -49.42645310536304493, -193.5000000000000000, 0.3202698538628349079 ) ) ;
#31019 = EDGE_LOOP ( 'NONE', ( #30480, #983, #19700, #1028 ) ) ;
#31020 = FACE_OUTER_BOUND ( 'NONE', #48619, .T. ) ;
#31021 = LINE ( 'NONE', #6859, #27383 ) ;
#31022 = CIRCLE ( 'NONE', #24314, 60.00000000000000000 ) ;
#31023 = DIRECTION ( 'NONE',  ( 0.1768902751225733261, 0.000000000000000000, -0.9842305779475966077 ) ) ;
#31024 = PLANE ( 'NONE',  #42177 ) ;
#31025 = DIRECTION ( 'NONE',  ( 0.000000000000000000, 1.000000000000000000, -0.000000000000000000 ) ) ;
#31026 = ORIENTED_EDGE ( 'NONE', *, *, #46490, .F. ) ;
#31027 = DIRECTION ( 'NONE',  ( -0.000000000000000000, 1.000000000000000000, 0.000000000000000000 ) ) ;
#31028 = CARTESIAN_POINT ( 'NONE',  ( 0.7476021451244497795, -175.3837268820161057, -113.8100815915415609 ) ) ;
#31029 = ORIENTED_EDGE ( 'NONE', *, *, #24697, .F. ) ;
#31030 = VERTEX_POINT ( 'NONE', #12978 ) ;
#31031 = ORIENTED_EDGE ( 'NONE', *, *, #30691, .T. ) ;
#31032 = DIRECTION ( 'NONE',  ( -0.000000000000000000, 0.3546048870425331789, -0.9350162426854158326 ) ) ;
#31033 = EDGE_CURVE ( 'NONE', #46014, #46919, #37761, .T. ) ;
#31034 = ADVANCED_FACE ( 'NONE', ( #37160 ), #13775, .T. ) ;
#31035 = DIRECTION ( 'NONE',  ( -0.000000000000000000, -1.000000000000000000, -0.000000000000000000 ) ) ;
#31036 = ORIENTED_EDGE ( 'NONE', *, *, #27417, .F. ) ;
#31037 = VECTOR ( 'NONE', #21996, 1000.000000000000000 ) ;
#31038 = VECTOR ( 'NONE', #33742, 1000.000000000000000 ) ;
#31039 = CARTESIAN_POINT ( 'NONE',  ( -332.3517673607765914, -81.08339623743702873, -41.09453333279329712 ) ) ;
#31040 = LINE ( 'NONE', #19721, #45395 ) ;
#31043 = EDGE_LOOP ( 'NONE', ( #16718, #41781, #44427, #37039 ) ) ;
#31042 = CARTESIAN_POINT ( 'NONE',  ( -18.31235070009513421, -175.3837268820161057, 121.3052580173829966 ) ) ;
#31041 = DIRECTION ( 'NONE',  ( -0.000000000000000000, 1.000000000000000000, -0.000000000000000000 ) ) ;
#31044 = ADVANCED_FACE ( 'NONE', ( #1690 ), #5650, .F. ) ;
#31045 = PLANE ( 'NONE',  #8798 ) ;
#31046 = VERTEX_POINT ( 'NONE', #5380 ) ;
#31047 = FACE_OUTER_BOUND ( 'NONE', #4607, .T. ) ;
#31048 = EDGE_LOOP ( 'NONE', ( #25416, #8057, #50272, #1312, #16651, #4287 ) ) ;
#31049 = LINE ( 'NONE', #14786, #1416 ) ;
#31050 = EDGE_CURVE ( 'NONE', #22956, #47477, #31156, .T. ) ;
#31051 = LINE ( 'NONE', #11328, #2801 ) ;
#31053 = DIRECTION ( 'NONE',  ( 0.000000000000000000, 0.8854560256532157947, 0.4647231720437573488 ) ) ;
#31052 = DIRECTION ( 'NONE',  ( 0.1768902751225733261, 0.000000000000000000, -0.9842305779475966077 ) ) ;
#31054 = VERTEX_POINT ( 'NONE', #50043 ) ;
#31055 = EDGE_CURVE ( 'NONE', #8505, #15290, #899, .T. ) ;
#31056 = LINE ( 'NONE', #43417, #50012 ) ;
#31057 = ORIENTED_EDGE ( 'NONE', *, *, #44948, .F. ) ;
#31058 = CARTESIAN_POINT ( 'NONE',  ( -155.9608607592036833, -177.1207230881787780, 63.81752780153064464 ) ) ;
#31059 = EDGE_CURVE ( 'NONE', #36633, #51798, #6719, .T. ) ;
#31061 = VECTOR ( 'NONE', #514, 1000.000000000000000 ) ;
#31060 = DIRECTION ( 'NONE',  ( -0.000000000000000000, 1.000000000000000000, -0.000000000000000000 ) ) ;
#31062 = EDGE_LOOP ( 'NONE', ( #23583, #46565, #5185, #39888 ) ) ;
#31063 = DIRECTION ( 'NONE',  ( -0.03686245026030504635, 0.000000000000000000, 0.9993203489176064602 ) ) ;
#31064 = CARTESIAN_POINT ( 'NONE',  ( -84.19171550243321178, -189.7472609257535510, 119.7898618611247485 ) ) ;
#31065 = EDGE_CURVE ( 'NONE', #77, #36042, #8781, .T. ) ;
#31066 = VERTEX_POINT ( 'NONE', #5123 ) ;
#31067 = LINE ( 'NONE', #27116, #20033 ) ;
#31068 = DIRECTION ( 'NONE',  ( -0.000000000000000000, 1.000000000000000000, -0.000000000000000000 ) ) ;
#31069 = VERTEX_POINT ( 'NONE', #9838 ) ;
#31070 = FACE_OUTER_BOUND ( 'NONE', #30078, .T. ) ;
#31071 = ORIENTED_EDGE ( 'NONE', *, *, #51034, .F. ) ;
#31072 = CARTESIAN_POINT ( 'NONE',  ( -18.95304271317703382, -189.7472609257535510, -121.4627941443854837 ) ) ;
#31073 = CARTESIAN_POINT ( 'NONE',  ( -47.47956591500005885, -183.6283474603465606, -0.02963332782254939762 ) ) ;
#31074 = EDGE_LOOP ( 'NONE', ( #23158, #17466, #36328, #24287 ) ) ;
#31075 = CARTESIAN_POINT ( 'NONE',  ( 74.60098876342242136, -193.5000000000000000, 21.82395850507348811 ) ) ;
#31076 = DIRECTION ( 'NONE',  ( 1.000000000000000000, 5.781354811211875074E-17, 6.525800561034969538E-17 ) ) ;
#31077 = CARTESIAN_POINT ( 'NONE',  ( -336.3521761649654422, -153.2494431741581025, -51.01861988938816950 ) ) ;
#31078 = AXIS2_PLACEMENT_3D ( 'NONE', #30861, #26905, #30333 ) ;
#31079 = AXIS2_PLACEMENT_3D ( 'NONE', #23963, #39980, #4008 ) ;
#31080 = CARTESIAN_POINT ( 'NONE',  ( -48.47912675150885065, -183.6283474603465606, 6.938893903907228378E-15 ) ) ;
#31081 = EDGE_CURVE ( 'NONE', #48517, #29101, #32953, .T. ) ;
#31082 = DIRECTION ( 'NONE',  ( -1.000000000000000000, -0.000000000000000000, -0.000000000000000000 ) ) ;
#31083 = CARTESIAN_POINT ( 'NONE',  ( -339.1964088526558498, -79.00630452878414189, 38.74998146212082162 ) ) ;
#31085 = ORIENTED_EDGE ( 'NONE', *, *, #34593, .T. ) ;
#31084 = CARTESIAN_POINT ( 'NONE',  ( 76.31829002442924548, -177.1207230881787780, 7.113702696402421033 ) ) ;
#31086 = ORIENTED_EDGE ( 'NONE', *, *, #23696, .T. ) ;
#31087 = LINE ( 'NONE', #47134, #39171 ) ;
#31088 = EDGE_CURVE ( 'NONE', #12031, #18822, #14043, .T. ) ;
#31089 = PLANE ( 'NONE',  #31295 ) ;
#31090 = ORIENTED_EDGE ( 'NONE', *, *, #34380, .F. ) ;
#31091 = ORIENTED_EDGE ( 'NONE', *, *, #43461, .T. ) ;
#31092 = VECTOR ( 'NONE', #38847, 1000.000000000000000 ) ;
#31093 = CARTESIAN_POINT ( 'NONE',  ( -48.18706998087188254, -183.6283474603465606, 0.9564009842765313074 ) ) ;
#31094 = VERTEX_POINT ( 'NONE', #44799 ) ;
#31095 = DIRECTION ( 'NONE',  ( 0.000000000000000000, -1.000000000000000000, 0.000000000000000000 ) ) ;
#31096 = FACE_OUTER_BOUND ( 'NONE', #22466, .T. ) ;
#31097 = EDGE_CURVE ( 'NONE', #51539, #49907, #9323, .T. ) ;
#31098 = EDGE_CURVE ( 'NONE', #40297, #22314, #21397, .T. ) ;
#31099 = EDGE_CURVE ( 'NONE', #14253, #32264, #49538, .T. ) ;
#31100 = EDGE_CURVE ( 'NONE', #31730, #23257, #41110, .T. ) ;
#31101 = DIRECTION ( 'NONE',  ( -1.000000000000000000, -0.000000000000000000, -0.000000000000000000 ) ) ;
#31102 = PLANE ( 'NONE',  #45927 ) ;
#31103 = ORIENTED_EDGE ( 'NONE', *, *, #38838, .T. ) ;
#31104 = ORIENTED_EDGE ( 'NONE', *, *, #23750, .T. ) ;
#31105 = EDGE_CURVE ( 'NONE', #16426, #18623, #5906, .T. ) ;
#31106 = ORIENTED_EDGE ( 'NONE', *, *, #48461, .T. ) ;
#31107 = DIRECTION ( 'NONE',  ( -0.000000000000000000, 1.047444401652940007E-14, 1.000000000000000000 ) ) ;
#31108 = CARTESIAN_POINT ( 'NONE',  ( 55.03325008324586776, -193.5000000000000000, -70.07273251429357686 ) ) ;
#31109 = DIRECTION ( 'NONE',  ( -0.000000000000000000, 0.6631226582407937498, -0.7485107481711024136 ) ) ;
#31110 = EDGE_CURVE ( 'NONE', #3616, #10162, #45074, .T. ) ;
#31111 = PLANE ( 'NONE',  #45518 ) ;
#31112 = DIRECTION ( 'NONE',  ( 1.043714542225393854E-14, -0.6631226582407965253, -0.7485107481711000821 ) ) ;
#31113 = ORIENTED_EDGE ( 'NONE', *, *, #20996, .F. ) ;
#31114 = AXIS2_PLACEMENT_3D ( 'NONE', #6147, #25575, #5894 ) ;
#31115 = EDGE_CURVE ( 'NONE', #38032, #39795, #6921, .T. ) ;
#31116 = PLANE ( 'NONE',  #18941 ) ;
#31117 = FACE_OUTER_BOUND ( 'NONE', #22949, .T. ) ;
#31118 = EDGE_CURVE ( 'NONE', #28891, #150, #22953, .T. ) ;
#31119 = VECTOR ( 'NONE', #48086, 1000.000000000000227 ) ;
#31120 = ORIENTED_EDGE ( 'NONE', *, *, #25581, .F. ) ;
#31121 = ORIENTED_EDGE ( 'NONE', *, *, #51246, .T. ) ;
#31122 = FACE_OUTER_BOUND ( 'NONE', #3387, .T. ) ;
#31123 = DIRECTION ( 'NONE',  ( 0.3482016354343866471, 0.000000000000000000, 0.9374196611341253371 ) ) ;
#31124 = EDGE_CURVE ( 'NONE', #4082, #38866, #5903, .T. ) ;
#31125 = CARTESIAN_POINT ( 'NONE',  ( -60.86541030502395699, -183.6283474603465606, -124.3848060646151481 ) ) ;
#31126 = DIRECTION ( 'NONE',  ( 1.043714542225393381E-14, 0.1205366802553303057, 0.9927088740980530845 ) ) ;
#31127 = ADVANCED_FACE ( 'NONE', ( #10345 ), #38460, .F. ) ;
#31128 = LINE ( 'NONE', #43732, #38811 ) ;
#31129 = CARTESIAN_POINT ( 'NONE',  ( -173.4787860028527007, -193.5000000000000000, 0.2918682030023981300 ) ) ;
#31130 = ORIENTED_EDGE ( 'NONE', *, *, #48451, .T. ) ;
#31131 = DIRECTION ( 'NONE',  ( 0.000000000000000000, 1.000000000000000000, 0.000000000000000000 ) ) ;
#31132 = ADVANCED_FACE ( 'NONE', ( #6672 ), #18498, .F. ) ;
#31133 = ORIENTED_EDGE ( 'NONE', *, *, #36926, .T. ) ;
#31134 = FACE_OUTER_BOUND ( 'NONE', #44668, .T. ) ;
#31135 = VECTOR ( 'NONE', #42746, 1000.000000000000000 ) ;
#31136 = DIRECTION ( 'NONE',  ( -0.4566292373937077542, 0.000000000000000000, -0.8896570909947499883 ) ) ;
#31137 = EDGE_LOOP ( 'NONE', ( #36494, #4540, #13468, #5610 ) ) ;
#31138 = DIRECTION ( 'NONE',  ( 0.000000000000000000, -0.000000000000000000, -1.000000000000000000 ) ) ;
#31139 = DIRECTION ( 'NONE',  ( 0.000000000000000000, 1.000000000000000000, 0.000000000000000000 ) ) ;
#31140 = CARTESIAN_POINT ( 'NONE',  ( -48.02249751411514467, -183.6283474603465606, 0.8896570909947569827 ) ) ;
#31141 = CARTESIAN_POINT ( 'NONE',  ( -330.4913330509368166, -96.06030588028485795, -53.35787839313392311 ) ) ;
#31142 = ADVANCED_FACE ( 'NONE', ( #34264 ), #11107, .T. ) ;
#31143 = EDGE_CURVE ( 'NONE', #29348, #18800, #49534, .T. ) ;
#31144 = PLANE ( 'NONE',  #20269 ) ;
#31145 = ORIENTED_EDGE ( 'NONE', *, *, #25536, .F. ) ;
#31146 = PLANE ( 'NONE',  #30232 ) ;
#31148 = ORIENTED_EDGE ( 'NONE', *, *, #1154, .F. ) ;
#31147 = DIRECTION ( 'NONE',  ( -0.000000000000000000, 1.000000000000000000, -0.000000000000000000 ) ) ;
#31149 = AXIS2_PLACEMENT_3D ( 'NONE', #33920, #30498, #18429 ) ;
#31150 = VERTEX_POINT ( 'NONE', #10863 ) ;
#31151 = DIRECTION ( 'NONE',  ( -0.000000000000000000, 1.000000000000000000, -0.000000000000000000 ) ) ;
#31152 = ORIENTED_EDGE ( 'NONE', *, *, #18548, .T. ) ;
#31153 = CIRCLE ( 'NONE', #8490, 10.00000000000000178 ) ;
#31154 = LINE ( 'NONE', #47205, #3308 ) ;
#31155 = EDGE_LOOP ( 'NONE', ( #25877, #20257, #7544, #43705 ) ) ;
#31156 = CIRCLE ( 'NONE', #846, 125.0000000000000000 ) ;
#31157 = FACE_BOUND ( 'NONE', #46177, .T. ) ;
#31158 = CARTESIAN_POINT ( 'NONE',  ( -48.47912675150885065, -189.7472609257535510, 6.938893903907228378E-15 ) ) ;
#31159 = ORIENTED_EDGE ( 'NONE', *, *, #16714, .T. ) ;
#31160 = LINE ( 'NONE', #6225, #26619 ) ;
#31161 = EDGE_CURVE ( 'NONE', #38778, #18675, #42665, .T. ) ;
#31162 = EDGE_CURVE ( 'NONE', #47705, #30169, #46617, .T. ) ;
#31163 = DIRECTION ( 'NONE',  ( -0.000000000000000000, 1.000000000000000000, -0.000000000000000000 ) ) ;
#31164 = DIRECTION ( 'NONE',  ( 0.000000000000000000, 0.000000000000000000, -1.000000000000000000 ) ) ;
#31165 = ORIENTED_EDGE ( 'NONE', *, *, #36257, .T. ) ;
#31166 = ORIENTED_EDGE ( 'NONE', *, *, #3467, .F. ) ;
#31167 = EDGE_CURVE ( 'NONE', #50146, #4273, #48692, .T. ) ;
#31168 = ORIENTED_EDGE ( 'NONE', *, *, #32365, .F. ) ;
#31169 = ADVANCED_FACE ( 'NONE', ( #10092 ), #22444, .T. ) ;
#31170 = CYLINDRICAL_SURFACE ( 'NONE', #27591, 4.999999999999997335 ) ;
#31171 = FACE_OUTER_BOUND ( 'NONE', #12423, .T. ) ;
#31172 = AXIS2_PLACEMENT_3D ( 'NONE', #29481, #12930, #17155 ) ;
#31173 = FACE_OUTER_BOUND ( 'NONE', #18553, .T. ) ;
#31174 = CARTESIAN_POINT ( 'NONE',  ( -167.6453766917639427, -193.5000000000000000, 37.74128873232411507 ) ) ;
#31175 = DIRECTION ( 'NONE',  ( 0.000000000000000000, 0.000000000000000000, -1.000000000000000000 ) ) ;
#31176 = ORIENTED_EDGE ( 'NONE', *, *, #9075, .T. ) ;
#31177 = CARTESIAN_POINT ( 'NONE',  ( 9.336583202542589888, -175.3837268820161057, 110.8257356506556306 ) ) ;
#31178 = VERTEX_POINT ( 'NONE', #2200 ) ;
#31180 = ORIENTED_EDGE ( 'NONE', *, *, #25675, .T. ) ;
#31179 = DIRECTION ( 'NONE',  ( 0.000000000000000000, -1.000000000000000000, -0.000000000000000000 ) ) ;
#31181 = CARTESIAN_POINT ( 'NONE',  ( -336.3521761649654422, -98.41210887299327226, -53.46519113769058151 ) ) ;
#31182 = ORIENTED_EDGE ( 'NONE', *, *, #29590, .F. ) ;
#31183 = DIRECTION ( 'NONE',  ( 0.000000000000000000, -1.000000000000000000, 0.000000000000000000 ) ) ;
#31184 = PRODUCT_RELATED_PRODUCT_CATEGORY ( 'part', '', ( #12961 ) ) ;
#31185 = FACE_OUTER_BOUND ( 'NONE', #8659, .T. ) ;
#31186 = CIRCLE ( 'NONE', #26120, 125.0000000000000000 ) ;
#31187 = LINE ( 'NONE', #47238, #17940 ) ;
#31188 = CARTESIAN_POINT ( 'NONE',  ( 57.66105628977221897, -189.7472609257535510, 66.02470404298190942 ) ) ;
#31189 = EDGE_LOOP ( 'NONE', ( #45, #17483, #5853, #36376 ) ) ;
#31190 = CARTESIAN_POINT ( 'NONE',  ( -332.3517673607765914, -126.1322888500942270, -59.00000000000001421 ) ) ;
#31191 = AXIS2_PLACEMENT_3D ( 'NONE', #14344, #30355, #21962 ) ;
#31192 = VERTEX_POINT ( 'NONE', #26637 ) ;
#31193 = EDGE_CURVE ( 'NONE', #16796, #28863, #32737, .T. ) ;
#31194 = VECTOR ( 'NONE', #39988, 1000.000000000000000 ) ;
#31195 = VERTEX_POINT ( 'NONE', #39235 ) ;
#31196 = CARTESIAN_POINT ( 'NONE',  ( -48.30223647638627682, -175.3837268820161057, -0.9842305779475897243 ) ) ;
#31197 = DIRECTION ( 'NONE',  ( -0.9960498426152171181, 0.000000000000000000, 0.08879589532293157006 ) ) ;
#31198 = ORIENTED_EDGE ( 'NONE', *, *, #28258, .T. ) ;
#31199 = LINE ( 'NONE', #39342, #50071 ) ;
#31200 = DIRECTION ( 'NONE',  ( 0.000000000000000000, 1.000000000000000000, 0.000000000000000000 ) ) ;
#31201 = LINE ( 'NONE', #10722, #49022 ) ;
#31202 = CARTESIAN_POINT ( 'NONE',  ( -49.17567778057184569, -193.5000000000000000, -0.7175072570443327136 ) ) ;
#31203 = VERTEX_POINT ( 'NONE', #46885 ) ;
#31204 = FACE_OUTER_BOUND ( 'NONE', #12578, .T. ) ;
#31205 = CARTESIAN_POINT ( 'NONE',  ( -156.7610986364826999, -177.1207230881787780, -62.45009659481510766 ) ) ;
#31206 = AXIS2_PLACEMENT_3D ( 'NONE', #2713, #47128, #18751 ) ;
#31207 = FACE_OUTER_BOUND ( 'NONE', #30350, .T. ) ;
#31208 = EDGE_LOOP ( 'NONE', ( #29093, #9543, #39870, #5948 ) ) ;
#31209 = AXIS2_PLACEMENT_3D ( 'NONE', #14251, #46316, #47083 ) ;
#31210 = DIRECTION ( 'NONE',  ( 1.000000000000000000, -0.000000000000000000, -0.000000000000000000 ) ) ;
#31211 = DIRECTION ( 'NONE',  ( -0.9646355819083614058, 0.000000000000000000, 0.2635871660690581320 ) ) ;
#31212 = ORIENTED_EDGE ( 'NONE', *, *, #5692, .F. ) ;
#31213 = CARTESIAN_POINT ( 'NONE',  ( -336.3521761649654422, -146.8829211657874794, -54.23253582808848705 ) ) ;
#31214 = VERTEX_POINT ( 'NONE', #38961 ) ;
#31215 = CARTESIAN_POINT ( 'NONE',  ( -336.3521761649654422, -72.01665693856799066, -28.86398714850468039 ) ) ;
#31216 = FACE_BOUND ( 'NONE', #48644, .T. ) ;
#31218 = ORIENTED_EDGE ( 'NONE', *, *, #41475, .T. ) ;
#31217 = DIRECTION ( 'NONE',  ( 0.000000000000000000, 1.000000000000000000, 0.000000000000000000 ) ) ;
#31219 = VECTOR ( 'NONE', #48132, 1000.000000000000114 ) ;
#31220 = EDGE_CURVE ( 'NONE', #38204, #16314, #3246, .T. ) ;
#31221 = VECTOR ( 'NONE', #41878, 1000.000000000000114 ) ;
#31222 = CARTESIAN_POINT ( 'NONE',  ( 43.57032560458359427, -189.7472609257535510, 83.08371579725745448 ) ) ;
#31223 = EDGE_LOOP ( 'NONE', ( #20825, #48173, #41755, #29661 ) ) ;
#31224 = VECTOR ( 'NONE', #30696, 1000.000000000000000 ) ;
#31225 = EDGE_LOOP ( 'NONE', ( #8549, #16009, #34107, #4698 ) ) ;
#31226 = PLANE ( 'NONE',  #36789 ) ;
#31227 = ORIENTED_EDGE ( 'NONE', *, *, #12652, .F. ) ;
#31228 = CARTESIAN_POINT ( 'NONE',  ( -167.1580984288390823, -193.5000000000000000, -39.24667733211878584 ) ) ;
#31229 = AXIS2_PLACEMENT_3D ( 'NONE', #41555, #49722, #13456 ) ;
#31230 = VECTOR ( 'NONE', #27235, 1000.000000000000000 ) ;
#31231 = PLANE ( 'NONE',  #43529 ) ;
#31232 = FACE_OUTER_BOUND ( 'NONE', #10002, .T. ) ;
#31233 = ORIENTED_EDGE ( 'NONE', *, *, #32087, .T. ) ;
#31236 = ORIENTED_EDGE ( 'NONE', *, *, #25234, .T. ) ;
#31235 = CARTESIAN_POINT ( 'NONE',  ( 26.10278175629141018, -175.3837268820161057, -99.06333546307678262 ) ) ;
#31234 = DIRECTION ( 'NONE',  ( 0.000000000000000000, -0.000000000000000000, -1.000000000000000000 ) ) ;
#31237 = VECTOR ( 'NONE', #21345, 1000.000000000000000 ) ;
#31238 = AXIS2_PLACEMENT_3D ( 'NONE', #17228, #38217, #37967 ) ;
#31239 = EDGE_CURVE ( 'NONE', #9613, #47963, #35038, .T. ) ;
#31240 = DIRECTION ( 'NONE',  ( -0.000000000000000000, 1.000000000000000000, -0.000000000000000000 ) ) ;
#31241 = ORIENTED_EDGE ( 'NONE', *, *, #46521, .F. ) ;
#31242 = DIRECTION ( 'NONE',  ( -0.7948544414133608127, 0.000000000000000000, 0.6068001458185834363 ) ) ;
#31243 = EDGE_LOOP ( 'NONE', ( #31507, #29696, #29414, #27043 ) ) ;
#31244 = CARTESIAN_POINT ( 'NONE',  ( -47.47956591500005885, -193.5000000000000000, -0.02963332782254939762 ) ) ;
#31245 = ORIENTED_EDGE ( 'NONE', *, *, #35913, .F. ) ;
#31247 = CARTESIAN_POINT ( 'NONE',  ( -336.3521761649654422, -179.5993808087905279, -18.46045550523168899 ) ) ;
#31246 = LINE ( 'NONE', #27302, #19873 ) ;
#31248 = EDGE_LOOP ( 'NONE', ( #12147, #47935, #51287, #49643 ) ) ;
#31249 = DIRECTION ( 'NONE',  ( 0.000000000000000000, 0.000000000000000000, -1.000000000000000000 ) ) ;
#31250 = VERTEX_POINT ( 'NONE', #47127 ) ;
#31251 = DIRECTION ( 'NONE',  ( 0.000000000000000000, 0.1205366802553164696, -0.9927088740980548609 ) ) ;
#31252 = DIRECTION ( 'NONE',  ( -0.5586467658036476935, 0.000000000000000000, -0.8294056854502049880 ) ) ;
#31253 = ORIENTED_EDGE ( 'NONE', *, *, #16775, .F. ) ;
#31254 = FACE_OUTER_BOUND ( 'NONE', #45708, .T. ) ;
#31255 = DIRECTION ( 'NONE',  ( 0.000000000000000000, 1.000000000000000000, -0.000000000000000000 ) ) ;
#31256 = CARTESIAN_POINT ( 'NONE',  ( -62.43888699632653072, -175.3837268820161057, 124.2180546213279229 ) ) ;
#31257 = AXIS2_PLACEMENT_3D ( 'NONE', #5494, #24936, #37015 ) ;
#31258 = DIRECTION ( 'NONE',  ( -1.000000000000000000, 0.000000000000000000, 0.000000000000000000 ) ) ;
#31259 = ORIENTED_EDGE ( 'NONE', *, *, #14446, .T. ) ;
#31260 = EDGE_CURVE ( 'NONE', #47114, #5997, #40656, .T. ) ;
#31261 = CARTESIAN_POINT ( 'NONE',  ( -89.44307666693796932, -193.5000000000000000, -117.0391155081702266 ) ) ;
#31262 = CARTESIAN_POINT ( 'NONE',  ( -2.174401709722246334, -193.5000000000000000, -115.0304316645280096 ) ) ;
#31263 = VECTOR ( 'NONE', #45459, 1000.000000000000000 ) ;
#31264 = CARTESIAN_POINT ( 'NONE',  ( 66.42899531795131907, -183.6283474603465606, 49.20491319441622124 ) ) ;
#31265 = ORIENTED_EDGE ( 'NONE', *, *, #29730, .F. ) ;
#31266 = EDGE_CURVE ( 'NONE', #34274, #15102, #6159, .T. ) ;
#31267 = DIRECTION ( 'NONE',  ( 0.000000000000000000, -1.000000000000000000, -0.000000000000000000 ) ) ;
#31268 = DIRECTION ( 'NONE',  ( 0.000000000000000000, 6.938893903907229364E-16, 1.000000000000000000 ) ) ;
#31269 = FACE_OUTER_BOUND ( 'NONE', #37496, .T. ) ;
#31271 = ORIENTED_EDGE ( 'NONE', *, *, #3441, .T. ) ;
#31270 = LINE ( 'NONE', #22365, #29111 ) ;
#31272 = VERTEX_POINT ( 'NONE', #35802 ) ;
#31273 = VECTOR ( 'NONE', #27272, 1000.000000000000000 ) ;
#31274 = EDGE_CURVE ( 'NONE', #18899, #43264, #28162, .T. ) ;
#31275 = CIRCLE ( 'NONE', #8620, 125.0000000000000000 ) ;
#31276 = CYLINDRICAL_SURFACE ( 'NONE', #26250, 4.999999999999997335 ) ;
#31277 = AXIS2_PLACEMENT_3D ( 'NONE', #33981, #13504, #29519 ) ;
#31278 = DIRECTION ( 'NONE',  ( 0.5085311186492154079, 0.000000000000000000, 0.8610436117673585521 ) ) ;
#31279 = CARTESIAN_POINT ( 'NONE',  ( -48.47912675150885065, -177.1207230881787780, 1.000000000000006883 ) ) ;
#31280 = DIRECTION ( 'NONE',  ( -0.9960498426152177842, 0.000000000000000000, 0.08879589532292482545 ) ) ;
#31281 = DIRECTION ( 'NONE',  ( 1.000000000000000000, -0.000000000000000000, -0.000000000000000000 ) ) ;
#31282 = ORIENTED_EDGE ( 'NONE', *, *, #44871, .T. ) ;
#31283 = EDGE_CURVE ( 'NONE', #232, #49593, #20549, .T. ) ;
#31284 = AXIS2_PLACEMENT_3D ( 'NONE', #25733, #30196, #9705 ) ;
#31285 = CARTESIAN_POINT ( 'NONE',  ( 1.445069716139520066, 57.92390192091106371, -16.54020211540079899 ) ) ;
#31286 = EDGE_CURVE ( 'NONE', #29888, #32182, #7693, .T. ) ;
#31287 = ORIENTED_EDGE ( 'NONE', *, *, #35692, .F. ) ;
#31288 = EDGE_LOOP ( 'NONE', ( #6516, #28670, #40876, #41439 ) ) ;
#31289 = ADVANCED_FACE ( 'NONE', ( #48422 ), #20037, .T. ) ;
#31290 = VERTEX_POINT ( 'NONE', #35531 ) ;
#31291 = CARTESIAN_POINT ( 'NONE',  ( 34.23904069044534992, -183.6283474603465606, -92.37913469314065651 ) ) ;
#31292 = AXIS2_PLACEMENT_3D ( 'NONE', #45635, #16475, #700 ) ;
#31293 = CYLINDRICAL_SURFACE ( 'NONE', #50477, 125.0000000000000000 ) ;
#31294 = ORIENTED_EDGE ( 'NONE', *, *, #1355, .T. ) ;
#31295 = AXIS2_PLACEMENT_3D ( 'NONE', #35043, #38967, #34272 ) ;
#31296 = PLANE ( 'NONE',  #29232 ) ;
#31297 = CARTESIAN_POINT ( 'NONE',  ( -339.1964088526558498, -65.12585595286510909, 13.87297036558291197 ) ) ;
#31300 = ORIENTED_EDGE ( 'NONE', *, *, #44958, .T. ) ;
#31299 = LINE ( 'NONE', #22910, #40904 ) ;
#31298 = CARTESIAN_POINT ( 'NONE',  ( -330.4913330509368166, -95.63860483659048839, 52.00954392751722111 ) ) ;
#31301 = EDGE_CURVE ( 'NONE', #43088, #30974, #15585, .T. ) ;
#31302 = CARTESIAN_POINT ( 'NONE',  ( -336.3521761649653854, -64.15626348514393840, -8.849911663702499709 ) ) ;
#31303 = ORIENTED_EDGE ( 'NONE', *, *, #42980, .T. ) ;
#31304 = DIRECTION ( 'NONE',  ( 0.000000000000000000, 0.000000000000000000, 1.000000000000000000 ) ) ;
#31305 = ORIENTED_EDGE ( 'NONE', *, *, #21026, .F. ) ;
#31306 = DIRECTION ( 'NONE',  ( 0.000000000000000000, 0.000000000000000000, 1.000000000000000000 ) ) ;
#31307 = FACE_OUTER_BOUND ( 'NONE', #49075, .T. ) ;
#31309 = DIRECTION ( 'NONE',  ( 0.000000000000000000, 0.000000000000000000, 1.000000000000000000 ) ) ;
#31308 = CARTESIAN_POINT ( 'NONE',  ( 55.03325008324585355, -183.6283474603465606, -70.07273251429357686 ) ) ;
#31310 = CIRCLE ( 'NONE', #38021, 125.0000000000000000 ) ;
#31311 = AXIS2_PLACEMENT_3D ( 'NONE', #6222, #39308, #34334 ) ;
#31312 = ORIENTED_EDGE ( 'NONE', *, *, #5264, .T. ) ;
#31313 = DIRECTION ( 'NONE',  ( 0.000000000000000000, 0.4647231720437664526, -0.8854560256532110207 ) ) ;
#31314 = ORIENTED_EDGE ( 'NONE', *, *, #2798, .T. ) ;
#31315 = AXIS2_PLACEMENT_3D ( 'NONE', #31080, #3734, #23213 ) ;
#31316 = LINE ( 'NONE', #2442, #48295 ) ;
#31317 = VERTEX_POINT ( 'NONE', #7448 ) ;
#31318 = FACE_OUTER_BOUND ( 'NONE', #7539, .T. ) ;
#31319 = LINE ( 'NONE', #47363, #44160 ) ;
#31320 = ORIENTED_EDGE ( 'NONE', *, *, #19211, .T. ) ;
#31321 = FACE_BOUND ( 'NONE', #22139, .T. ) ;
#31322 = VECTOR ( 'NONE', #13575, 1000.000000000000000 ) ;
#31323 = PLANE ( 'NONE',  #43253 ) ;
#31324 = EDGE_CURVE ( 'NONE', #18133, #43502, #31865, .T. ) ;
#31325 = ORIENTED_EDGE ( 'NONE', *, *, #28433, .T. ) ;
#31326 = PLANE ( 'NONE',  #45925 ) ;
#31327 = VERTEX_POINT ( 'NONE', #23716 ) ;
#31328 = DIRECTION ( 'NONE',  ( 0.000000000000000000, 0.000000000000000000, -1.000000000000000000 ) ) ;
#31329 = LINE ( 'NONE', #43682, #17742 ) ;
#31330 = VERTEX_POINT ( 'NONE', #43694 ) ;
#31331 = DIRECTION ( 'NONE',  ( 0.000000000000000000, 0.000000000000000000, 1.000000000000000000 ) ) ;
#31332 = EDGE_CURVE ( 'NONE', #3078, #48105, #39831, .T. ) ;
#31333 = LINE ( 'NONE', #23964, #29795 ) ;
#31334 = CARTESIAN_POINT ( 'NONE',  ( -330.4913330509368166, -123.5000000000000284, 0.000000000000000000 ) ) ;
#31335 = EDGE_CURVE ( 'NONE', #18623, #52027, #51859, .T. ) ;
#31336 = AXIS2_PLACEMENT_3D ( 'NONE', #26827, #42861, #34974 ) ;
#31337 = CARTESIAN_POINT ( 'NONE',  ( 1.734723475976807094E-15, 0.000000000000000000, 41.00000000000000711 ) ) ;
#31338 = CARTESIAN_POINT ( 'NONE',  ( 76.43863189440992301, -175.3837268820161057, -4.533605064403317009 ) ) ;
#31339 = CARTESIAN_POINT ( 'NONE',  ( -106.4764934152196645, -213.5000000000000000, -110.7307791902283043 ) ) ;
#31341 = VERTEX_POINT ( 'NONE', #3736 ) ;
#31340 = DIRECTION ( 'NONE',  ( 1.000000000000000000, -0.000000000000000000, -0.000000000000000000 ) ) ;
#31342 = ORIENTED_EDGE ( 'NONE', *, *, #49795, .T. ) ;
#31343 = DIRECTION ( 'NONE',  ( 0.000000000000000000, 0.9350162426854194964, 0.3546048870425235200 ) ) ;
#31344 = EDGE_CURVE ( 'NONE', #38174, #12681, #61, .T. ) ;
#31345 = VECTOR ( 'NONE', #2166, 1000.000000000000000 ) ;
#31346 = EDGE_CURVE ( 'NONE', #15571, #11734, #43446, .T. ) ;
#31347 = DIRECTION ( 'NONE',  ( 0.05924062789370748011, 0.000000000000000000, 0.9982437317643217956 ) ) ;
#31348 = ORIENTED_EDGE ( 'NONE', *, *, #39458, .T. ) ;
#31349 =( REPRESENTATION_RELATIONSHIP ('NONE','NONE', #4578, #24080 ) REPRESENTATION_RELATIONSHIP_WITH_TRANSFORMATION ( #29912 )SHAPE_REPRESENTATION_RELATIONSHIP( ) );
#31350 = VECTOR ( 'NONE', #31442, 999.9999999999998863 ) ;
#31351 = EDGE_LOOP ( 'NONE', ( #16574, #38264, #30814, #37207 ) ) ;
#31352 = ADVANCED_FACE ( 'NONE', ( #3483 ), #27912, .F. ) ;
#31353 = CARTESIAN_POINT ( 'NONE',  ( -154.0877180371535928, -193.5000000000000000, -66.87170886601927577 ) ) ;
#31354 = VERTEX_POINT ( 'NONE', #36062 ) ;
#31355 = CARTESIAN_POINT ( 'NONE',  ( -48.77118352214581876, -189.7472609257535510, -0.9564009842765195391 ) ) ;
#31356 = DIRECTION ( 'NONE',  ( 0.000000000000000000, -1.000000000000000000, -0.000000000000000000 ) ) ;
#31357 = EDGE_CURVE ( 'NONE', #48695, #37838, #16103, .T. ) ;
#31358 = CARTESIAN_POINT ( 'NONE',  ( -330.4913330509368166, -138.3439121830091665, 58.13482838284733845 ) ) ;
#31359 = DIRECTION ( 'NONE',  ( 1.043714542225393697E-14, 0.7485107481710934207, -0.6631226582408039638 ) ) ;
#31360 = ORIENTED_EDGE ( 'NONE', *, *, #38759, .F. ) ;
#31361 = ORIENTED_EDGE ( 'NONE', *, *, #21349, .T. ) ;
#31362 = ORIENTED_EDGE ( 'NONE', *, *, #29520, .T. ) ;
#31363 = DIRECTION ( 'NONE',  ( 5.399917434947259359E-17, 1.000000000000000000, -0.000000000000000000 ) ) ;
#31364 = CARTESIAN_POINT ( 'NONE',  ( -48.30223647638627682, -177.1207230881787780, -0.9842305779475897243 ) ) ;
#31365 = CARTESIAN_POINT ( 'NONE',  ( -15.81236726369125023, -193.5000000000000000, -120.6560517527615417 ) ) ;
#31366 = DIRECTION ( 'NONE',  ( -0.9890401873221633666, 0.000000000000000000, -0.1476465640024850756 ) ) ;
#31367 = DIRECTION ( 'NONE',  ( 0.000000000000000000, -0.000000000000000000, 1.000000000000000000 ) ) ;
#31368 = AXIS2_PLACEMENT_3D ( 'NONE', #38580, #30680, #46735 ) ;
#31369 = EDGE_LOOP ( 'NONE', ( #42987, #36111, #50934, #22851 ) ) ;
#31370 = DIRECTION ( 'NONE',  ( -1.000000000000000000, -0.000000000000000000, -0.000000000000000000 ) ) ;
#31371 = FACE_OUTER_BOUND ( 'NONE', #17689, .T. ) ;
#31372 = CIRCLE ( 'NONE', #24665, 125.0000000000000000 ) ;
#31373 = EDGE_LOOP ( 'NONE', ( #7877, #2014, #44553, #27406 ) ) ;
#31374 = ORIENTED_EDGE ( 'NONE', *, *, #34957, .T. ) ;
#31375 = LINE ( 'NONE', #27437, #34807 ) ;
#31376 = DIRECTION ( 'NONE',  ( 1.000000000000000000, 0.000000000000000000, -0.000000000000000000 ) ) ;
#31377 = ORIENTED_EDGE ( 'NONE', *, *, #20009, .T. ) ;
#31378 = CARTESIAN_POINT ( 'NONE',  ( -47.47956591500005885, -175.3837268820161057, -0.02963332782254939762 ) ) ;
#31379 = DIRECTION ( 'NONE',  ( 0.000000000000000000, 0.000000000000000000, 1.000000000000000000 ) ) ;
#31380 = LINE ( 'NONE', #22733, #17606 ) ;
#31381 = ORIENTED_EDGE ( 'NONE', *, *, #12364, .T. ) ;
#31382 = LINE ( 'NONE', #3015, #50255 ) ;
#31383 = AXIS2_PLACEMENT_3D ( 'NONE', #22904, #27795, #40391 ) ;
#31384 = VERTEX_POINT ( 'NONE', #44211 ) ;
#31385 = CARTESIAN_POINT ( 'NONE',  ( -170.0000000000000284, -113.5000000000000142, 39.99999999999998579 ) ) ;
#31386 = EDGE_CURVE ( 'NONE', #43619, #40951, #8211, .T. ) ;
#31387 = DIRECTION ( 'NONE',  ( 0.000000000000000000, -1.000000000000000000, -0.000000000000000000 ) ) ;
#31388 = ORIENTED_EDGE ( 'NONE', *, *, #25390, .F. ) ;
#31389 = EDGE_CURVE ( 'NONE', #47761, #9672, #4267, .T. ) ;
#31390 = CARTESIAN_POINT ( 'NONE',  ( -125.5794209599708466, -193.5000000000000000, 97.11716833071892552 ) ) ;
#31391 = EDGE_CURVE ( 'NONE', #45944, #28183, #315, .T. ) ;
#31392 = DIRECTION ( 'NONE',  ( 0.4300652022765245608, 0.000000000000000000, -0.9027978299657416494 ) ) ;
#31393 = CARTESIAN_POINT ( 'NONE',  ( -143.3583119192899744, -177.1207230881787780, -81.38144888055202841 ) ) ;
#31394 = EDGE_CURVE ( 'NONE', #8493, #13356, #24490, .T. ) ;
#31395 = LINE ( 'NONE', #11421, #41685 ) ;
#31396 = EDGE_CURVE ( 'NONE', #8311, #5668, #36579, .T. ) ;
#31397 = DIRECTION ( 'NONE',  ( 1.000000000000000000, -0.000000000000000000, 0.000000000000000000 ) ) ;
#31398 = ORIENTED_EDGE ( 'NONE', *, *, #20419, .T. ) ;
#31399 = ORIENTED_EDGE ( 'NONE', *, *, #39678, .T. ) ;
#31400 = ADVANCED_FACE ( 'NONE', ( #16551 ), #15505, .F. ) ;
#31401 = PLANE ( 'NONE',  #44931 ) ;
#31403 = VERTEX_POINT ( 'NONE', #35454 ) ;
#31402 = DIRECTION ( 'NONE',  ( -1.000000000000000000, -0.000000000000000000, -0.000000000000000000 ) ) ;
#31404 = VECTOR ( 'NONE', #33954, 999.9999999999998863 ) ;
#31405 = AXIS2_PLACEMENT_3D ( 'NONE', #35714, #19684, #11795 ) ;
#31406 = EDGE_LOOP ( 'NONE', ( #5389, #6906, #45375, #31830 ) ) ;
#31407 = LINE ( 'NONE', #124, #50084 ) ;
#31408 = EDGE_CURVE ( 'NONE', #41381, #38006, #30607, .T. ) ;
#31409 = VECTOR ( 'NONE', #22223, 1000.000000000000114 ) ;
#31410 = ADVANCED_FACE ( 'NONE', ( #3404 ), #19434, .F. ) ;
#31411 = CARTESIAN_POINT ( 'NONE',  ( -170.2837019307126809, -193.5000000000000000, 23.23456943914129269 ) ) ;
#31412 = ORIENTED_EDGE ( 'NONE', *, *, #4295, .T. ) ;
#31413 = ADVANCED_FACE ( 'NONE', ( #39648 ), #51505, .T. ) ;
#31414 = CARTESIAN_POINT ( 'NONE',  ( -98.62206515315352817, -193.5000000000000000, 113.4093733337831367 ) ) ;
#31415 = DIRECTION ( 'NONE',  ( 0.000000000000000000, -1.000000000000000000, 0.000000000000000000 ) ) ;
#31416 = ORIENTED_EDGE ( 'NONE', *, *, #2216, .F. ) ;
#31417 = CARTESIAN_POINT ( 'NONE',  ( 26.52087324849106054, -198.5000000000000000, -70.00000000000002842 ) ) ;
#31418 = ADVANCED_FACE ( 'NONE', ( #11798 ), #27824, .F. ) ;
#31420 = AXIS2_PLACEMENT_3D ( 'NONE', #9600, #21693, #29307 ) ;
#31419 = LINE ( 'NONE', #30912, #44567 ) ;
#31421 = CARTESIAN_POINT ( 'NONE',  ( -172.2424017797220870, -177.1207230881787780, 7.666780576875857456 ) ) ;
#31422 = ORIENTED_EDGE ( 'NONE', *, *, #3543, .F. ) ;
#31423 = ORIENTED_EDGE ( 'NONE', *, *, #41660, .T. ) ;
#31424 = ADVANCED_FACE ( 'NONE', ( #40183 ), #23391, .T. ) ;
#31425 = ORIENTED_EDGE ( 'NONE', *, *, #31741, .T. ) ;
#31426 = CARTESIAN_POINT ( 'NONE',  ( -66.46933728415690723, -193.5000000000000000, 122.6885491605231522 ) ) ;
#31427 = CARTESIAN_POINT ( 'NONE',  ( -28.86423599357335590, -183.6283474603465606, 122.4396006697296144 ) ) ;
#31428 = CARTESIAN_POINT ( 'NONE',  ( 13.41824523304568828, 28.00000000000000355, 8.421342806086375532 ) ) ;
#31429 = CARTESIAN_POINT ( 'NONE',  ( -169.8550585387150136, -175.3837268820161057, 25.37485791684381553 ) ) ;
#31430 = DIRECTION ( 'NONE',  ( 0.000000000000000000, 0.000000000000000000, -1.000000000000000000 ) ) ;
#31431 = VERTEX_POINT ( 'NONE', #7369 ) ;
#31432 = EDGE_CURVE ( 'NONE', #19489, #7086, #27583, .T. ) ;
#31433 = CARTESIAN_POINT ( 'NONE',  ( -171.2727421180348415, -177.1207230881787780, 23.38221600314377113 ) ) ;
#31434 = ORIENTED_EDGE ( 'NONE', *, *, #27835, .F. ) ;
#31436 = ORIENTED_EDGE ( 'NONE', *, *, #5138, .F. ) ;
#31435 = CARTESIAN_POINT ( 'NONE',  ( -49.47517659412406488, -193.5000000000000000, -0.08879589532293878651 ) ) ;
#31437 = ORIENTED_EDGE ( 'NONE', *, *, #46239, .F. ) ;
#31438 = LINE ( 'NONE', #34602, #3986 ) ;
#31439 = CYLINDRICAL_SURFACE ( 'NONE', #7348, 125.0000000000000000 ) ;
#31440 = VECTOR ( 'NONE', #5546, 1000.000000000000114 ) ;
#31441 = VECTOR ( 'NONE', #37793, 1000.000000000000000 ) ;
#31442 = DIRECTION ( 'NONE',  ( 0.2920567706369764371, 0.000000000000000000, -0.9564009842765223146 ) ) ;
#31443 = CARTESIAN_POINT ( 'NONE',  ( -339.1964088526558498, -102.1108035431470427, 54.98865587491797413 ) ) ;
#31444 = ORIENTED_EDGE ( 'NONE', *, *, #22546, .F. ) ;
#31445 = PLANE ( 'NONE',  #46839 ) ;
#31446 = ORIENTED_EDGE ( 'NONE', *, *, #47213, .F. ) ;
#31447 = VECTOR ( 'NONE', #11356, 1000.000000000000000 ) ;
#31448 = ADVANCED_FACE ( 'NONE', ( #4449 ), #4195, .F. ) ;
#31449 = ORIENTED_EDGE ( 'NONE', *, *, #39521, .T. ) ;
#31450 = CARTESIAN_POINT ( 'NONE',  ( -104.3615810019516630, -175.3837268820161057, 110.6939782313525455 ) ) ;
#31451 = CARTESIAN_POINT ( 'NONE',  ( -47.64924157374594671, -175.3837268820161057, 124.9972451320097377 ) ) ;
#31452 = CIRCLE ( 'NONE', #51607, 124.9999999999999858 ) ;
#31453 = DIRECTION ( 'NONE',  ( 0.000000000000000000, -0.8854560256532141294, -0.4647231720437604574 ) ) ;
#31454 = DIRECTION ( 'NONE',  ( 0.000000000000000000, -0.000000000000000000, 1.000000000000000000 ) ) ;
#31455 = EDGE_CURVE ( 'NONE', #28202, #2676, #48073, .T. ) ;
#31456 = ADVANCED_FACE ( 'NONE', ( #3661 ), #486, .T. ) ;
#31457 = LINE ( 'NONE', #22809, #30548 ) ;
#31458 = DIRECTION ( 'NONE',  ( 0.000000000000000000, 1.000000000000000000, 0.000000000000000000 ) ) ;
#31459 = ORIENTED_EDGE ( 'NONE', *, *, #22043, .F. ) ;
#31460 = AXIS2_PLACEMENT_3D ( 'NONE', #34475, #50521, #26590 ) ;
#31461 = CARTESIAN_POINT ( 'NONE',  ( 70.02079272397770637, -193.5000000000000000, -36.52255268223056106 ) ) ;
#31462 = DIRECTION ( 'NONE',  ( -0.000000000000000000, 1.000000000000000000, -0.000000000000000000 ) ) ;
#31463 = EDGE_CURVE ( 'NONE', #11866, #34416, #15783, .T. ) ;
#31464 = FACE_BOUND ( 'NONE', #37272, .T. ) ;
#31465 = EDGE_LOOP ( 'NONE', ( #22036, #9031, #34806, #32717 ) ) ;
#31466 = DIRECTION ( 'NONE',  ( 5.399917434947259359E-17, 1.000000000000000000, -0.000000000000000000 ) ) ;
#31467 = ORIENTED_EDGE ( 'NONE', *, *, #11762, .T. ) ;
#31468 = DIRECTION ( 'NONE',  ( 0.000000000000000000, -0.3546048870425396182, -0.9350162426854132791 ) ) ;
#31469 = VERTEX_POINT ( 'NONE', #47828 ) ;
#31470 = FACE_OUTER_BOUND ( 'NONE', #17492, .T. ) ;
#31471 = CIRCLE ( 'NONE', #49951, 4.999999999999997335 ) ;
#31472 = ADVANCED_FACE ( 'NONE', ( #39906 ), #42703, .T. ) ;
#31473 = FACE_BOUND ( 'NONE', #29825, .T. ) ;
#31475 = VERTEX_POINT ( 'NONE', #32286 ) ;
#31474 = DIRECTION ( 'NONE',  ( -0.000000000000000000, 0.1205366802553199113, -0.9927088740980544168 ) ) ;
#31476 = AXIS2_PLACEMENT_3D ( 'NONE', #3386, #31242, #44110 ) ;
#31477 = VECTOR ( 'NONE', #50669, 1000.000000000000000 ) ;
#31478 = ADVANCED_FACE ( 'NONE', ( #48339 ), #12323, .T. ) ;
#31479 = CARTESIAN_POINT ( 'NONE',  ( 0.000000000000000000, -66.21443277186293130, -14.11962419296594362 ) ) ;
#31480 = ORIENTED_EDGE ( 'NONE', *, *, #9226, .F. ) ;
#31481 = CIRCLE ( 'NONE', #14736, 125.0000000000000000 ) ;
#31482 = EDGE_CURVE ( 'NONE', #4347, #39696, #32562, .T. ) ;
#31483 = ORIENTED_EDGE ( 'NONE', *, *, #51070, .T. ) ;
#31484 = LINE ( 'NONE', #50967, #17489 ) ;
#31485 = VERTEX_POINT ( 'NONE', #9687 ) ;
#31486 = VECTOR ( 'NONE', #9664, 1000.000000000000227 ) ;
#31487 = FACE_OUTER_BOUND ( 'NONE', #36931, .T. ) ;
#31488 = VECTOR ( 'NONE', #33231, 1000.000000000000000 ) ;
#31489 = VECTOR ( 'NONE', #50714, 1000.000000000000000 ) ;
#31490 = VECTOR ( 'NONE', #9725, 1000.000000000000227 ) ;
#31491 = LINE ( 'NONE', #23863, #24244 ) ;
#31492 = CARTESIAN_POINT ( 'NONE',  ( 72.71365293123227502, -193.5000000000000000, -30.61552143554913030 ) ) ;
#31493 = VERTEX_POINT ( 'NONE', #36771 ) ;
#31496 = ORIENTED_EDGE ( 'NONE', *, *, #21208, .F. ) ;
#31495 = FACE_OUTER_BOUND ( 'NONE', #47031, .T. ) ;
#31494 = FACE_OUTER_BOUND ( 'NONE', #17370, .T. ) ;
#31497 = DIRECTION ( 'NONE',  ( 0.000000000000000000, 1.000000000000000000, -0.000000000000000000 ) ) ;
#31498 = ORIENTED_EDGE ( 'NONE', *, *, #24050, .T. ) ;
#31499 = FACE_OUTER_BOUND ( 'NONE', #47657, .T. ) ;
#31500 = ORIENTED_EDGE ( 'NONE', *, *, #21138, .F. ) ;
#31501 = DIRECTION ( 'NONE',  ( 0.000000000000000000, -8.095376221225100300E-15, -1.000000000000000000 ) ) ;
#31502 = ORIENTED_EDGE ( 'NONE', *, *, #18877, .T. ) ;
#31504 = DIRECTION ( 'NONE',  ( -0.4566292373937018145, 0.000000000000000000, -0.8896570909947529859 ) ) ;
#31503 = DIRECTION ( 'NONE',  ( -1.000000000000000000, 0.000000000000000000, 0.000000000000000000 ) ) ;
#31505 = EDGE_LOOP ( 'NONE', ( #2367, #13467, #1957, #49861 ) ) ;
#31506 = LINE ( 'NONE', #30998, #25686 ) ;
#31507 = ORIENTED_EDGE ( 'NONE', *, *, #44512, .F. ) ;
#31508 = PLANE ( 'NONE',  #16985 ) ;
#31509 = VECTOR ( 'NONE', #33664, 1000.000000000000114 ) ;
#31510 = DIRECTION ( 'NONE',  ( -1.000000000000000000, -0.000000000000000000, -0.000000000000000000 ) ) ;
#31511 = CARTESIAN_POINT ( 'NONE',  ( -112.7586829773731267, -193.5000000000000000, -107.2060569716373379 ) ) ;
#31512 = CARTESIAN_POINT ( 'NONE',  ( 60.00000000000001421, 0.000000000000000000, 60.00000000000000711 ) ) ;
#31513 = CARTESIAN_POINT ( 'NONE',  ( 2.669657140899367676, -189.7472609257535510, 114.0561348912355726 ) ) ;
#31514 = VECTOR ( 'NONE', #25258, 1000.000000000000000 ) ;
#31515 = CARTESIAN_POINT ( 'NONE',  ( -48.30223647638628393, -193.5000000000000000, 0.9842305779476049343 ) ) ;
#31516 = AXIS2_PLACEMENT_3D ( 'NONE', #23206, #18738, #42899 ) ;
#31517 = ORIENTED_EDGE ( 'NONE', *, *, #30207, .F. ) ;
#31518 = EDGE_CURVE ( 'NONE', #27166, #47640, #45441, .T. ) ;
#31519 = EDGE_CURVE ( 'NONE', #35003, #18053, #15515, .T. ) ;
#31520 = DIRECTION ( 'NONE',  ( 0.9820818503191364179, 2.775557561562891351E-17, -0.1884548733085492089 ) ) ;
#31521 = FACE_OUTER_BOUND ( 'NONE', #18981, .T. ) ;
#31522 = CYLINDRICAL_SURFACE ( 'NONE', #18956, 124.9999999999999858 ) ;
#31523 = LINE ( 'NONE', #7617, #36333 ) ;
#31524 = ORIENTED_EDGE ( 'NONE', *, *, #3702, .T. ) ;
#31525 = DIRECTION ( 'NONE',  ( 0.000000000000000000, 0.2393156642875548246, -0.9709418174260527890 ) ) ;
#31526 = FACE_OUTER_BOUND ( 'NONE', #30267, .T. ) ;
#31527 = AXIS2_PLACEMENT_3D ( 'NONE', #46407, #34557, #50870 ) ;
#31528 = FACE_OUTER_BOUND ( 'NONE', #33312, .T. ) ;
#31530 = ORIENTED_EDGE ( 'NONE', *, *, #39521, .F. ) ;
#31529 = DIRECTION ( 'NONE',  ( 5.399917434947259359E-17, 1.000000000000000000, -0.000000000000000000 ) ) ;
#31531 = EDGE_LOOP ( 'NONE', ( #43215, #11390, #48189, #11247 ) ) ;
#31532 = AXIS2_PLACEMENT_3D ( 'NONE', #51305, #3455, #28135 ) ;
#31533 = ORIENTED_EDGE ( 'NONE', *, *, #38782, .T. ) ;
#31534 = AXIS2_PLACEMENT_3D ( 'NONE', #16132, #24273, #20315 ) ;
#31535 = LINE ( 'NONE', #19704, #36307 ) ;
#31536 = LINE ( 'NONE', #23413, #39611 ) ;
#31537 = EDGE_CURVE ( 'NONE', #34920, #17366, #18030, .T. ) ;
#31538 = CARTESIAN_POINT ( 'NONE',  ( 71.44208735029286572, -177.1207230881787780, 35.26900067126700833 ) ) ;
#31539 = DIRECTION ( 'NONE',  ( 0.000000000000000000, -0.000000000000000000, -1.000000000000000000 ) ) ;
#31540 = ORIENTED_EDGE ( 'NONE', *, *, #40065, .F. ) ;
#31541 = CARTESIAN_POINT ( 'NONE',  ( -339.1964088526558498, -70.14212160686619768, -27.43969411971537298 ) ) ;
#31542 = EDGE_CURVE ( 'NONE', #21288, #46449, #44914, .T. ) ;
#31543 = ORIENTED_EDGE ( 'NONE', *, *, #49929, .T. ) ;
#31544 = VERTEX_POINT ( 'NONE', #28605 ) ;
#31545 = CIRCLE ( 'NONE', #33204, 124.9999999999999858 ) ;
#31546 = AXIS2_PLACEMENT_3D ( 'NONE', #22283, #10448, #21519 ) ;
#31547 = ORIENTED_EDGE ( 'NONE', *, *, #15071, .T. ) ;
#31548 = CARTESIAN_POINT ( 'NONE',  ( -336.3521761649654422, -66.84438072661991725, -16.67542351306652648 ) ) ;
#31549 = VECTOR ( 'NONE', #4191, 1000.000000000000000 ) ;
#31550 = VECTOR ( 'NONE', #23453, 1000.000000000000000 ) ;
#31551 = FACE_OUTER_BOUND ( 'NONE', #3257, .T. ) ;
#31552 = VERTEX_POINT ( 'NONE', #8645 ) ;
#31553 = PLANE ( 'NONE',  #34262 ) ;
#31554 = DIRECTION ( 'NONE',  ( -0.000000000000000000, 1.000000000000000000, -0.000000000000000000 ) ) ;
#31557 = ORIENTED_EDGE ( 'NONE', *, *, #9300, .T. ) ;
#31556 = CARTESIAN_POINT ( 'NONE',  ( -19.28375372365793083, -189.7472609257535510, 121.5427093402341114 ) ) ;
#31555 = DIRECTION ( 'NONE',  ( -0.000000000000000000, 1.000000000000000000, -0.000000000000000000 ) ) ;
#31558 = VECTOR ( 'NONE', #12107, 1000.000000000000114 ) ;
#31559 = AXIS2_PLACEMENT_3D ( 'NONE', #40561, #20604, #46104 ) ;
#31560 = DIRECTION ( 'NONE',  ( 0.000000000000000000, 0.000000000000000000, 1.000000000000000000 ) ) ;
#31562 = VERTEX_POINT ( 'NONE', #29388 ) ;
#31561 = VECTOR ( 'NONE', #30239, 1000.000000000000000 ) ;
#31563 = CARTESIAN_POINT ( 'NONE',  ( -172.1341525481709880, -175.3837268820161057, 18.28755301364337527 ) ) ;
#31564 = ORIENTED_EDGE ( 'NONE', *, *, #15276, .T. ) ;
#31565 = DIRECTION ( 'NONE',  ( -0.1182731709213730997, 0.000000000000000000, 0.9929810960135161402 ) ) ;
#31566 = AXIS2_PLACEMENT_3D ( 'NONE', #19177, #19680, #35445 ) ;
#31567 = DIRECTION ( 'NONE',  ( 1.000000000000000000, -0.000000000000000000, -0.000000000000000000 ) ) ;
#31569 = DIRECTION ( 'NONE',  ( 0.000000000000000000, -1.000000000000000000, 0.000000000000000000 ) ) ;
#31568 = FACE_OUTER_BOUND ( 'NONE', #14906, .T. ) ;
#31570 = EDGE_LOOP ( 'NONE', ( #23530, #47084, #15231, #22291 ) ) ;
#31571 = EDGE_CURVE ( 'NONE', #17630, #23609, #29648, .T. ) ;
#31572 = AXIS2_PLACEMENT_3D ( 'NONE', #1992, #50357, #18033 ) ;
#31573 = DIRECTION ( 'NONE',  ( 0.4566292373937018145, 0.000000000000000000, 0.8896570909947529859 ) ) ;
#31574 = DIRECTION ( 'NONE',  ( 0.000000000000000000, -1.000000000000000000, 0.000000000000000000 ) ) ;
#31575 = ORIENTED_EDGE ( 'NONE', *, *, #35489, .T. ) ;
#31576 = DIRECTION ( 'NONE',  ( 1.000000000000000000, 0.000000000000000000, 0.000000000000000000 ) ) ;
#31577 = DIRECTION ( 'NONE',  ( -0.9995608365087946812, 0.000000000000000000, 0.02963332782254913048 ) ) ;
#31578 = ORIENTED_EDGE ( 'NONE', *, *, #21148, .T. ) ;
#31579 = EDGE_CURVE ( 'NONE', #46831, #44523, #12982, .T. ) ;
#31580 = DIRECTION ( 'NONE',  ( 5.399917434947259359E-17, 1.000000000000000000, -0.000000000000000000 ) ) ;
#31581 = DIRECTION ( 'NONE',  ( -0.000000000000000000, -0.7485107481711046340, -0.6631226582407911962 ) ) ;
#31582 = CARTESIAN_POINT ( 'NONE',  ( -330.4913330509368166, -102.1108035431478811, -54.98865587491830809 ) ) ;
#31583 = EDGE_LOOP ( 'NONE', ( #17805, #24337, #36945, #11963 ) ) ;
#31584 = DIRECTION ( 'NONE',  ( -0.000000000000000000, 0.6631226582407937498, -0.7485107481711024136 ) ) ;
#31585 = ORIENTED_EDGE ( 'NONE', *, *, #2093, .T. ) ;
#31586 = EDGE_CURVE ( 'NONE', #47414, #49045, #25713, .T. ) ;
#31587 = VECTOR ( 'NONE', #49584, 1000.000000000000000 ) ;
#31588 = CARTESIAN_POINT ( 'NONE',  ( -124.1938582159088469, -175.3837268820161057, -99.45993886622792957 ) ) ;
#31589 = DIRECTION ( 'NONE',  ( 0.000000000000000000, 0.000000000000000000, -1.000000000000000000 ) ) ;
#31590 = AXIS2_PLACEMENT_3D ( 'NONE', #39053, #22539, #6764 ) ;
#31591 = CARTESIAN_POINT ( 'NONE',  ( -168.4003408533108086, -183.6283474603465606, -35.26900067126609173 ) ) ;
#31592 = DIRECTION ( 'NONE',  ( -0.000000000000000000, 1.000000000000000000, -0.000000000000000000 ) ) ;
#31593 = CARTESIAN_POINT ( 'NONE',  ( -330.4913330509368166, -179.4217241332784454, -21.74306257088698757 ) ) ;
#31594 = PLANE ( 'NONE',  #23785 ) ;
#31595 = CIRCLE ( 'NONE', #14859, 125.0000000000000000 ) ;
#31596 = VECTOR ( 'NONE', #16272, 999.9999999999998863 ) ;
#31597 = FACE_OUTER_BOUND ( 'NONE', #29037, .T. ) ;
#31598 = EDGE_CURVE ( 'NONE', #17396, #2622, #4707, .T. ) ;
#31599 = CARTESIAN_POINT ( 'NONE',  ( 8.448131207122518305, -189.7472609257535510, 111.2847127925100068 ) ) ;
#31601 = VERTEX_POINT ( 'NONE', #45698 ) ;
#31600 = DIRECTION ( 'NONE',  ( 0.000000000000000000, -1.000000000000000000, 0.000000000000000000 ) ) ;
#31602 = VECTOR ( 'NONE', #47000, 1000.000000000000000 ) ;
#31603 = CIRCLE ( 'NONE', #16503, 125.0000000000000000 ) ;
#31604 = ORIENTED_EDGE ( 'NONE', *, *, #23287, .F. ) ;
#31605 = EDGE_CURVE ( 'NONE', #6500, #37405, #28927, .T. ) ;
#31606 = CARTESIAN_POINT ( 'NONE',  ( -95.72791768350688812, -177.1207230881787780, -115.7261930397105090 ) ) ;
#31607 = VECTOR ( 'NONE', #29024, 1000.000000000000000 ) ;
#31608 = AXIS2_PLACEMENT_3D ( 'NONE', #46331, #2439, #50530 ) ;
#31609 = LINE ( 'NONE', #47660, #22080 ) ;
#31610 = EDGE_LOOP ( 'NONE', ( #17225, #28381, #50390, #4160 ) ) ;
#31611 = ORIENTED_EDGE ( 'NONE', *, *, #32113, .F. ) ;
#31612 = CARTESIAN_POINT ( 'NONE',  ( -48.47912675150885065, -177.1207230881787780, 6.938893903907228378E-15 ) ) ;
#31613 = EDGE_LOOP ( 'NONE', ( #24661, #42573, #4370, #14087 ) ) ;
#31614 = LINE ( 'NONE', #43706, #18342 ) ;
#31615 = DIRECTION ( 'NONE',  ( -0.5338233779647887367, 0.000000000000000000, -0.8455960035018273979 ) ) ;
#31616 = CARTESIAN_POINT ( 'NONE',  ( 8.879953965148883910, -189.7472609257535510, 109.9360785596608707 ) ) ;
#31617 = CARTESIAN_POINT ( 'NONE',  ( 44.30815888362531041, -189.7472609257535510, 83.75869879877569701 ) ) ;
#31618 = EDGE_LOOP ( 'NONE', ( #452, #51185, #829, #10176 ) ) ;
#31619 = ORIENTED_EDGE ( 'NONE', *, *, #1149, .F. ) ;
#31620 = ORIENTED_EDGE ( 'NONE', *, *, #8110, .F. ) ;
#31621 = CARTESIAN_POINT ( 'NONE',  ( -332.3517673607765914, -123.5000000000000284, 0.000000000000000000 ) ) ;
#31622 = LINE ( 'NONE', #35061, #21005 ) ;
#31623 = CIRCLE ( 'NONE', #3952, 60.00000000000000000 ) ;
#31624 = DIRECTION ( 'NONE',  ( -0.000000000000000000, 0.8229838658936556861, -0.5680647467311569221 ) ) ;
#31625 = DIRECTION ( 'NONE',  ( 0.000000000000000000, 0.000000000000000000, -1.000000000000000000 ) ) ;
#31626 = DIRECTION ( 'NONE',  ( -1.000000000000000000, 0.000000000000000000, -0.000000000000000000 ) ) ;
#31627 = VERTEX_POINT ( 'NONE', #9433 ) ;
#31628 = DIRECTION ( 'NONE',  ( 0.000000000000000000, -0.000000000000000000, 1.000000000000000000 ) ) ;
#31629 = VECTOR ( 'NONE', #35902, 999.9999999999998863 ) ;
#31630 = EDGE_CURVE ( 'NONE', #9931, #22453, #9622, .T. ) ;
#31631 = UNCERTAINTY_MEASURE_WITH_UNIT (LENGTH_MEASURE( 1.000000000000000082E-05 ), #33419, 'distance_accuracy_value', 'NONE');
#31632 = DIRECTION ( 'NONE',  ( 0.000000000000000000, 0.000000000000000000, 1.000000000000000000 ) ) ;
#31633 = ORIENTED_EDGE ( 'NONE', *, *, #48797, .T. ) ;
#31634 = ORIENTED_EDGE ( 'NONE', *, *, #2103, .T. ) ;
#31635 = VECTOR ( 'NONE', #9596, 1000.000000000000000 ) ;
#31636 = ORIENTED_EDGE ( 'NONE', *, *, #49998, .T. ) ;
#31637 = DIRECTION ( 'NONE',  ( -0.1768902751225802927, 0.000000000000000000, 0.9842305779475953864 ) ) ;
#31638 = PLANE ( 'NONE',  #14919 ) ;
#31639 = CIRCLE ( 'NONE', #35842, 4.999999999999997335 ) ;
#31640 = VERTEX_POINT ( 'NONE', #1545 ) ;
#31641 = CARTESIAN_POINT ( 'NONE',  ( -332.3517673607765914, -123.5000000000000284, 0.000000000000000000 ) ) ;
#31642 = VECTOR ( 'NONE', #36613, 1000.000000000000114 ) ;
#31643 = CIRCLE ( 'NONE', #37498, 60.00000000000000000 ) ;
#31644 = CARTESIAN_POINT ( 'NONE',  ( -332.3517673607765914, -117.8908635894569272, -59.73723787327232060 ) ) ;
#31645 = DIRECTION ( 'NONE',  ( -0.000000000000000000, 0.000000000000000000, -1.000000000000000000 ) ) ;
#31646 = ORIENTED_EDGE ( 'NONE', *, *, #42687, .F. ) ;
#31647 = ADVANCED_FACE ( 'NONE', ( #20999 ), #13107, .T. ) ;
#31648 = CARTESIAN_POINT ( 'NONE',  ( 30.00000000000000711, -43.50000000000000000, 30.00000000000000355 ) ) ;
#31649 = COLOUR_RGB ( '', 0.40784314, 0.44705882, 0.49803922) ;
#31650 = EDGE_CURVE ( 'NONE', #39961, #39674, #37020, .T. ) ;
#31651 = ADVANCED_FACE ( 'NONE', ( #20739 ), #33855, .T. ) ;
#31652 = AXIS2_PLACEMENT_3D ( 'NONE', #30474, #19174, #30227 ) ;
#31653 = ORIENTED_EDGE ( 'NONE', *, *, #626, .T. ) ;
#31654 = DIRECTION ( 'NONE',  ( 0.000000000000000000, 0.000000000000000000, -1.000000000000000000 ) ) ;
#31655 = EDGE_CURVE ( 'NONE', #15345, #16448, #11290, .T. ) ;
#31656 = EDGE_CURVE ( 'NONE', #2545, #44250, #47398, .T. ) ;
#31657 = LINE ( 'NONE', #27182, #48839 ) ;
#31658 = ORIENTED_EDGE ( 'NONE', *, *, #31162, .F. ) ;
#31659 = FACE_OUTER_BOUND ( 'NONE', #40129, .T. ) ;
#31660 = DIRECTION ( 'NONE',  ( 1.000000000000000000, -0.000000000000000000, 0.000000000000000000 ) ) ;
#31661 = DIRECTION ( 'NONE',  ( 0.000000000000000000, 0.000000000000000000, -1.000000000000000000 ) ) ;
#31662 = DIRECTION ( 'NONE',  ( 0.000000000000000000, 0.000000000000000000, 1.000000000000000000 ) ) ;
#31663 = ORIENTED_EDGE ( 'NONE', *, *, #8216, .T. ) ;
#31664 = CARTESIAN_POINT ( 'NONE',  ( -339.1964088526558498, -151.3613951634084742, 52.00954392751779665 ) ) ;
#31665 = ORIENTED_EDGE ( 'NONE', *, *, #49465, .T. ) ;
#31666 = ORIENTED_EDGE ( 'NONE', *, *, #52036, .T. ) ;
#31667 = CIRCLE ( 'NONE', #40059, 125.0000000000000000 ) ;
#31668 = AXIS2_PLACEMENT_3D ( 'NONE', #2402, #34956, #51022 ) ;
#31669 = CARTESIAN_POINT ( 'NONE',  ( -3.104056038602976741, -193.5000000000000000, -115.4006183233321678 ) ) ;
#31671 = ORIENTED_EDGE ( 'NONE', *, *, #8331, .T. ) ;
#31670 = DIRECTION ( 'NONE',  ( 0.000000000000000000, 6.938893903907228378E-14, -1.000000000000000000 ) ) ;
#31672 = VECTOR ( 'NONE', #36392, 1000.000000000000000 ) ;
#31673 = ORIENTED_EDGE ( 'NONE', *, *, #21553, .F. ) ;
#31674 = PLANE ( 'NONE',  #27943 ) ;
#31675 = CARTESIAN_POINT ( 'NONE',  ( 0.000000000000000000, -43.50000000000000000, -60.00000000000000711 ) ) ;
#31676 = VECTOR ( 'NONE', #30633, 1000.000000000000114 ) ;
#31677 = ORIENTED_EDGE ( 'NONE', *, *, #14581, .T. ) ;
#31678 = CARTESIAN_POINT ( 'NONE',  ( -332.3517673607765914, -76.43926241122620979, -35.68215131113738181 ) ) ;
#31679 = CIRCLE ( 'NONE', #40076, 125.0000000000000000 ) ;
#31680 = DIRECTION ( 'NONE',  ( -0.000000000000000000, 0.000000000000000000, -1.000000000000000000 ) ) ;
#31681 = ORIENTED_EDGE ( 'NONE', *, *, #46940, .T. ) ;
#31682 = DIRECTION ( 'NONE',  ( 0.000000000000000000, 0.000000000000000000, 1.000000000000000000 ) ) ;
#31683 = CARTESIAN_POINT ( 'NONE',  ( -260.0000000000000000, -113.5000000000000000, 60.00000000000000711 ) ) ;
#31684 = CIRCLE ( 'NONE', #19093, 60.00000000000000000 ) ;
#31685 = AXIS2_PLACEMENT_3D ( 'NONE', #51503, #22617, #15502 ) ;
#31686 = CARTESIAN_POINT ( 'NONE',  ( -339.1964088526558498, -131.1080185721133660, -58.50955523165751515 ) ) ;
#31687 = CARTESIAN_POINT ( 'NONE',  ( -63.09433862318517328, -193.5000000000000000, -124.1426420773539405 ) ) ;
#31688 = ORIENTED_EDGE ( 'NONE', *, *, #4534, .F. ) ;
#31689 = ORIENTED_EDGE ( 'NONE', *, *, #23700, .T. ) ;
#31690 = ORIENTED_EDGE ( 'NONE', *, *, #6729, .F. ) ;
#31691 = AXIS2_PLACEMENT_3D ( 'NONE', #19994, #47613, #31828 ) ;
#31692 = CARTESIAN_POINT ( 'NONE',  ( -142.3192003680973414, -177.1207230881787780, 82.57748230379304744 ) ) ;
#31693 = CARTESIAN_POINT ( 'NONE',  ( -339.1964088526558498, -137.1341532842523065, 57.40522506028101901 ) ) ;
#31694 = DIRECTION ( 'NONE',  ( 0.5338233779647826305, 0.000000000000000000, 0.8455960035018311727 ) ) ;
#31695 = CARTESIAN_POINT ( 'NONE',  ( -88.23625491228470707, -183.6283474603465606, 118.5089480183148254 ) ) ;
#31696 = CYLINDRICAL_SURFACE ( 'NONE', #39808, 125.0000000000000000 ) ;
#31697 = ORIENTED_EDGE ( 'NONE', *, *, #9639, .T. ) ;
#31698 = EDGE_CURVE ( 'NONE', #22737, #15872, #8785, .T. ) ;
#31699 = EDGE_CURVE ( 'NONE', #39182, #41471, #13628, .T. ) ;
#31700 = EDGE_CURVE ( 'NONE', #37972, #22789, #34117, .T. ) ;
#31701 = EDGE_CURVE ( 'NONE', #1446, #10636, #38048, .T. ) ;
#31702 = LINE ( 'NONE', #31177, #32462 ) ;
#31703 = ORIENTED_EDGE ( 'NONE', *, *, #26777, .T. ) ;
#31705 = EDGE_LOOP ( 'NONE', ( #22416, #51098, #4736, #29310 ) ) ;
#31704 = CARTESIAN_POINT ( 'NONE',  ( 12.99855592850622443, -183.6283474603465606, 108.8370090194294875 ) ) ;
#31706 = CIRCLE ( 'NONE', #8185, 125.0000000000000000 ) ;
#31707 = VERTEX_POINT ( 'NONE', #22027 ) ;
#31708 = CIRCLE ( 'NONE', #9063, 60.00000000000000000 ) ;
#31709 = LINE ( 'NONE', #28525, #17407 ) ;
#31710 = EDGE_CURVE ( 'NONE', #2676, #1973, #9957, .T. ) ;
#31711 = FACE_OUTER_BOUND ( 'NONE', #16366, .T. ) ;
#31712 = VECTOR ( 'NONE', #47668, 1000.000000000000114 ) ;
#31713 = CARTESIAN_POINT ( 'NONE',  ( -56.05401443572781517, -189.7472609257535510, 124.7702732086913073 ) ) ;
#31714 = LINE ( 'NONE', #30936, #741 ) ;
#31715 = ORIENTED_EDGE ( 'NONE', *, *, #19417, .F. ) ;
#31716 = EDGE_CURVE ( 'NONE', #24085, #48695, #14162, .T. ) ;
#31717 = DIRECTION ( 'NONE',  ( 0.000000000000000000, -0.000000000000000000, -1.000000000000000000 ) ) ;
#31718 = ORIENTED_EDGE ( 'NONE', *, *, #30765, .F. ) ;
#31719 = EDGE_CURVE ( 'NONE', #27526, #37757, #44925, .T. ) ;
#31720 = ORIENTED_EDGE ( 'NONE', *, *, #7360, .T. ) ;
#31721 = DIRECTION ( 'NONE',  ( 0.8124868780056825335, 0.000000000000000000, -0.5829794791144703447 ) ) ;
#31722 = AXIS2_PLACEMENT_3D ( 'NONE', #21150, #12731, #49801 ) ;
#31723 = ADVANCED_FACE ( 'NONE', ( #10197 ), #38576, .F. ) ;
#31724 = LINE ( 'NONE', #31969, #23647 ) ;
#31725 = DIRECTION ( 'NONE',  ( 1.000000000000000000, -0.000000000000000000, -0.000000000000000000 ) ) ;
#31726 = CARTESIAN_POINT ( 'NONE',  ( -330.4913330509368166, -123.5000000000000284, 0.000000000000000000 ) ) ;
#31727 = EDGE_CURVE ( 'NONE', #43845, #18286, #30180, .T. ) ;
#31728 = CARTESIAN_POINT ( 'NONE',  ( -48.47912675150885065, -189.7472609257535510, 6.938893903907228378E-15 ) ) ;
#31729 = DIRECTION ( 'NONE',  ( 1.000000000000000000, -0.000000000000000000, 0.000000000000000000 ) ) ;
#31730 = VERTEX_POINT ( 'NONE', #7040 ) ;
#31731 = CARTESIAN_POINT ( 'NONE',  ( -170.0000000000000284, -115.7896721143442278, -18.45401972188387418 ) ) ;
#31732 = DIRECTION ( 'NONE',  ( -1.000000000000000000, 0.000000000000000000, 0.000000000000000000 ) ) ;
#31733 = VECTOR ( 'NONE', #35179, 1000.000000000000114 ) ;
#31734 = FACE_BOUND ( 'NONE', #33203, .T. ) ;
#31735 = ORIENTED_EDGE ( 'NONE', *, *, #25356, .T. ) ;
#31736 = DIRECTION ( 'NONE',  ( 0.000000000000000000, -1.000000000000000000, 0.000000000000000000 ) ) ;
#31737 = DIRECTION ( 'NONE',  ( 0.000000000000000000, 1.000000000000000000, 0.000000000000000000 ) ) ;
#31738 = ORIENTED_EDGE ( 'NONE', *, *, #2542, .F. ) ;
#31739 = CARTESIAN_POINT ( 'NONE',  ( -339.1964088526558498, -109.8658467157473666, -57.40522506028092664 ) ) ;
#31740 = ORIENTED_EDGE ( 'NONE', *, *, #42081, .T. ) ;
#31741 = EDGE_CURVE ( 'NONE', #10636, #41581, #14412, .T. ) ;
#31742 = AXIS2_PLACEMENT_3D ( 'NONE', #3714, #31843, #8438 ) ;
#31743 = DIRECTION ( 'NONE',  ( 0.4566292373937018145, 0.000000000000000000, 0.8896570909947529859 ) ) ;
#31744 = VECTOR ( 'NONE', #44576, 1000.000000000000114 ) ;
#31745 = VECTOR ( 'NONE', #11836, 1000.000000000000000 ) ;
#31746 = FACE_BOUND ( 'NONE', #38039, .T. ) ;
#31748 = ORIENTED_EDGE ( 'NONE', *, *, #5168, .T. ) ;
#31747 = FACE_OUTER_BOUND ( 'NONE', #38270, .T. ) ;
#31749 = CIRCLE ( 'NONE', #49399, 124.9999999999999858 ) ;
#31750 = CARTESIAN_POINT ( 'NONE',  ( 52.59568867645218404, -193.5000000000000000, -73.54509967498589162 ) ) ;
#31751 = ORIENTED_EDGE ( 'NONE', *, *, #21827, .T. ) ;
#31752 = ORIENTED_EDGE ( 'NONE', *, *, #22119, .F. ) ;
#31753 = EDGE_CURVE ( 'NONE', #42165, #38881, #46222, .T. ) ;
#31754 = DIRECTION ( 'NONE',  ( 0.8455960035018234011, 0.000000000000000000, 0.5338233779647948429 ) ) ;
#31755 = CIRCLE ( 'NONE', #24187, 20.00000000000000000 ) ;
#31756 = EDGE_LOOP ( 'NONE', ( #20354, #17571, #45094, #35148 ) ) ;
#31757 = PLANE ( 'NONE',  #47744 ) ;
#31758 = LINE ( 'NONE', #40154, #17978 ) ;
#31759 = EDGE_CURVE ( 'NONE', #39207, #21817, #46993, .T. ) ;
#31760 = EDGE_CURVE ( 'NONE', #5462, #20620, #38310, .T. ) ;
#31761 = EDGE_CURVE ( 'NONE', #49096, #6252, #10449, .T. ) ;
#31762 = EDGE_CURVE ( 'NONE', #40799, #12141, #18359, .T. ) ;
#31763 = ADVANCED_FACE ( 'NONE', ( #30674 ), #46729, .F. ) ;
#31764 = AXIS2_PLACEMENT_3D ( 'NONE', #31244, #47297, #19946 ) ;
#31765 = DIRECTION ( 'NONE',  ( 0.000000000000000000, -1.000000000000000000, 0.000000000000000000 ) ) ;
#31766 = CARTESIAN_POINT ( 'NONE',  ( -26.20043062753592977, -193.5000000000000000, -122.9986166548863196 ) ) ;
#31767 = ORIENTED_EDGE ( 'NONE', *, *, #29562, .F. ) ;
#31770 = ORIENTED_EDGE ( 'NONE', *, *, #31571, .F. ) ;
#31769 = LINE ( 'NONE', #16790, #46592 ) ;
#31768 = LINE ( 'NONE', #19665, #31733 ) ;
#31771 = EDGE_CURVE ( 'NONE', #9203, #39625, #26744, .T. ) ;
#31772 = LINE ( 'NONE', #43594, #44098 ) ;
#31773 = ORIENTED_EDGE ( 'NONE', *, *, #18555, .T. ) ;
#31774 = PLANE ( 'NONE',  #19728 ) ;
#31775 = ORIENTED_EDGE ( 'NONE', *, *, #12136, .T. ) ;
#31776 = PLANE ( 'NONE',  #15840 ) ;
#31777 = VERTEX_POINT ( 'NONE', #10972 ) ;
#31778 = EDGE_CURVE ( 'NONE', #27687, #21993, #14685, .T. ) ;
#31780 = CARTESIAN_POINT ( 'NONE',  ( -45.06671089634842531, -183.6283474603465606, -124.9534129907280686 ) ) ;
#31779 = PLANE ( 'NONE',  #22483 ) ;
#31781 = ORIENTED_EDGE ( 'NONE', *, *, #7479, .T. ) ;
#31782 = ADVANCED_FACE ( 'NONE', ( #43032 ), #50936, .T. ) ;
#31783 = DIRECTION ( 'NONE',  ( -0.000000000000000000, -1.000000000000000000, -0.000000000000000000 ) ) ;
#31784 = VERTEX_POINT ( 'NONE', #23066 ) ;
#31785 = CARTESIAN_POINT ( 'NONE',  ( -171.2399149993172500, -193.5000000000000000, -17.48697739784459415 ) ) ;
#31786 = CIRCLE ( 'NONE', #4936, 125.0000000000000000 ) ;
#31787 = DIRECTION ( 'NONE',  ( 0.000000000000000000, 0.000000000000000000, 1.000000000000000000 ) ) ;
#31788 = EDGE_CURVE ( 'NONE', #22776, #48106, #39076, .T. ) ;
#31789 = AXIS2_PLACEMENT_3D ( 'NONE', #28324, #31765, #35963 ) ;
#31790 = DIRECTION ( 'NONE',  ( -0.7765238627180482966, 0.000000000000000000, 0.6300878435817038881 ) ) ;
#31791 = LINE ( 'NONE', #8642, #30006 ) ;
#31792 = FACE_OUTER_BOUND ( 'NONE', #12298, .T. ) ;
#31793 = CIRCLE ( 'NONE', #25087, 125.0000000000000000 ) ;
#31794 = DIRECTION ( 'NONE',  ( 0.9027978299657446470, 0.000000000000000000, -0.4300652022765183435 ) ) ;
#31795 = ADVANCED_FACE ( 'NONE', ( #39343 ), #3348, .T. ) ;
#31796 = ORIENTED_EDGE ( 'NONE', *, *, #19759, .F. ) ;
#31797 = DIRECTION ( 'NONE',  ( 0.000000000000000000, 0.000000000000000000, 1.000000000000000000 ) ) ;
#31798 = DIRECTION ( 'NONE',  ( -0.000000000000000000, -0.9927088740980548609, -0.1205366802553164696 ) ) ;
#31799 = DIRECTION ( 'NONE',  ( -0.9564009842765264224, 0.000000000000000000, 0.2920567706369628924 ) ) ;
#31800 = ADVANCED_FACE ( 'NONE', ( #7298 ), #47766, .F. ) ;
#31801 = DIRECTION ( 'NONE',  ( -0.000000000000000000, 1.000000000000000000, -0.000000000000000000 ) ) ;
#31802 = ORIENTED_EDGE ( 'NONE', *, *, #3640, .F. ) ;
#31803 = AXIS2_PLACEMENT_3D ( 'NONE', #21744, #29875, #45935 ) ;
#31804 = CARTESIAN_POINT ( 'NONE',  ( -64.08700758308647494, -189.7472609257535510, -124.0217483183786840 ) ) ;
#31805 = CARTESIAN_POINT ( 'NONE',  ( -336.3521761649654422, -168.7445418633863596, -37.90245108779149064 ) ) ;
#31807 = EDGE_LOOP ( 'NONE', ( #41278, #14804, #9295, #4621 ) ) ;
#31806 = CARTESIAN_POINT ( 'NONE',  ( -305.0000000000000568, -123.5000000000000284, 0.000000000000000000 ) ) ;
#31808 = ORIENTED_EDGE ( 'NONE', *, *, #20635, .T. ) ;
#31809 = ORIENTED_EDGE ( 'NONE', *, *, #11718, .T. ) ;
#31810 = EDGE_LOOP ( 'NONE', ( #24551, #12606, #36915, #41841 ) ) ;
#31811 = ADVANCED_FACE ( 'NONE', ( #28023 ), #15187, .F. ) ;
#31812 = CARTESIAN_POINT ( 'NONE',  ( -159.5526844214375615, -177.1207230881787780, 57.33816169485226055 ) ) ;
#31813 = LINE ( 'NONE', #23652, #23723 ) ;
#31814 = DIRECTION ( 'NONE',  ( -0.000000000000000000, 0.8854560256532157947, 0.4647231720437573488 ) ) ;
#31815 = ORIENTED_EDGE ( 'NONE', *, *, #23595, .T. ) ;
#31816 = CARTESIAN_POINT ( 'NONE',  ( 2.957638829135800673, 51.44316066764527307, -20.60505050678383654 ) ) ;
#31817 = EDGE_LOOP ( 'NONE', ( #36964, #31980 ) ) ;
#31818 = ORIENTED_EDGE ( 'NONE', *, *, #46567, .F. ) ;
#31819 = AXIS2_PLACEMENT_3D ( 'NONE', #10738, #22825, #42794 ) ;
#31820 = ORIENTED_EDGE ( 'NONE', *, *, #50052, .T. ) ;
#31821 = DIRECTION ( 'NONE',  ( -0.000000000000000000, 1.000000000000000000, -0.000000000000000000 ) ) ;
#31822 = CIRCLE ( 'NONE', #3314, 125.0000000000000000 ) ;
#31823 = EDGE_CURVE ( 'NONE', #29476, #728, #15710, .T. ) ;
#31824 = EDGE_CURVE ( 'NONE', #13870, #29270, #22255, .T. ) ;
#31825 = ORIENTED_EDGE ( 'NONE', *, *, #10118, .T. ) ;
#31826 = CARTESIAN_POINT ( 'NONE',  ( -173.0563034899574859, -189.7472609257535510, -10.27263529369817618 ) ) ;
#31827 = DIRECTION ( 'NONE',  ( 0.000000000000000000, 1.000000000000000000, 0.000000000000000000 ) ) ;
#31830 = ORIENTED_EDGE ( 'NONE', *, *, #49747, .F. ) ;
#31829 = CARTESIAN_POINT ( 'NONE',  ( 0.000000000000000000, -162.6242368362071602, -44.16213414209478572 ) ) ;
#31828 = DIRECTION ( 'NONE',  ( 0.000000000000000000, 0.000000000000000000, 1.000000000000000000 ) ) ;
#31831 = FACE_OUTER_BOUND ( 'NONE', #49510, .T. ) ;
#31832 = EDGE_LOOP ( 'NONE', ( #47892, #46961, #34358, #34505 ) ) ;
#31833 = DIRECTION ( 'NONE',  ( -0.000000000000000000, 1.000000000000000000, -0.000000000000000000 ) ) ;
#31834 = ORIENTED_EDGE ( 'NONE', *, *, #36509, .F. ) ;
#31835 = CARTESIAN_POINT ( 'NONE',  ( -59.81005805956441179, -183.6283474603465606, -123.4817304940906126 ) ) ;
#31836 = CARTESIAN_POINT ( 'NONE',  ( -336.3521761649654422, -153.2494431741581025, -51.01861988938816950 ) ) ;
#31838 = DIRECTION ( 'NONE',  ( -0.000000000000000000, 1.000000000000000000, -0.000000000000000000 ) ) ;
#31837 = LINE ( 'NONE', #4240, #19834 ) ;
#31839 = VERTEX_POINT ( 'NONE', #27518 ) ;
#31840 = AXIS2_PLACEMENT_3D ( 'NONE', #21058, #37075, #9494 ) ;
#31841 = DIRECTION ( 'NONE',  ( -0.000000000000000000, 0.4647231720437789981, 0.8854560256532044704 ) ) ;
#31842 = CARTESIAN_POINT ( 'NONE',  ( 43.63512310656540905, -189.7472609257535510, 84.49831343337136502 ) ) ;
#31843 = DIRECTION ( 'NONE',  ( 0.000000000000000000, 0.000000000000000000, 1.000000000000000000 ) ) ;
#31844 = VERTEX_POINT ( 'NONE', #47253 ) ;
#31845 = ADVANCED_FACE ( 'NONE', ( #11222 ), #24355, .T. ) ;
#31846 = DIRECTION ( 'NONE',  ( 0.9564009842765202052, 0.000000000000000000, 0.2920567706369833760 ) ) ;
#31847 = CARTESIAN_POINT ( 'NONE',  ( 48.06131630543706734, -189.7472609257535510, -79.40367028273054473 ) ) ;
#31848 = LINE ( 'NONE', #19747, #19810 ) ;
#31849 = ORIENTED_EDGE ( 'NONE', *, *, #50449, .T. ) ;
#31850 = LINE ( 'NONE', #16086, #33484 ) ;
#31851 = DIRECTION ( 'NONE',  ( 0.000000000000000000, 0.000000000000000000, -1.000000000000000000 ) ) ;
#31852 = ADVANCED_FACE ( 'NONE', ( #27250 ), #47502, .F. ) ;
#31853 = ORIENTED_EDGE ( 'NONE', *, *, #22600, .F. ) ;
#31854 = DIRECTION ( 'NONE',  ( 0.000000000000000000, -1.000000000000000000, 0.000000000000000000 ) ) ;
#31855 = ORIENTED_EDGE ( 'NONE', *, *, #17369, .F. ) ;
#31856 = AXIS2_PLACEMENT_3D ( 'NONE', #26703, #27203, #18560 ) ;
#31857 = DIRECTION ( 'NONE',  ( 0.000000000000000000, -0.000000000000000000, -1.000000000000000000 ) ) ;
#31858 = CARTESIAN_POINT ( 'NONE',  ( -30.00000000000000000, -43.50000000000000000, -0.000000000000000000 ) ) ;
#31859 = AXIS2_PLACEMENT_3D ( 'NONE', #39942, #43651, #3696 ) ;
#31860 = DIRECTION ( 'NONE',  ( 0.000000000000000000, 0.000000000000000000, -1.000000000000000000 ) ) ;
#31861 = CARTESIAN_POINT ( 'NONE',  ( -156.9880281022168447, -193.5000000000000000, -60.01515274640934194 ) ) ;
#31862 = DIRECTION ( 'NONE',  ( 0.000000000000000000, 1.000000000000000000, 0.000000000000000000 ) ) ;
#31863 = PLANE ( 'NONE',  #38027 ) ;
#31864 = FACE_OUTER_BOUND ( 'NONE', #31248, .T. ) ;
#31865 = LINE ( 'NONE', #31599, #16333 ) ;
#31867 = VERTEX_POINT ( 'NONE', #31971 ) ;
#31866 = CARTESIAN_POINT ( 'NONE',  ( -165.5546359831674295, -177.1207230881787780, 43.79868877201492694 ) ) ;
#31868 = ORIENTED_EDGE ( 'NONE', *, *, #49583, .T. ) ;
#31869 = CARTESIAN_POINT ( 'NONE',  ( 46.71972386536815236, 28.00000000000000355, -44.63995836652267712 ) ) ;
#31870 = AXIS2_PLACEMENT_3D ( 'NONE', #46695, #26716, #10165 ) ;
#31871 = CARTESIAN_POINT ( 'NONE',  ( -332.3517673607765914, -171.9335100611925213, 35.41461708323791413 ) ) ;
#31872 = ORIENTED_EDGE ( 'NONE', *, *, #34386, .F. ) ;
#31873 = ORIENTED_EDGE ( 'NONE', *, *, #16609, .T. ) ;
#31874 = ORIENTED_EDGE ( 'NONE', *, *, #3512, .T. ) ;
#31875 = DIRECTION ( 'NONE',  ( 0.1182731709213660498, 0.000000000000000000, -0.9929810960135169173 ) ) ;
#31876 = DIRECTION ( 'NONE',  ( 0.000000000000000000, -1.000000000000000000, 0.000000000000000000 ) ) ;
#31877 = EDGE_CURVE ( 'NONE', #28119, #38913, #43290, .T. ) ;
#31878 = DIRECTION ( 'NONE',  ( -0.000000000000000000, 1.000000000000000000, 0.000000000000000000 ) ) ;
#31879 = CARTESIAN_POINT ( 'NONE',  ( -4.794493649713349015, -175.3837268820161057, -117.1181148702518726 ) ) ;
#31880 = ORIENTED_EDGE ( 'NONE', *, *, #9942, .F. ) ;
#31881 = ORIENTED_EDGE ( 'NONE', *, *, #34534, .T. ) ;
#31882 = ORIENTED_EDGE ( 'NONE', *, *, #48467, .T. ) ;
#31883 = LINE ( 'NONE', #39503, #1451 ) ;
#31884 = CARTESIAN_POINT ( 'NONE',  ( -23.99795575808070325, -183.6283474603465606, -122.5792489240757561 ) ) ;
#31885 = CARTESIAN_POINT ( 'NONE',  ( 5.015379008610432621, -177.1207230881787780, -112.9749434763326832 ) ) ;
#31886 = AXIS2_PLACEMENT_3D ( 'NONE', #18117, #34143, #29673 ) ;
#31887 = LINE ( 'NONE', #7966, #4391 ) ;
#31888 = DIRECTION ( 'NONE',  ( 0.000000000000000000, 1.000000000000000000, 0.000000000000000000 ) ) ;
#31889 = EDGE_LOOP ( 'NONE', ( #47288, #9742, #21122, #20634 ) ) ;
#31890 = CARTESIAN_POINT ( 'NONE',  ( 15.23368049493604381, -193.5000000000000000, -107.5438431188757420 ) ) ;
#31891 = DIRECTION ( 'NONE',  ( 0.000000000000000000, 0.000000000000000000, -1.000000000000000000 ) ) ;
#31892 = LINE ( 'NONE', #11909, #27335 ) ;
#31893 = CARTESIAN_POINT ( 'NONE',  ( -12.42681898335384538, -189.7472609257535510, 118.6432945265039507 ) ) ;
#31894 = ORIENTED_EDGE ( 'NONE', *, *, #50392, .T. ) ;
#31895 = EDGE_LOOP ( 'NONE', ( #22786, #21811, #48987, #38715 ) ) ;
#31896 = ORIENTED_EDGE ( 'NONE', *, *, #16841, .T. ) ;
#31897 = DIRECTION ( 'NONE',  ( 0.000000000000000000, 0.000000000000000000, 1.000000000000000000 ) ) ;
#31898 = LINE ( 'NONE', #350, #1477 ) ;
#31899 = ORIENTED_EDGE ( 'NONE', *, *, #5689, .F. ) ;
#31900 = EDGE_CURVE ( 'NONE', #40482, #46919, #39845, .T. ) ;
#31901 = PLANE ( 'NONE',  #50905 ) ;
#31902 = PLANE ( 'NONE',  #8581 ) ;
#31903 = DIRECTION ( 'NONE',  ( 1.000000000000000000, 0.000000000000000000, 0.000000000000000000 ) ) ;
#31904 = ORIENTED_EDGE ( 'NONE', *, *, #12668, .F. ) ;
#31905 = CYLINDRICAL_SURFACE ( 'NONE', #46058, 5.000000000000001776 ) ;
#31906 = VECTOR ( 'NONE', #6182, 1000.000000000000000 ) ;
#31907 = AXIS2_PLACEMENT_3D ( 'NONE', #11870, #51325, #31331 ) ;
#31908 = ORIENTED_EDGE ( 'NONE', *, *, #38757, .F. ) ;
#31909 = CARTESIAN_POINT ( 'NONE',  ( -45.12595152424216138, -193.5000000000000000, -123.9551692589637213 ) ) ;
#31910 = DIRECTION ( 'NONE',  ( 0.000000000000000000, 0.000000000000000000, -1.000000000000000000 ) ) ;
#31911 = CARTESIAN_POINT ( 'NONE',  ( 74.60098876342242136, -193.5000000000000000, 21.82395850507348811 ) ) ;
#31912 = ORIENTED_EDGE ( 'NONE', *, *, #51103, .T. ) ;
#31913 = CARTESIAN_POINT ( 'NONE',  ( -336.3521761649654422, -165.9166037625627439, 41.09453333279358134 ) ) ;
#31914 = DIRECTION ( 'NONE',  ( 0.1768902751225592818, 0.000000000000000000, 0.9842305779475992722 ) ) ;
#31915 = CARTESIAN_POINT ( 'NONE',  ( 60.00000000000001421, -173.5000000000000284, -60.00000000000001421 ) ) ;
#31916 = ADVANCED_FACE ( 'NONE', ( #39587 ), #43800, .T. ) ;
#31917 = CARTESIAN_POINT ( 'NONE',  ( 24.15597040328004752, -177.1207230881787780, -101.7307360698543874 ) ) ;
#31918 = EDGE_LOOP ( 'NONE', ( #21831, #3253, #29729, #47349 ) ) ;
#31919 = LINE ( 'NONE', #27975, #950 ) ;
#31920 = ORIENTED_EDGE ( 'NONE', *, *, #10367, .T. ) ;
#31921 = EDGE_LOOP ( 'NONE', ( #14224, #43431, #48509, #28123 ) ) ;
#31922 = CIRCLE ( 'NONE', #21016, 125.0000000000000000 ) ;
#31923 = CARTESIAN_POINT ( 'NONE',  ( 48.66843973345087448, 35.00000000000000000, -40.95752564483601788 ) ) ;
#31925 = ORIENTED_EDGE ( 'NONE', *, *, #4453, .F. ) ;
#31924 = CARTESIAN_POINT ( 'NONE',  ( -112.7586829773731267, -189.7472609257535510, -107.2060569716373379 ) ) ;
#31926 = EDGE_CURVE ( 'NONE', #47587, #7980, #16215, .T. ) ;
#31927 = EDGE_LOOP ( 'NONE', ( #25412, #31934, #13162, #10246 ) ) ;
#31928 = LINE ( 'NONE', #16435, #45017 ) ;
#31929 = EDGE_CURVE ( 'NONE', #46931, #20894, #26451, .T. ) ;
#31930 = CARTESIAN_POINT ( 'NONE',  ( -47.63353074800702558, -177.1207230881787780, -0.5338233779647817423 ) ) ;
#31931 = EDGE_LOOP ( 'NONE', ( #48956, #35350, #19045, #46226 ) ) ;
#31932 = DIRECTION ( 'NONE',  ( -0.4639789333096864810, 0.000000000000000000, -0.8858462335218260097 ) ) ;
#31933 = DIRECTION ( 'NONE',  ( 0.000000000000000000, -0.000000000000000000, -1.000000000000000000 ) ) ;
#31934 = ORIENTED_EDGE ( 'NONE', *, *, #42980, .F. ) ;
#31935 = DIRECTION ( 'NONE',  ( 0.000000000000000000, -0.000000000000000000, 1.000000000000000000 ) ) ;
#31936 = DIRECTION ( 'NONE',  ( 0.1182731709213523247, 0.000000000000000000, 0.9929810960135185827 ) ) ;
#31937 = EDGE_CURVE ( 'NONE', #4302, #38037, #19891, .T. ) ;
#31938 = DIRECTION ( 'NONE',  ( -0.000000000000000000, 1.000000000000000000, -0.000000000000000000 ) ) ;
#31939 = DIRECTION ( 'NONE',  ( -0.000000000000000000, 0.9709418174260544543, 0.2393156642875482465 ) ) ;
#31940 = ORIENTED_EDGE ( 'NONE', *, *, #7021, .T. ) ;
#31941 = VERTEX_POINT ( 'NONE', #48010 ) ;
#31942 = ADVANCED_FACE ( 'NONE', ( #11994 ), #24110, .T. ) ;
#31943 = VECTOR ( 'NONE', #16847, 1000.000000000000000 ) ;
#31945 = EDGE_LOOP ( 'NONE', ( #4894, #31245, #43220, #46851 ) ) ;
#31944 = VECTOR ( 'NONE', #43105, 1000.000000000000000 ) ;
#31946 = CARTESIAN_POINT ( 'NONE',  ( -163.3872488209693756, -177.1207230881787780, -49.20491319441543254 ) ) ;
#31947 = CARTESIAN_POINT ( 'NONE',  ( -137.9639882952644143, -193.5000000000000000, 87.27805883780241913 ) ) ;
#31948 = EDGE_CURVE ( 'NONE', #17967, #31195, #8329, .T. ) ;
#31949 = CARTESIAN_POINT ( 'NONE',  ( -78.41101675714241992, -175.3837268820161057, -120.3332351033023286 ) ) ;
#31950 = DIRECTION ( 'NONE',  ( 0.000000000000000000, 0.000000000000000000, -1.000000000000000000 ) ) ;
#31951 = CARTESIAN_POINT ( 'NONE',  ( -101.9736325116273576, -193.5000000000000000, 112.9749434763330811 ) ) ;
#31952 = VERTEX_POINT ( 'NONE', #51201 ) ;
#31953 = CARTESIAN_POINT ( 'NONE',  ( -67.22356632362119910, -183.6283474603465606, -123.5865930638409793 ) ) ;
#31954 = ORIENTED_EDGE ( 'NONE', *, *, #20750, .F. ) ;
#31956 = ORIENTED_EDGE ( 'NONE', *, *, #21761, .F. ) ;
#31955 = CARTESIAN_POINT ( 'NONE',  ( -55.65514169787636689, -175.3837268820161057, -123.7921848946937331 ) ) ;
#31957 = ORIENTED_EDGE ( 'NONE', *, *, #24630, .T. ) ;
#31958 = AXIS2_PLACEMENT_3D ( 'NONE', #33236, #38208, #46125 ) ;
#31959 = CYLINDRICAL_SURFACE ( 'NONE', #9843, 125.0000000000000000 ) ;
#31960 = ADVANCED_FACE ( 'NONE', ( #1678 ), #12768, .T. ) ;
#31961 = PLANE ( 'NONE',  #30827 ) ;
#31962 = DIRECTION ( 'NONE',  ( 0.000000000000000000, 0.000000000000000000, -1.000000000000000000 ) ) ;
#31963 = FACE_OUTER_BOUND ( 'NONE', #15732, .T. ) ;
#31964 = EDGE_LOOP ( 'NONE', ( #29593, #40650, #36884, #31086 ) ) ;
#31965 = CARTESIAN_POINT ( 'NONE',  ( -140.8230258362169707, -189.7472609257535510, 84.24728067916045404 ) ) ;
#31966 = EDGE_LOOP ( 'NONE', ( #40045, #47793, #21728, #43012 ) ) ;
#31967 = VERTEX_POINT ( 'NONE', #28796 ) ;
#31968 = CARTESIAN_POINT ( 'NONE',  ( -40.24578378811990831, -189.7472609257535510, 124.7285535218268251 ) ) ;
#31969 = CARTESIAN_POINT ( 'NONE',  ( -114.9600645115007467, -183.6283474603465606, 105.8550183720738147 ) ) ;
#31970 = LINE ( 'NONE', #48009, #46680 ) ;
#31971 = CARTESIAN_POINT ( 'NONE',  ( -62.97606545226378216, -189.7472609257535510, -123.1496609813404319 ) ) ;
#31972 = AXIS2_PLACEMENT_3D ( 'NONE', #51017, #15012, #11035 ) ;
#31973 = CARTESIAN_POINT ( 'NONE',  ( -332.3517673607765914, -74.01670616005314685, 32.17247266903214609 ) ) ;
#31974 = DIRECTION ( 'NONE',  ( -0.000000000000000000, 1.000000000000000000, -0.000000000000000000 ) ) ;
#31975 = ORIENTED_EDGE ( 'NONE', *, *, #39739, .T. ) ;
#31976 = DIRECTION ( 'NONE',  ( 0.6965510290629982615, 0.000000000000000000, -0.7175072570443298270 ) ) ;
#31977 = DIRECTION ( 'NONE',  ( 0.9646355819083594074, 0.000000000000000000, -0.2635871660690647933 ) ) ;
#31978 = VECTOR ( 'NONE', #34263, 1000.000000000000000 ) ;
#31979 = FACE_BOUND ( 'NONE', #32013, .T. ) ;
#31980 = ORIENTED_EDGE ( 'NONE', *, *, #23359, .F. ) ;
#31981 = LINE ( 'NONE', #8343, #46624 ) ;
#31982 = DIRECTION ( 'NONE',  ( 0.000000000000000000, 0.8229838658936575735, 0.5680647467311540355 ) ) ;
#31983 = ADVANCED_FACE ( 'NONE', ( #48795 ), #1932, .T. ) ;
#31984 = ORIENTED_EDGE ( 'NONE', *, *, #50645, .T. ) ;
#31985 = EDGE_CURVE ( 'NONE', #7370, #45652, #37678, .T. ) ;
#31986 = LINE ( 'NONE', #51723, #12869 ) ;
#31987 = VERTEX_POINT ( 'NONE', #5634 ) ;
#31988 = DIRECTION ( 'NONE',  ( 0.000000000000000000, 1.000000000000000000, -0.000000000000000000 ) ) ;
#31989 = CIRCLE ( 'NONE', #9354, 125.0000000000000000 ) ;
#31990 = FACE_BOUND ( 'NONE', #47036, .T. ) ;
#31992 = ORIENTED_EDGE ( 'NONE', *, *, #40635, .F. ) ;
#31991 = CARTESIAN_POINT ( 'NONE',  ( 20.66186849114819069, -193.5000000000000000, -104.1370384486465070 ) ) ;
#31993 = EDGE_CURVE ( 'NONE', #36416, #36764, #17718, .T. ) ;
#31994 = LINE ( 'NONE', #4161, #8439 ) ;
#31995 = VERTEX_POINT ( 'NONE', #8573 ) ;
#31996 = EDGE_CURVE ( 'NONE', #23080, #33448, #40618, .T. ) ;
#31997 = ORIENTED_EDGE ( 'NONE', *, *, #1897, .T. ) ;
#31998 = CARTESIAN_POINT ( 'NONE',  ( -4.794493649713342798, -175.3837268820161057, -117.1181148702518726 ) ) ;
#31999 = EDGE_CURVE ( 'NONE', #21924, #37305, #4639, .T. ) ;
#32000 = VERTEX_POINT ( 'NONE', #33731 ) ;
#32001 = CARTESIAN_POINT ( 'NONE',  ( 53.56330073376472711, -189.7472609257535510, 72.19655804062050208 ) ) ;
#32002 = LINE ( 'NONE', #16249, #21310 ) ;
#32003 = VECTOR ( 'NONE', #41418, 1000.000000000000000 ) ;
#32004 = EDGE_CURVE ( 'NONE', #12983, #48687, #14286, .T. ) ;
#32005 = VECTOR ( 'NONE', #42720, 1000.000000000000000 ) ;
#32006 = CIRCLE ( 'NONE', #23649, 125.0000000000000000 ) ;
#32007 = FILL_AREA_STYLE_COLOUR ( '', #14996 ) ;
#32008 = DIRECTION ( 'NONE',  ( 0.9842305779475980509, 0.000000000000000000, -0.1768902751225666647 ) ) ;
#32009 = ORIENTED_EDGE ( 'NONE', *, *, #29730, .T. ) ;
#32012 = ORIENTED_EDGE ( 'NONE', *, *, #20678, .T. ) ;
#32011 = FACE_OUTER_BOUND ( 'NONE', #50045, .T. ) ;
#32010 = DIRECTION ( 'NONE',  ( -0.000000000000000000, -1.000000000000000000, -0.000000000000000000 ) ) ;
#32013 = EDGE_LOOP ( 'NONE', ( #11511, #39673, #7376, #39180 ) ) ;
#32014 = CARTESIAN_POINT ( 'NONE',  ( -56.71246971489870958, -189.7472609257535510, -124.7285535218267682 ) ) ;
#32015 = ORIENTED_EDGE ( 'NONE', *, *, #20646, .T. ) ;
#32016 = DIRECTION ( 'NONE',  ( -0.000000000000000000, 1.000000000000000000, -0.000000000000000000 ) ) ;
#32017 = VERTEX_POINT ( 'NONE', #48551 ) ;
#32018 = CARTESIAN_POINT ( 'NONE',  ( -336.3521761649654422, -181.7525362123217292, 9.724760635742144999 ) ) ;
#32019 = ORIENTED_EDGE ( 'NONE', *, *, #8566, .F. ) ;
#32021 = DIRECTION ( 'NONE',  ( 0.000000000000000000, 0.000000000000000000, 1.000000000000000000 ) ) ;
#32020 = CARTESIAN_POINT ( 'NONE',  ( -85.14888725715768203, -193.5000000000000000, 119.5003291395398577 ) ) ;
#32022 = VERTEX_POINT ( 'NONE', #29774 ) ;
#32023 = CIRCLE ( 'NONE', #43769, 60.00000000000000000 ) ;
#32024 = ORIENTED_EDGE ( 'NONE', *, *, #15241, .T. ) ;
#32025 = CARTESIAN_POINT ( 'NONE',  ( -144.2430459457361280, -189.7472609257535510, 78.77358243914956404 ) ) ;
#32027 = AXIS2_PLACEMENT_3D ( 'NONE', #13074, #9149, #20706 ) ;
#32026 = DIRECTION ( 'NONE',  ( 1.000000000000000000, 0.000000000000000000, 0.000000000000000000 ) ) ;
#32028 = CARTESIAN_POINT ( 'NONE',  ( 59.29945538372744807, -177.1207230881787780, 63.31490529818492519 ) ) ;
#32029 = DIRECTION ( 'NONE',  ( 0.000000000000000000, 0.000000000000000000, -1.000000000000000000 ) ) ;
#32030 = CARTESIAN_POINT ( 'NONE',  ( -336.3521761649654422, -110.9652333097088217, -57.67619951860654481 ) ) ;
#32031 = CARTESIAN_POINT ( 'NONE',  ( -336.3521761649654422, -141.9604555052315220, 56.09938080879057765 ) ) ;
#32032 = ORIENTED_EDGE ( 'NONE', *, *, #33560, .F. ) ;
#32033 = CARTESIAN_POINT ( 'NONE',  ( -139.8555433305420195, -175.3837268820161057, -83.82333043185244037 ) ) ;
#32034 = CARTESIAN_POINT ( 'NONE',  ( -48.93575598890257794, -183.6283474603465606, 0.8896570909947506545 ) ) ;
#32035 = EDGE_CURVE ( 'NONE', #26860, #41341, #20666, .T. ) ;
#32036 = CARTESIAN_POINT ( 'NONE',  ( -336.3521761649654422, -158.3591674452439122, -47.62880233550485087 ) ) ;
#32037 = ORIENTED_EDGE ( 'NONE', *, *, #29172, .F. ) ;
#32038 = FACE_OUTER_BOUND ( 'NONE', #3371, .T. ) ;
#32039 = VECTOR ( 'NONE', #36291, 1000.000000000000000 ) ;
#32040 = EDGE_CURVE ( 'NONE', #7438, #35703, #26096, .T. ) ;
#32041 = LINE ( 'NONE', #43623, #31119 ) ;
#32042 = CARTESIAN_POINT ( 'NONE',  ( -339.1964088526558498, -182.1300919119128423, 6.615309698015510165 ) ) ;
#32043 = EDGE_CURVE ( 'NONE', #41791, #51089, #25850, .T. ) ;
#32044 = ORIENTED_EDGE ( 'NONE', *, *, #9249, .T. ) ;
#32045 = EDGE_CURVE ( 'NONE', #34518, #1575, #24871, .T. ) ;
#32046 = EDGE_LOOP ( 'NONE', ( #20079, #34149, #47920, #50775 ) ) ;
#32047 = AXIS2_PLACEMENT_3D ( 'NONE', #17192, #36901, #16416 ) ;
#32048 = ORIENTED_EDGE ( 'NONE', *, *, #31771, .T. ) ;
#32049 = EDGE_CURVE ( 'NONE', #50010, #20455, #44845, .T. ) ;
#32050 = VECTOR ( 'NONE', #37570, 1000.000000000000000 ) ;
#32051 = PLANE ( 'NONE',  #43562 ) ;
#32052 = EDGE_CURVE ( 'NONE', #24430, #24544, #705, .T. ) ;
#32053 = CARTESIAN_POINT ( 'NONE',  ( -111.8989814360438828, -175.3837268820161057, -107.7168604805787027 ) ) ;
#32054 = CARTESIAN_POINT ( 'NONE',  ( 15.23368049493604381, -193.5000000000000000, -107.5438431188757420 ) ) ;
#32055 = CARTESIAN_POINT ( 'NONE',  ( -339.1964088526558498, -123.5000000000000284, 0.000000000000000000 ) ) ;
#32056 = ORIENTED_EDGE ( 'NONE', *, *, #17702, .T. ) ;
#32057 = EDGE_CURVE ( 'NONE', #34863, #1466, #30048, .T. ) ;
#32058 = CARTESIAN_POINT ( 'NONE',  ( 4.434257923028284587, 54.62691647646887816, -18.21285284460631360 ) ) ;
#32059 = AXIS2_PLACEMENT_3D ( 'NONE', #14240, #30258, #38398 ) ;
#32060 = ORIENTED_EDGE ( 'NONE', *, *, #4561, .F. ) ;
#32061 = EDGE_CURVE ( 'NONE', #9877, #40690, #13864, .T. ) ;
#32062 = VERTEX_POINT ( 'NONE', #42125 ) ;
#32063 = AXIS2_PLACEMENT_3D ( 'NONE', #3827, #15924, #11955 ) ;
#32064 = ORIENTED_EDGE ( 'NONE', *, *, #15285, .T. ) ;
#32065 = AXIS2_PLACEMENT_3D ( 'NONE', #14850, #30865, #10890 ) ;
#32066 = ADVANCED_FACE ( 'NONE', ( #10080 ), #6146, .T. ) ;
#32067 = VERTEX_POINT ( 'NONE', #26357 ) ;
#32068 = FACE_OUTER_BOUND ( 'NONE', #42230, .T. ) ;
#32069 = EDGE_CURVE ( 'NONE', #10459, #15796, #33169, .T. ) ;
#32070 = ORIENTED_EDGE ( 'NONE', *, *, #27779, .F. ) ;
#32071 = ADVANCED_FACE ( 'NONE', ( #2701 ), #38949, .T. ) ;
#32072 = ADVANCED_FACE ( 'NONE', ( #19266 ), #35021, .T. ) ;
#32073 = DIRECTION ( 'NONE',  ( -0.000000000000000000, 1.000000000000000000, -0.000000000000000000 ) ) ;
#32074 = CARTESIAN_POINT ( 'NONE',  ( -339.1964088526558498, -64.86990808808717190, -6.615309698015097162 ) ) ;
#32077 = ORIENTED_EDGE ( 'NONE', *, *, #13734, .T. ) ;
#32076 = LINE ( 'NONE', #28118, #48469 ) ;
#32075 = LINE ( 'NONE', #23434, #9865 ) ;
#32078 = CARTESIAN_POINT ( 'NONE',  ( -77.67449977936057337, -189.7472609257535510, -121.5427093402339267 ) ) ;
#32079 = ORIENTED_EDGE ( 'NONE', *, *, #15406, .F. ) ;
#32080 = FACE_OUTER_BOUND ( 'NONE', #25074, .T. ) ;
#32081 = AXIS2_PLACEMENT_3D ( 'NONE', #37787, #37539, #8895 ) ;
#32082 = ORIENTED_EDGE ( 'NONE', *, *, #28055, .T. ) ;
#32083 = DIRECTION ( 'NONE',  ( 0.000000000000000000, 0.000000000000000000, -1.000000000000000000 ) ) ;
#32084 = CARTESIAN_POINT ( 'NONE',  ( 63.39453919430265927, -189.7472609257535510, 53.48161459190912126 ) ) ;
#32086 = CARTESIAN_POINT ( 'NONE',  ( -305.0000000000000568, -97.97423230103774472, -54.29949524055093946 ) ) ;
#32085 = CARTESIAN_POINT ( 'NONE',  ( 14.43219681437621205, -189.7472609257535510, 106.8558168688117860 ) ) ;
#32087 = EDGE_CURVE ( 'NONE', #17378, #34311, #46603, .T. ) ;
#32088 = VERTEX_POINT ( 'NONE', #42652 ) ;
#32089 = CIRCLE ( 'NONE', #4374, 125.0000000000000000 ) ;
#32090 = DIRECTION ( 'NONE',  ( 0.000000000000000000, 0.000000000000000000, 1.000000000000000000 ) ) ;
#32091 = LINE ( 'NONE', #4509, #31219 ) ;
#32092 = ORIENTED_EDGE ( 'NONE', *, *, #19254, .T. ) ;
#32093 = DIRECTION ( 'NONE',  ( 0.000000000000000000, 0.000000000000000000, 1.000000000000000000 ) ) ;
#32094 = DIRECTION ( 'NONE',  ( 0.000000000000000000, 1.000000000000000000, 0.000000000000000000 ) ) ;
#32095 = ORIENTED_EDGE ( 'NONE', *, *, #10533, .T. ) ;
#32096 = FACE_OUTER_BOUND ( 'NONE', #14913, .T. ) ;
#32097 = AXIS2_PLACEMENT_3D ( 'NONE', #38128, #2131, #26307 ) ;
#32099 = AXIS2_PLACEMENT_3D ( 'NONE', #49570, #2500, #50597 ) ;
#32098 = PLANE ( 'NONE',  #45787 ) ;
#32100 = ORIENTED_EDGE ( 'NONE', *, *, #29434, .T. ) ;
#32101 = CARTESIAN_POINT ( 'NONE',  ( 47.04848625005566021, -177.1207230881787780, 80.61932246194658092 ) ) ;
#32102 = ORIENTED_EDGE ( 'NONE', *, *, #7696, .F. ) ;
#32103 = AXIS2_PLACEMENT_3D ( 'NONE', #37988, #50609, #9372 ) ;
#32104 = CIRCLE ( 'NONE', #51449, 125.0000000000000000 ) ;
#32105 = CARTESIAN_POINT ( 'NONE',  ( -48.47912675150885065, -189.7472609257535510, 6.938893903907228378E-15 ) ) ;
#32106 = DIRECTION ( 'NONE',  ( 0.000000000000000000, 1.000000000000000000, 0.000000000000000000 ) ) ;
#32107 = EDGE_CURVE ( 'NONE', #41052, #16634, #14807, .T. ) ;
#32108 = DIRECTION ( 'NONE',  ( 0.5586467658036535777, 0.000000000000000000, -0.8294056854502011022 ) ) ;
#32109 = DIRECTION ( 'NONE',  ( 0.000000000000000000, 0.000000000000000000, 1.000000000000000000 ) ) ;
#32110 = DIRECTION ( 'NONE',  ( 0.000000000000000000, 0.000000000000000000, 1.000000000000000000 ) ) ;
#32111 = EDGE_CURVE ( 'NONE', #16080, #43501, #449, .T. ) ;
#32112 = CLOSED_SHELL ( 'NONE', ( #11049, #30124, #48443, #51073, #50342, #24286, #367, #34330, #17970, #14982, #38636, #44572, #25900, #20871, #12093, #47851, #28390, #13426, #3821, #10467 ) ) ;
#32113 = EDGE_CURVE ( 'NONE', #19097, #14204, #22940, .T. ) ;
#32114 = CARTESIAN_POINT ( 'NONE',  ( -30.31202594373734271, -177.1207230881787780, -123.6727797384706093 ) ) ;
#32115 = EDGE_CURVE ( 'NONE', #21117, #7438, #43160, .T. ) ;
#32116 = CARTESIAN_POINT ( 'NONE',  ( 60.00000000000001421, -93.50000000000001421, -51.54700538379269403 ) ) ;
#32117 = CARTESIAN_POINT ( 'NONE',  ( 14.72514937628681508, -193.5000000000000000, -106.6827995071083848 ) ) ;
#32119 = VERTEX_POINT ( 'NONE', #14546 ) ;
#32118 = LINE ( 'NONE', #4531, #26168 ) ;
#32120 = VECTOR ( 'NONE', #17252, 999.9999999999998863 ) ;
#32121 = ORIENTED_EDGE ( 'NONE', *, *, #22048, .T. ) ;
#32122 = LINE ( 'NONE', #7455, #7299 ) ;
#32123 = AXIS2_PLACEMENT_3D ( 'NONE', #2408, #22636, #38648 ) ;
#32124 = FACE_OUTER_BOUND ( 'NONE', #50081, .T. ) ;
#32125 = ORIENTED_EDGE ( 'NONE', *, *, #45914, .F. ) ;
#32126 = ORIENTED_EDGE ( 'NONE', *, *, #6763, .T. ) ;
#32127 = EDGE_CURVE ( 'NONE', #2085, #10130, #22682, .T. ) ;
#32128 = ORIENTED_EDGE ( 'NONE', *, *, #51776, .F. ) ;
#32129 = CARTESIAN_POINT ( 'NONE',  ( -332.3517673607765914, -120.8677111499054320, 59.94223098458771659 ) ) ;
#32130 = DIRECTION ( 'NONE',  ( 0.000000000000000000, 0.2393156642875547968, -0.9709418174260527890 ) ) ;
#32131 = CARTESIAN_POINT ( 'NONE',  ( -165.1736796818183564, -183.6283474603465606, -41.93543928473609839 ) ) ;
#32132 = DIRECTION ( 'NONE',  ( 0.000000000000000000, -0.000000000000000000, -1.000000000000000000 ) ) ;
#32134 = ORIENTED_EDGE ( 'NONE', *, *, #20083, .T. ) ;
#32133 = VECTOR ( 'NONE', #6603, 1000.000000000000000 ) ;
#32135 = VECTOR ( 'NONE', #49072, 1000.000000000000000 ) ;
#32136 = VERTEX_POINT ( 'NONE', #38695 ) ;
#32137 = ADVANCED_FACE ( 'NONE', ( #18998 ), #7165, .T. ) ;
#32138 = VERTEX_POINT ( 'NONE', #3472 ) ;
#32139 = DIRECTION ( 'NONE',  ( -1.000000000000000000, 0.000000000000000000, -0.000000000000000000 ) ) ;
#32140 = CARTESIAN_POINT ( 'NONE',  ( -336.3521761649654422, -63.55776901541228341, -2.632288850093980503 ) ) ;
#32141 = DIRECTION ( 'NONE',  ( 1.000000000000000000, 0.000000000000000000, 0.000000000000000000 ) ) ;
#32142 = AXIS2_PLACEMENT_3D ( 'NONE', #21605, #41828, #25795 ) ;
#32143 = DIRECTION ( 'NONE',  ( 0.000000000000000000, 0.000000000000000000, 1.000000000000000000 ) ) ;
#32144 = CARTESIAN_POINT ( 'NONE',  ( 11.61413489515543418, -177.1207230881787780, -109.6074810615842381 ) ) ;
#32145 = ORIENTED_EDGE ( 'NONE', *, *, #5139, .T. ) ;
#32146 = LINE ( 'NONE', #35565, #17996 ) ;
#32147 = AXIS2_PLACEMENT_3D ( 'NONE', #36184, #185, #43816 ) ;
#32148 = DIRECTION ( 'NONE',  ( 0.9266896074318317078, 0.000000000000000000, 0.3758275821142421647 ) ) ;
#32149 = DIRECTION ( 'NONE',  ( 0.000000000000000000, 1.000000000000000000, 0.000000000000000000 ) ) ;
#32150 = CARTESIAN_POINT ( 'NONE',  ( -68.09401750944520870, -193.5000000000000000, -122.4396006697294581 ) ) ;
#32151 = EDGE_LOOP ( 'NONE', ( #47937, #31031, #395, #38367 ) ) ;
#32152 = ORIENTED_EDGE ( 'NONE', *, *, #43277, .T. ) ;
#32153 = VERTEX_POINT ( 'NONE', #51081 ) ;
#32154 = CARTESIAN_POINT ( 'NONE',  ( -150.1390659022305840, -175.3837268820161057, 72.73415134496005408 ) ) ;
#32155 = DIRECTION ( 'NONE',  ( -0.000000000000000000, 0.9927088740980544168, 0.1205366802553199113 ) ) ;
#32156 = ORIENTED_EDGE ( 'NONE', *, *, #35489, .F. ) ;
#32157 = PLANE ( 'NONE',  #25726 ) ;
#32158 = AXIS2_PLACEMENT_3D ( 'NONE', #7372, #35457, #31009 ) ;
#32159 = LINE ( 'NONE', #40034, #46379 ) ;
#32160 = CARTESIAN_POINT ( 'NONE',  ( -336.3521761649654422, -120.8677111499054320, 59.00000000000000000 ) ) ;
#32162 = ADVANCED_FACE ( 'NONE', ( #19503 ), #2960, .T. ) ;
#32161 = VERTEX_POINT ( 'NONE', #18481 ) ;
#32163 = CARTESIAN_POINT ( 'NONE',  ( -96.65280530915693191, -177.1207230881787780, -115.3442529744087466 ) ) ;
#32164 = AXIS2_PLACEMENT_3D ( 'NONE', #16110, #20293, #48693 ) ;
#32165 = VERTEX_POINT ( 'NONE', #27384 ) ;
#32166 = LINE ( 'NONE', #48212, #30742 ) ;
#32167 = EDGE_LOOP ( 'NONE', ( #9051, #43257, #40631, #7593 ) ) ;
#32168 = CARTESIAN_POINT ( 'NONE',  ( 10.22625775207003507, -177.1207230881787780, -109.2239789693433352 ) ) ;
#32169 = FACE_BOUND ( 'NONE', #10954, .T. ) ;
#32170 = DIRECTION ( 'NONE',  ( -0.08879589532293158394, 0.000000000000000000, -0.9960498426152172291 ) ) ;
#32171 = ORIENTED_EDGE ( 'NONE', *, *, #7066, .F. ) ;
#32172 = DIRECTION ( 'NONE',  ( 0.000000000000000000, 0.000000000000000000, 1.000000000000000000 ) ) ;
#32173 = DIRECTION ( 'NONE',  ( 0.000000000000000000, -0.000000000000000000, 1.000000000000000000 ) ) ;
#32174 = CARTESIAN_POINT ( 'NONE',  ( -332.3517673607765914, -92.15051119686104641, -50.05135858667769355 ) ) ;
#32175 = EDGE_CURVE ( 'NONE', #21817, #6661, #35274, .T. ) ;
#32176 = ADVANCED_FACE ( 'NONE', ( #51570 ), #26866, .F. ) ;
#32177 = AXIS2_PLACEMENT_3D ( 'NONE', #42094, #26323, #33942 ) ;
#32178 = PLANE ( 'NONE',  #48410 ) ;
#32179 = EDGE_LOOP ( 'NONE', ( #9421, #50313, #2992, #9060 ) ) ;
#32180 = DIRECTION ( 'NONE',  ( -0.000000000000000000, 1.000000000000000000, -0.000000000000000000 ) ) ;
#32181 = ORIENTED_EDGE ( 'NONE', *, *, #48138, .T. ) ;
#32182 = VERTEX_POINT ( 'NONE', #31588 ) ;
#32183 = CIRCLE ( 'NONE', #37209, 60.00000000000000000 ) ;
#32184 = CYLINDRICAL_SURFACE ( 'NONE', #26838, 125.0000000000000000 ) ;
#32186 = VERTEX_POINT ( 'NONE', #11627 ) ;
#32185 = CARTESIAN_POINT ( 'NONE',  ( -157.8637630444124795, -189.7472609257535510, -60.49794494914010556 ) ) ;
#32187 = EDGE_LOOP ( 'NONE', ( #18862, #19030, #46935, #3443 ) ) ;
#32188 = CARTESIAN_POINT ( 'NONE',  ( 1.663811650136611586, -189.7472609257535510, -113.4093733337827530 ) ) ;
#32189 = CARTESIAN_POINT ( 'NONE',  ( -336.3521761649654422, -87.81784868886214213, 47.06073758877343494 ) ) ;
#32190 = ORIENTED_EDGE ( 'NONE', *, *, #31059, .F. ) ;
#32191 = LINE ( 'NONE', #32965, #51655 ) ;
#32192 = CARTESIAN_POINT ( 'NONE',  ( 75.67769207106684348, -183.6283474603465606, 14.49428645563876827 ) ) ;
#32193 = EDGE_CURVE ( 'NONE', #25190, #26407, #11353, .T. ) ;
#32194 = ORIENTED_EDGE ( 'NONE', *, *, #24644, .F. ) ;
#32195 = CARTESIAN_POINT ( 'NONE',  ( -38.78589637709155369, -193.5000000000000000, -123.6213615703898654 ) ) ;
#32196 = DIRECTION ( 'NONE',  ( 0.000000000000000000, 0.000000000000000000, 1.000000000000000000 ) ) ;
#32197 = CIRCLE ( 'NONE', #46468, 125.0000000000000000 ) ;
#32198 = CARTESIAN_POINT ( 'NONE',  ( -339.1964088526558498, -63.50208336950359467, -0.5000000000000457412 ) ) ;
#32199 = PLANE ( 'NONE',  #24904 ) ;
#32200 = EDGE_LOOP ( 'NONE', ( #4280, #2028, #38919, #43477 ) ) ;
#32201 = ORIENTED_EDGE ( 'NONE', *, *, #13979, .F. ) ;
#32202 = AXIS2_PLACEMENT_3D ( 'NONE', #21344, #33161, #9265 ) ;
#32203 = EDGE_CURVE ( 'NONE', #35744, #45569, #43681, .T. ) ;
#32204 = VERTEX_POINT ( 'NONE', #2454 ) ;
#32205 = DIRECTION ( 'NONE',  ( -0.9027978299657477557, 0.000000000000000000, 0.4300652022765115712 ) ) ;
#32206 = CARTESIAN_POINT ( 'NONE',  ( -48.47912675150885065, -117.5479369270332057, 15.00000000000000711 ) ) ;
#32207 = DIRECTION ( 'NONE',  ( -0.000000000000000000, 0.000000000000000000, -1.000000000000000000 ) ) ;
#32208 = FACE_BOUND ( 'NONE', #51936, .T. ) ;
#32209 = CARTESIAN_POINT ( 'NONE',  ( -330.4913330509368166, -131.1080185721132807, -58.50955523165751515 ) ) ;
#32210 = ORIENTED_EDGE ( 'NONE', *, *, #31344, .F. ) ;
#32211 = EDGE_CURVE ( 'NONE', #24136, #38799, #39977, .T. ) ;
#32212 = VECTOR ( 'NONE', #36994, 1000.000000000000114 ) ;
#32213 = ORIENTED_EDGE ( 'NONE', *, *, #21031, .T. ) ;
#32215 = ORIENTED_EDGE ( 'NONE', *, *, #51902, .F. ) ;
#32214 = PLANE ( 'NONE',  #33178 ) ;
#32216 = ORIENTED_EDGE ( 'NONE', *, *, #21443, .F. ) ;
#32217 = DIRECTION ( 'NONE',  ( -0.000000000000000000, 1.000000000000000000, -0.000000000000000000 ) ) ;
#32218 = PLANE ( 'NONE',  #30004 ) ;
#32219 = CARTESIAN_POINT ( 'NONE',  ( -123.4791267515088435, -198.5000000000000000, 70.00000000000000000 ) ) ;
#32220 = LINE ( 'NONE', #48264, #9987 ) ;
#32221 = VERTEX_POINT ( 'NONE', #36840 ) ;
#32222 = CARTESIAN_POINT ( 'NONE',  ( 27.42205759510524032, -189.7472609257535510, 98.05618656931997634 ) ) ;
#32223 = ORIENTED_EDGE ( 'NONE', *, *, #11829, .T. ) ;
#32224 = EDGE_CURVE ( 'NONE', #46894, #11150, #43258, .T. ) ;
#32225 = ORIENTED_EDGE ( 'NONE', *, *, #4135, .F. ) ;
#32226 = PLANE ( 'NONE',  #47263 ) ;
#32227 = DIRECTION ( 'NONE',  ( 0.000000000000000000, -0.000000000000000000, -1.000000000000000000 ) ) ;
#32228 = AXIS2_PLACEMENT_3D ( 'NONE', #25555, #46076, #10060 ) ;
#32229 = DIRECTION ( 'NONE',  ( -0.000000000000000000, 1.000000000000000000, 0.000000000000000000 ) ) ;
#32230 = AXIS2_PLACEMENT_3D ( 'NONE', #19955, #47308, #47568 ) ;
#32231 = DIRECTION ( 'NONE',  ( 0.000000000000000000, 0.000000000000000000, 1.000000000000000000 ) ) ;
#32232 = CARTESIAN_POINT ( 'NONE',  ( 73.79319191488886531, -193.5000000000000000, 20.63201007055492653 ) ) ;
#32233 = EDGE_CURVE ( 'NONE', #28874, #8885, #831, .T. ) ;
#32234 = VERTEX_POINT ( 'NONE', #39714 ) ;
#32235 = DIRECTION ( 'NONE',  ( -0.000000000000000000, 1.000000000000000000, -0.000000000000000000 ) ) ;
#32236 = CARTESIAN_POINT ( 'NONE',  ( -336.3521761649654422, -148.5878911270064009, 53.46519113769075204 ) ) ;
#32237 = CIRCLE ( 'NONE', #38945, 125.0000000000000000 ) ;
#32238 = FACE_BOUND ( 'NONE', #41888, .T. ) ;
#32239 = ORIENTED_EDGE ( 'NONE', *, *, #22996, .F. ) ;
#32240 = EDGE_CURVE ( 'NONE', #29294, #24657, #28671, .T. ) ;
#32241 = DIRECTION ( 'NONE',  ( -0.000000000000000000, 1.000000000000000000, -0.000000000000000000 ) ) ;
#32242 = DIRECTION ( 'NONE',  ( -1.000000000000000000, 0.000000000000000000, 0.000000000000000000 ) ) ;
#32243 = ORIENTED_EDGE ( 'NONE', *, *, #43430, .T. ) ;
#32244 = PLANE ( 'NONE',  #27117 ) ;
#32245 = AXIS2_PLACEMENT_3D ( 'NONE', #18518, #34532, #13802 ) ;
#32246 = ORIENTED_EDGE ( 'NONE', *, *, #34160, .F. ) ;
#32247 = CARTESIAN_POINT ( 'NONE',  ( 1.150725574412418739, -193.5000000000000000, -114.7252272087845881 ) ) ;
#32248 = CARTESIAN_POINT ( 'NONE',  ( -330.4913330509368166, -124.0000000000001990, -59.00000000000002132 ) ) ;
#32250 = ORIENTED_EDGE ( 'NONE', *, *, #17667, .T. ) ;
#32249 = CARTESIAN_POINT ( 'NONE',  ( -336.3521761649653854, -180.1590281025188460, -19.74220186498920881 ) ) ;
#32251 = ADVANCED_FACE ( 'NONE', ( #19756 ), #11867, .T. ) ;
#32252 = FACE_OUTER_BOUND ( 'NONE', #20893, .T. ) ;
#32253 = ORIENTED_EDGE ( 'NONE', *, *, #19711, .T. ) ;
#32254 = EDGE_LOOP ( 'NONE', ( #43657, #2098 ) ) ;
#32255 = CARTESIAN_POINT ( 'NONE',  ( -336.3521761649653854, -67.99860710409808462, -22.79463504017392950 ) ) ;
#32256 = EDGE_LOOP ( 'NONE', ( #37921, #7992, #16869, #17093 ) ) ;
#32257 = FACE_OUTER_BOUND ( 'NONE', #20099, .T. ) ;
#32258 = VECTOR ( 'NONE', #35245, 1000.000000000000000 ) ;
#32259 = DIRECTION ( 'NONE',  ( -0.000000000000000000, 1.000000000000000000, -0.000000000000000000 ) ) ;
#32260 = AXIS2_PLACEMENT_3D ( 'NONE', #17330, #48868, #33349 ) ;
#32261 = AXIS2_PLACEMENT_3D ( 'NONE', #6152, #42390, #42904 ) ;
#32262 = DIRECTION ( 'NONE',  ( 0.000000000000000000, -0.000000000000000000, -1.000000000000000000 ) ) ;
#32263 = DIRECTION ( 'NONE',  ( -0.000000000000000000, 1.000000000000000000, -0.000000000000000000 ) ) ;
#32264 = VERTEX_POINT ( 'NONE', #35789 ) ;
#32266 = ORIENTED_EDGE ( 'NONE', *, *, #19428, .F. ) ;
#32265 = CARTESIAN_POINT ( 'NONE',  ( 14.94072793302542124, -175.3837268820161057, 107.7168604805791574 ) ) ;
#32267 = EDGE_LOOP ( 'NONE', ( #48494, #23701, #30426, #52002 ) ) ;
#32268 = CARTESIAN_POINT ( 'NONE',  ( -339.1964088526558498, -178.8432607619609485, -20.45418021416653076 ) ) ;
#32269 = ORIENTED_EDGE ( 'NONE', *, *, #24677, .F. ) ;
#32270 = DIRECTION ( 'NONE',  ( 0.000000000000000000, 0.000000000000000000, 1.000000000000000000 ) ) ;
#32271 = ORIENTED_EDGE ( 'NONE', *, *, #3657, .T. ) ;
#32272 = EDGE_CURVE ( 'NONE', #5202, #32545, #302, .T. ) ;
#32273 = EDGE_CURVE ( 'NONE', #28202, #28554, #44201, .T. ) ;
#32274 = CARTESIAN_POINT ( 'NONE',  ( -63.31390705753092618, -193.5000000000000000, 123.1094209424469312 ) ) ;
#32275 = ORIENTED_EDGE ( 'NONE', *, *, #17495, .F. ) ;
#32277 = PLANE ( 'NONE',  #40060 ) ;
#32276 = DIRECTION ( 'NONE',  ( 1.000000000000000000, -0.000000000000000000, -0.000000000000000000 ) ) ;
#32278 = AXIS2_PLACEMENT_3D ( 'NONE', #45544, #12431, #40798 ) ;
#32279 = ORIENTED_EDGE ( 'NONE', *, *, #10826, .F. ) ;
#32280 = ORIENTED_EDGE ( 'NONE', *, *, #51596, .T. ) ;
#32281 = CARTESIAN_POINT ( 'NONE',  ( -336.3521761649654422, -67.40061919120938683, 18.46045550523129819 ) ) ;
#32282 = PLANE ( 'NONE',  #4706 ) ;
#32283 = LINE ( 'NONE', #15780, #46543 ) ;
#32284 = CARTESIAN_POINT ( 'NONE',  ( 0.000000000000000000, -182.0698235717852924, -7.111664135063673342 ) ) ;
#32285 = PLANE ( 'NONE',  #38321 ) ;
#32286 = CARTESIAN_POINT ( 'NONE',  ( 30.50828161901817381, -183.6283474603465606, 96.88131563365350019 ) ) ;
#32287 = EDGE_LOOP ( 'NONE', ( #860, #18208, #429, #2568 ) ) ;
#32288 = EDGE_CURVE ( 'NONE', #1472, #32182, #10551, .T. ) ;
#32289 = FACE_OUTER_BOUND ( 'NONE', #21039, .T. ) ;
#32290 = DIRECTION ( 'NONE',  ( 0.5586467658036594619, 0.000000000000000000, -0.8294056854501971054 ) ) ;
#32291 = EDGE_CURVE ( 'NONE', #9248, #16704, #23707, .T. ) ;
#32292 = CARTESIAN_POINT ( 'NONE',  ( -137.2624501260119985, -177.1207230881787780, 87.99159897727967916 ) ) ;
#32293 = VERTEX_POINT ( 'NONE', #44724 ) ;
#32294 = EDGE_CURVE ( 'NONE', #346, #24932, #24479, .T. ) ;
#32295 = VECTOR ( 'NONE', #24538, 1000.000000000000114 ) ;
#32296 = DIRECTION ( 'NONE',  ( 0.1182731709213592358, 0.000000000000000000, 0.9929810960135178055 ) ) ;
#32297 = VECTOR ( 'NONE', #40943, 1000.000000000000000 ) ;
#32298 = VECTOR ( 'NONE', #41993, 1000.000000000000227 ) ;
#32299 = CARTESIAN_POINT ( 'NONE',  ( -49.32472275501068282, -193.5000000000000000, 0.5338233779647895139 ) ) ;
#32300 = CARTESIAN_POINT ( 'NONE',  ( 16.59365244519688787, -193.5000000000000000, -105.5544085257710947 ) ) ;
#32301 = VERTEX_POINT ( 'NONE', #7928 ) ;
#32302 = EDGE_LOOP ( 'NONE', ( #48949, #32934, #12600, #48500 ) ) ;
#32303 = VERTEX_POINT ( 'NONE', #48676 ) ;
#32304 = VECTOR ( 'NONE', #35407, 1000.000000000000114 ) ;
#32305 = FACE_OUTER_BOUND ( 'NONE', #10389, .T. ) ;
#32306 = LINE ( 'NONE', #1295, #19484 ) ;
#32307 = AXIS2_PLACEMENT_3D ( 'NONE', #47544, #7077, #15223 ) ;
#32308 = CARTESIAN_POINT ( 'NONE',  ( -48.24424070572786860, -183.6283474603465606, -0.9720229140804037549 ) ) ;
#32309 = FACE_OUTER_BOUND ( 'NONE', #2982, .T. ) ;
#32310 = AXIS2_PLACEMENT_3D ( 'NONE', #9331, #17737, #25352 ) ;
#32311 = VERTEX_POINT ( 'NONE', #20027 ) ;
#32312 = AXIS2_PLACEMENT_3D ( 'NONE', #37596, #33892, #49680 ) ;
#32313 = FACE_OUTER_BOUND ( 'NONE', #47001, .T. ) ;
#32314 = VERTEX_POINT ( 'NONE', #16094 ) ;
#32315 = AXIS2_PLACEMENT_3D ( 'NONE', #8367, #32008, #16001 ) ;
#32316 = EDGE_LOOP ( 'NONE', ( #47409, #7291, #31666, #43561 ) ) ;
#32317 = LINE ( 'NONE', #7402, #38463 ) ;
#32318 = ORIENTED_EDGE ( 'NONE', *, *, #50057, .F. ) ;
#32319 = DIRECTION ( 'NONE',  ( -0.000000000000000000, 1.000000000000000000, -0.000000000000000000 ) ) ;
#32320 = DIRECTION ( 'NONE',  ( 1.000000000000000000, -0.000000000000000000, -0.000000000000000000 ) ) ;
#32323 = ORIENTED_EDGE ( 'NONE', *, *, #40430, .T. ) ;
#32322 = DIRECTION ( 'NONE',  ( 0.000000000000000000, 0.1205366802553338029, 0.9927088740980527515 ) ) ;
#32321 = DIRECTION ( 'NONE',  ( -1.000000000000000000, 0.000000000000000000, 0.000000000000000000 ) ) ;
#32324 = VECTOR ( 'NONE', #35268, 1000.000000000000000 ) ;
#32325 = CARTESIAN_POINT ( 'NONE',  ( -161.2555905272864436, -193.5000000000000000, -53.91167979418489864 ) ) ;
#32326 = VECTOR ( 'NONE', #5878, 999.9999999999998863 ) ;
#32327 = ORIENTED_EDGE ( 'NONE', *, *, #42310, .T. ) ;
#32328 = LINE ( 'NONE', #24211, #18839 ) ;
#32329 = ORIENTED_EDGE ( 'NONE', *, *, #5919, .F. ) ;
#32330 = CIRCLE ( 'NONE', #8044, 125.0000000000000000 ) ;
#32331 = EDGE_CURVE ( 'NONE', #6669, #20596, #14732, .T. ) ;
#32332 = EDGE_CURVE ( 'NONE', #30086, #8637, #1325, .T. ) ;
#32333 = EDGE_CURVE ( 'NONE', #9325, #8246, #20536, .T. ) ;
#32334 = PLANE ( 'NONE',  #17458 ) ;
#32335 = CARTESIAN_POINT ( 'NONE',  ( 0.000000000000000000, -63.50000000000000000, 0.000000000000000000 ) ) ;
#32337 = LINE ( 'NONE', #12630, #46661 ) ;
#32336 = LINE ( 'NONE', #16074, #51781 ) ;
#32338 = VERTEX_POINT ( 'NONE', #12909 ) ;
#32339 = EDGE_CURVE ( 'NONE', #51600, #48065, #46654, .T. ) ;
#32340 = CARTESIAN_POINT ( 'NONE',  ( -336.3521761649654422, -123.5000000000000284, 0.000000000000000000 ) ) ;
#32341 = DIRECTION ( 'NONE',  ( 0.000000000000000000, -1.000000000000000000, -0.000000000000000000 ) ) ;
#32342 = DIRECTION ( 'NONE',  ( 0.000000000000000000, -0.4647231720437725033, -0.8854560256532079121 ) ) ;
#32343 = ORIENTED_EDGE ( 'NONE', *, *, #3173, .T. ) ;
#32344 = EDGE_CURVE ( 'NONE', #8272, #2850, #32330, .T. ) ;
#32345 = VECTOR ( 'NONE', #13085, 1000.000000000000000 ) ;
#32346 = DIRECTION ( 'NONE',  ( 1.000000000000000000, -0.000000000000000000, -0.000000000000000000 ) ) ;
#32347 = DIRECTION ( 'NONE',  ( -0.000000000000000000, 0.000000000000000000, -1.000000000000000000 ) ) ;
#32348 = EDGE_CURVE ( 'NONE', #5759, #50025, #51685, .T. ) ;
#32349 = VECTOR ( 'NONE', #40991, 1000.000000000000000 ) ;
#32350 = CARTESIAN_POINT ( 'NONE',  ( -48.47912675150885065, -189.7472609257535510, 6.938893903907228378E-15 ) ) ;
#32351 = EDGE_LOOP ( 'NONE', ( #43665, #51179, #6407, #45826 ) ) ;
#32352 = CARTESIAN_POINT ( 'NONE',  ( -171.4559849729830603, -183.6283474603465606, 22.39848972532371718 ) ) ;
#32353 = EDGE_CURVE ( 'NONE', #11613, #18519, #36567, .T. ) ;
#32354 = AXIS2_PLACEMENT_3D ( 'NONE', #47880, #7661, #23685 ) ;
#32355 = CARTESIAN_POINT ( 'NONE',  ( -172.5669052183642123, -177.1207230881787780, 15.07392567185553567 ) ) ;
#32356 = EDGE_CURVE ( 'NONE', #32186, #3877, #9699, .T. ) ;
#32357 = AXIS2_PLACEMENT_3D ( 'NONE', #12436, #3273, #4296 ) ;
#32358 = EDGE_CURVE ( 'NONE', #16769, #49622, #6083, .T. ) ;
#32359 = VERTEX_POINT ( 'NONE', #21064 ) ;
#32360 = CARTESIAN_POINT ( 'NONE',  ( -33.52607327456453135, -189.7472609257535510, -124.1024020384603119 ) ) ;
#32361 = EDGE_LOOP ( 'NONE', ( #50270, #49278 ) ) ;
#32362 = EDGE_CURVE ( 'NONE', #48442, #49029, #49195, .T. ) ;
#32363 = CARTESIAN_POINT ( 'NONE',  ( -48.47912675150885065, -189.7472609257535510, 6.938893903907228378E-15 ) ) ;
#32364 = DIRECTION ( 'NONE',  ( -0.000000000000000000, 1.000000000000000000, -0.000000000000000000 ) ) ;
#32365 = EDGE_CURVE ( 'NONE', #48376, #47640, #37085, .T. ) ;
#32366 = DIRECTION ( 'NONE',  ( 1.000000000000000000, -0.000000000000000000, 0.000000000000000000 ) ) ;
#32367 = LINE ( 'NONE', #27906, #44200 ) ;
#32368 = DIRECTION ( 'NONE',  ( 0.000000000000000000, 0.000000000000000000, -1.000000000000000000 ) ) ;
#32369 = AXIS2_PLACEMENT_3D ( 'NONE', #49645, #16556, #1020 ) ;
#32370 = CARTESIAN_POINT ( 'NONE',  ( -172.4792251663439231, -193.5000000000000000, 0.3215015308249614123 ) ) ;
#32371 = DIRECTION ( 'NONE',  ( -0.000000000000000000, -0.7485107481710953081, 0.6631226582408016323 ) ) ;
#32373 = ORIENTED_EDGE ( 'NONE', *, *, #21504, .T. ) ;
#32372 = LINE ( 'NONE', #28163, #13577 ) ;
#32374 = VECTOR ( 'NONE', #14217, 1000.000000000000341 ) ;
#32375 = AXIS2_PLACEMENT_3D ( 'NONE', #28089, #44135, #40192 ) ;
#32376 = VERTEX_POINT ( 'NONE', #9762 ) ;
#32377 = DIRECTION ( 'NONE',  ( 0.000000000000000000, 0.5680647467311569221, 0.8229838658936556861 ) ) ;
#32378 = EDGE_CURVE ( 'NONE', #16147, #13737, #13963, .T. ) ;
#32379 = DIRECTION ( 'NONE',  ( -0.000000000000000000, -0.3546048870425396182, -0.9350162426854132791 ) ) ;
#32380 = ORIENTED_EDGE ( 'NONE', *, *, #19369, .F. ) ;
#32381 = VERTEX_POINT ( 'NONE', #41542 ) ;
#32382 = CIRCLE ( 'NONE', #13951, 60.00000000000000000 ) ;
#32383 = VERTEX_POINT ( 'NONE', #5050 ) ;
#32384 = VECTOR ( 'NONE', #20340, 1000.000000000000000 ) ;
#32386 = CIRCLE ( 'NONE', #37467, 125.0000000000000000 ) ;
#32385 = DIRECTION ( 'NONE',  ( 0.000000000000000000, 0.000000000000000000, 1.000000000000000000 ) ) ;
#32387 = DIRECTION ( 'NONE',  ( 0.000000000000000000, 0.000000000000000000, 1.000000000000000000 ) ) ;
#32388 = VERTEX_POINT ( 'NONE', #1625 ) ;
#32389 = EDGE_LOOP ( 'NONE', ( #8937, #32926, #23319, #40376 ) ) ;
#32390 = VERTEX_POINT ( 'NONE', #9503 ) ;
#32391 = AXIS2_PLACEMENT_3D ( 'NONE', #6187, #23250, #22982 ) ;
#32392 = EDGE_CURVE ( 'NONE', #8865, #1307, #25271, .T. ) ;
#32393 = DIRECTION ( 'NONE',  ( -1.000000000000000000, 5.399917434947259359E-17, 0.000000000000000000 ) ) ;
#32394 = LINE ( 'NONE', #16902, #4225 ) ;
#32396 = ORIENTED_EDGE ( 'NONE', *, *, #3033, .F. ) ;
#32395 = DIRECTION ( 'NONE',  ( 0.000000000000000000, -0.000000000000000000, -1.000000000000000000 ) ) ;
#32397 = FACE_OUTER_BOUND ( 'NONE', #9696, .T. ) ;
#32398 = LINE ( 'NONE', #4552, #18858 ) ;
#32399 = ORIENTED_EDGE ( 'NONE', *, *, #25597, .F. ) ;
#32400 = DIRECTION ( 'NONE',  ( 0.000000000000000000, -0.9709418174260544543, -0.2393156642875482465 ) ) ;
#32401 = EDGE_CURVE ( 'NONE', #44533, #22822, #25521, .T. ) ;
#32402 = EDGE_CURVE ( 'NONE', #22956, #19332, #41822, .T. ) ;
#32403 = EDGE_CURVE ( 'NONE', #12964, #42609, #21327, .T. ) ;
#32404 = FACE_OUTER_BOUND ( 'NONE', #25948, .T. ) ;
#32405 = DIRECTION ( 'NONE',  ( -0.000000000000000000, 0.000000000000000000, -1.000000000000000000 ) ) ;
#32406 = DIRECTION ( 'NONE',  ( -0.000000000000000000, 1.000000000000000000, -0.000000000000000000 ) ) ;
#32407 = ADVANCED_FACE ( 'NONE', ( #1085 ), #2120, .T. ) ;
#32408 = ORIENTED_EDGE ( 'NONE', *, *, #18127, .F. ) ;
#32409 = ORIENTED_EDGE ( 'NONE', *, *, #17666, .T. ) ;
#32410 = CIRCLE ( 'NONE', #39119, 20.00000000000001776 ) ;
#32411 = ORIENTED_EDGE ( 'NONE', *, *, #34906, .T. ) ;
#32412 = CARTESIAN_POINT ( 'NONE',  ( -339.1964088526558498, -172.3400804610915600, -33.10432812419107051 ) ) ;
#32413 = CIRCLE ( 'NONE', #18173, 125.0000000000000000 ) ;
#32414 = DIRECTION ( 'NONE',  ( -0.3482016354344059095, 0.000000000000000000, 0.9374196611341183427 ) ) ;
#32415 = VERTEX_POINT ( 'NONE', #1867 ) ;
#32416 = EDGE_CURVE ( 'NONE', #51152, #15690, #17911, .T. ) ;
#32417 = DIRECTION ( 'NONE',  ( -8.718379230999705894E-17, -0.3546048870425235200, 0.9350162426854194964 ) ) ;
#32418 = CIRCLE ( 'NONE', #45869, 125.0000000000000000 ) ;
#32419 = FACE_OUTER_BOUND ( 'NONE', #30223, .T. ) ;
#32420 = EDGE_LOOP ( 'NONE', ( #29561, #50985, #1112, #39872 ) ) ;
#32421 = DIRECTION ( 'NONE',  ( -0.000000000000000000, -1.000000000000000000, -0.000000000000000000 ) ) ;
#32422 = EDGE_CURVE ( 'NONE', #20596, #46251, #1350, .T. ) ;
#32423 = DIRECTION ( 'NONE',  ( 0.000000000000000000, -0.7485107481711069655, -0.6631226582407885317 ) ) ;
#32424 = ORIENTED_EDGE ( 'NONE', *, *, #9720, .F. ) ;
#32425 = CARTESIAN_POINT ( 'NONE',  ( 58.48829670243886625, -183.6283474603465606, -64.67588669375805921 ) ) ;
#32426 = ORIENTED_EDGE ( 'NONE', *, *, #18064, .F. ) ;
#32427 = FACE_BOUND ( 'NONE', #6244, .T. ) ;
#32428 = AXIS2_PLACEMENT_3D ( 'NONE', #51134, #31126, #29257 ) ;
#32429 = EDGE_CURVE ( 'NONE', #51235, #35050, #48296, .T. ) ;
#32430 = AXIS2_PLACEMENT_3D ( 'NONE', #20268, #7915, #28142 ) ;
#32431 = CARTESIAN_POINT ( 'NONE',  ( -336.3521761649654422, -110.9652333097088217, -57.67619951860654481 ) ) ;
#32432 = ORIENTED_EDGE ( 'NONE', *, *, #28624, .F. ) ;
#32433 = VECTOR ( 'NONE', #48457, 1000.000000000000227 ) ;
#32434 = AXIS2_PLACEMENT_3D ( 'NONE', #103, #2326, #18851 ) ;
#32435 = EDGE_CURVE ( 'NONE', #31403, #36384, #38117, .T. ) ;
#32436 = CYLINDRICAL_SURFACE ( 'NONE', #21486, 10.00000000000000000 ) ;
#32437 = DIRECTION ( 'NONE',  ( 1.000000000000000000, 0.000000000000000000, 0.000000000000000000 ) ) ;
#32438 = CARTESIAN_POINT ( 'NONE',  ( -117.6201219941651601, -189.7472609257535510, 104.1370384486469760 ) ) ;
#32439 = AXIS2_PLACEMENT_3D ( 'NONE', #12998, #12489, #40856 ) ;
#32440 = PLANE ( 'NONE',  #26601 ) ;
#32441 = EDGE_CURVE ( 'NONE', #10598, #12446, #29459, .T. ) ;
#32442 = ORIENTED_EDGE ( 'NONE', *, *, #842, .T. ) ;
#32444 = AXIS2_PLACEMENT_3D ( 'NONE', #42364, #27366, #34733 ) ;
#32443 = LINE ( 'NONE', #45331, #987 ) ;
#32445 = VERTEX_POINT ( 'NONE', #8983 ) ;
#32446 = EDGE_LOOP ( 'NONE', ( #44538, #51865, #30120, #34368 ) ) ;
#32447 = CIRCLE ( 'NONE', #12289, 4.000000000000003553 ) ;
#32448 = CARTESIAN_POINT ( 'NONE',  ( -336.3521761649654422, -111.9361751271348879, -57.91551518289410438 ) ) ;
#32450 = ORIENTED_EDGE ( 'NONE', *, *, #51252, .T. ) ;
#32449 = LINE ( 'NONE', #48499, #12817 ) ;
#32451 = VERTEX_POINT ( 'NONE', #29717 ) ;
#32452 = CARTESIAN_POINT ( 'NONE',  ( 18.49541618049842384, -177.1207230881787780, 105.5434062319798159 ) ) ;
#32453 = EDGE_CURVE ( 'NONE', #15240, #22737, #22105, .T. ) ;
#32454 = LINE ( 'NONE', #4092, #16762 ) ;
#32455 = VECTOR ( 'NONE', #48220, 1000.000000000000000 ) ;
#32456 = AXIS2_PLACEMENT_3D ( 'NONE', #35527, #7171, #30557 ) ;
#32457 = ORIENTED_EDGE ( 'NONE', *, *, #27192, .T. ) ;
#32458 = DIRECTION ( 'NONE',  ( 0.000000000000000000, -1.000000000000000000, 0.000000000000000000 ) ) ;
#32459 = ORIENTED_EDGE ( 'NONE', *, *, #4182, .F. ) ;
#32460 = LINE ( 'NONE', #11706, #45135 ) ;
#32461 = PLANE ( 'NONE',  #28323 ) ;
#32462 = VECTOR ( 'NONE', #19874, 1000.000000000000114 ) ;
#32463 = CARTESIAN_POINT ( 'NONE',  ( 0.000000000000000000, -74.94395191227431496, -33.51582005713827783 ) ) ;
#32464 = DIRECTION ( 'NONE',  ( 0.000000000000000000, 0.000000000000000000, 1.000000000000000000 ) ) ;
#32465 = ORIENTED_EDGE ( 'NONE', *, *, #44164, .F. ) ;
#32466 = EDGE_LOOP ( 'NONE', ( #14199, #42702, #10424, #18595 ) ) ;
#32467 = ORIENTED_EDGE ( 'NONE', *, *, #41249, .T. ) ;
#32468 = LINE ( 'NONE', #23805, #39986 ) ;
#32469 = FACE_BOUND ( 'NONE', #20054, .T. ) ;
#32470 = AXIS2_PLACEMENT_3D ( 'NONE', #9341, #29028, #24840 ) ;
#32471 = VECTOR ( 'NONE', #34937, 1000.000000000000000 ) ;
#32472 = LINE ( 'NONE', #25120, #1635 ) ;
#32473 = VECTOR ( 'NONE', #31306, 1000.000000000000000 ) ;
#32475 = CIRCLE ( 'NONE', #39184, 125.0000000000000000 ) ;
#32474 = FACE_BOUND ( 'NONE', #22282, .T. ) ;
#32476 = CARTESIAN_POINT ( 'NONE',  ( -332.3517673607765914, -149.4733471526596134, 53.00046796564699036 ) ) ;
#32477 = ORIENTED_EDGE ( 'NONE', *, *, #16714, .F. ) ;
#32478 = EDGE_CURVE ( 'NONE', #20725, #22344, #29990, .T. ) ;
#32479 = VECTOR ( 'NONE', #15344, 1000.000000000000114 ) ;
#32480 = CIRCLE ( 'NONE', #41709, 60.00000000000000000 ) ;
#32481 = ORIENTED_EDGE ( 'NONE', *, *, #40396, .T. ) ;
#32483 = VERTEX_POINT ( 'NONE', #42069 ) ;
#32482 = CARTESIAN_POINT ( 'NONE',  ( 7.859956736328458149, -193.5000000000000000, -111.5836353223468649 ) ) ;
#32484 = ORIENTED_EDGE ( 'NONE', *, *, #4942, .F. ) ;
#32485 = FACE_OUTER_BOUND ( 'NONE', #22213, .T. ) ;
#32486 = CARTESIAN_POINT ( 'NONE',  ( -260.0000000000000000, -153.5000000000000284, -59.99999999999999289 ) ) ;
#32487 = CARTESIAN_POINT ( 'NONE',  ( -169.6719064342497632, -183.6283474603465606, 30.61552143554992256 ) ) ;
#32488 = DIRECTION ( 'NONE',  ( 0.000000000000000000, 0.000000000000000000, 1.000000000000000000 ) ) ;
#32489 = ORIENTED_EDGE ( 'NONE', *, *, #3906, .F. ) ;
#32490 = CARTESIAN_POINT ( 'NONE',  ( -48.47912675150885065, -177.1207230881787780, 6.938893903907228378E-15 ) ) ;
#32491 = VERTEX_POINT ( 'NONE', #34191 ) ;
#32492 = ORIENTED_EDGE ( 'NONE', *, *, #20337, .T. ) ;
#32493 = CARTESIAN_POINT ( 'NONE',  ( -48.47912675150885065, -175.3837268820161057, 6.938893903907228378E-15 ) ) ;
#32494 = VECTOR ( 'NONE', #32217, 1000.000000000000000 ) ;
#32495 = EDGE_CURVE ( 'NONE', #12363, #42035, #50240, .T. ) ;
#32496 = DIRECTION ( 'NONE',  ( 1.000000000000000000, -0.000000000000000000, 0.000000000000000000 ) ) ;
#32497 = CARTESIAN_POINT ( 'NONE',  ( -47.51449116960048968, -183.6283474603465606, -0.2635871660690578544 ) ) ;
#32498 = DIRECTION ( 'NONE',  ( -0.000000000000000000, 1.000000000000000000, -0.000000000000000000 ) ) ;
#32499 = CIRCLE ( 'NONE', #9026, 60.00000000000000000 ) ;
#32500 = CARTESIAN_POINT ( 'NONE',  ( -55.71438232577004612, -189.7472609257535510, -124.7904286264580662 ) ) ;
#32501 = CARTESIAN_POINT ( 'NONE',  ( -85.14888725715768203, -193.5000000000000000, 119.5003291395398577 ) ) ;
#32502 = ORIENTED_EDGE ( 'NONE', *, *, #41, .T. ) ;
#32503 = DIRECTION ( 'NONE',  ( -0.000000000000000000, 0.7485107481710999711, -0.6631226582407964143 ) ) ;
#32504 = DIRECTION ( 'NONE',  ( -0.1182731709213592358, 0.000000000000000000, -0.9929810960135178055 ) ) ;
#32505 = ADVANCED_FACE ( 'NONE', ( #26292 ), #38640, .T. ) ;
#32506 = LINE ( 'NONE', #35463, #38684 ) ;
#32507 = FACE_BOUND ( 'NONE', #10094, .T. ) ;
#32508 = VERTEX_POINT ( 'NONE', #50490 ) ;
#32509 = AXIS2_PLACEMENT_3D ( 'NONE', #6997, #2536, #46956 ) ;
#32510 = AXIS2_PLACEMENT_3D ( 'NONE', #41574, #50519, #38145 ) ;
#32511 = CARTESIAN_POINT ( 'NONE',  ( -330.4913330509368166, -137.3729703655831997, 58.37414404713486249 ) ) ;
#32512 = VECTOR ( 'NONE', #36690, 1000.000000000000000 ) ;
#32513 = FACE_OUTER_BOUND ( 'NONE', #4919, .T. ) ;
#32514 = VERTEX_POINT ( 'NONE', #47060 ) ;
#32515 = CARTESIAN_POINT ( 'NONE',  ( -48.47912675150885065, -175.3837268820161057, 6.938893903907228378E-15 ) ) ;
#32516 = VECTOR ( 'NONE', #16329, 1000.000000000000114 ) ;
#32517 = ORIENTED_EDGE ( 'NONE', *, *, #42378, .F. ) ;
#32518 = AXIS2_PLACEMENT_3D ( 'NONE', #6369, #47345, #22396 ) ;
#32519 = PLANE ( 'NONE',  #22635 ) ;
#32520 = FACE_OUTER_BOUND ( 'NONE', #19269, .T. ) ;
#32522 = ORIENTED_EDGE ( 'NONE', *, *, #48029, .T. ) ;
#32521 = CARTESIAN_POINT ( 'NONE',  ( 68.79964045138288498, -183.6283474603465606, 43.25148278810711844 ) ) ;
#32523 = LINE ( 'NONE', #28569, #15172 ) ;
#32524 = ORIENTED_EDGE ( 'NONE', *, *, #4144, .F. ) ;
#32525 = VERTEX_POINT ( 'NONE', #23142 ) ;
#32526 = FACE_OUTER_BOUND ( 'NONE', #43797, .T. ) ;
#32527 = VECTOR ( 'NONE', #32678, 1000.000000000000000 ) ;
#32528 = VECTOR ( 'NONE', #19949, 1000.000000000000000 ) ;
#32529 = VERTEX_POINT ( 'NONE', #11034 ) ;
#32530 = CYLINDRICAL_SURFACE ( 'NONE', #30095, 125.0000000000000000 ) ;
#32531 = DIRECTION ( 'NONE',  ( -0.2635871660690783380, 0.000000000000000000, 0.9646355819083558547 ) ) ;
#32532 = DIRECTION ( 'NONE',  ( -0.9266896074318370369, 0.000000000000000000, 0.3758275821142292306 ) ) ;
#32533 = CIRCLE ( 'NONE', #13264, 125.0000000000000000 ) ;
#32534 = EDGE_CURVE ( 'NONE', #33013, #3044, #10275, .T. ) ;
#32535 =( LENGTH_UNIT ( ) NAMED_UNIT ( * ) SI_UNIT ( .MILLI., .METRE. ) );
#32536 = CARTESIAN_POINT ( 'NONE',  ( -113.4314575050762102, -123.5000000000000284, 20.00000000000002487 ) ) ;
#32537 = ORIENTED_EDGE ( 'NONE', *, *, #6568, .T. ) ;
#32540 = ORIENTED_EDGE ( 'NONE', *, *, #31650, .T. ) ;
#32539 = LINE ( 'NONE', #44628, #36467 ) ;
#32538 = DIRECTION ( 'NONE',  ( 0.5315839928299667116, 0.000000000000000000, -0.8470055835512242393 ) ) ;
#32541 = VECTOR ( 'NONE', #41631, 1000.000000000000000 ) ;
#32542 = ORIENTED_EDGE ( 'NONE', *, *, #25012, .F. ) ;
#32543 = VECTOR ( 'NONE', #46144, 1000.000000000000000 ) ;
#32544 = CARTESIAN_POINT ( 'NONE',  ( -48.53836737940255119, -193.5000000000000000, -0.9982437317643153563 ) ) ;
#32545 = VERTEX_POINT ( 'NONE', #50744 ) ;
#32546 = FACE_OUTER_BOUND ( 'NONE', #49249, .T. ) ;
#32547 = EDGE_LOOP ( 'NONE', ( #2975, #35378, #21394, #24650 ) ) ;
#32548 = PLANE ( 'NONE',  #27108 ) ;
#32549 = DIRECTION ( 'NONE',  ( 0.000000000000000000, 0.000000000000000000, 1.000000000000000000 ) ) ;
#32550 = ORIENTED_EDGE ( 'NONE', *, *, #35940, .T. ) ;
#32552 = CARTESIAN_POINT ( 'NONE',  ( -330.4913330509368166, -115.7716958700755470, -59.50019592636139265 ) ) ;
#32551 = CARTESIAN_POINT ( 'NONE',  ( -48.47912675150885065, -189.7472609257535510, 6.938893903907228378E-15 ) ) ;
#32553 = ORIENTED_EDGE ( 'NONE', *, *, #11391, .T. ) ;
#32554 = VECTOR ( 'NONE', #25240, 1000.000000000000114 ) ;
#32555 = VERTEX_POINT ( 'NONE', #7107 ) ;
#32556 = DIRECTION ( 'NONE',  ( -0.000000000000000000, 1.000000000000000000, -0.000000000000000000 ) ) ;
#32557 = DIRECTION ( 'NONE',  ( 0.8124868780056825335, 0.000000000000000000, -0.5829794791144703447 ) ) ;
#32558 = EDGE_CURVE ( 'NONE', #5960, #34734, #8859, .T. ) ;
#32559 = LINE ( 'NONE', #25201, #341 ) ;
#32560 = DIRECTION ( 'NONE',  ( 0.6068001458185834363, 0.000000000000000000, 0.7948544414133608127 ) ) ;
#32561 = DIRECTION ( 'NONE',  ( 0.000000000000000000, -0.000000000000000000, -1.000000000000000000 ) ) ;
#32562 = LINE ( 'NONE', #48612, #7111 ) ;
#32563 = SHAPE_DEFINITION_REPRESENTATION ( #46172, #33116 ) ;
#32564 = CARTESIAN_POINT ( 'NONE',  ( 57.66105628977221897, -193.5000000000000000, 66.02470404298190942 ) ) ;
#32565 = DIRECTION ( 'NONE',  ( -0.000000000000000000, 0.9350162426854194964, 0.3546048870425235200 ) ) ;
#32566 = LINE ( 'NONE', #33082, #42464 ) ;
#32567 = FACE_OUTER_BOUND ( 'NONE', #12045, .T. ) ;
#32568 = EDGE_LOOP ( 'NONE', ( #36731, #20533, #41139, #35099 ) ) ;
#32569 = AXIS2_PLACEMENT_3D ( 'NONE', #27110, #30539, #23192 ) ;
#32570 = EDGE_LOOP ( 'NONE', ( #16617, #9260, #34246, #24694 ) ) ;
#32571 = AXIS2_PLACEMENT_3D ( 'NONE', #26205, #21507, #2317 ) ;
#32572 = DIRECTION ( 'NONE',  ( 0.000000000000000000, -1.000000000000000000, 0.000000000000000000 ) ) ;
#32573 = VECTOR ( 'NONE', #4813, 999.9999999999998863 ) ;
#32574 = CARTESIAN_POINT ( 'NONE',  ( 0.000000000000000000, -130.6116641350635064, 58.56982357178529242 ) ) ;
#32575 = FACE_OUTER_BOUND ( 'NONE', #14328, .T. ) ;
#32576 = ORIENTED_EDGE ( 'NONE', *, *, #39465, .F. ) ;
#32577 = ORIENTED_EDGE ( 'NONE', *, *, #16934, .F. ) ;
#32578 = ORIENTED_EDGE ( 'NONE', *, *, #18255, .F. ) ;
#32579 = CIRCLE ( 'NONE', #42636, 125.0000000000000000 ) ;
#32580 = DIRECTION ( 'NONE',  ( -0.000000000000000000, -0.1205366802553268363, -0.9927088740980534176 ) ) ;
#32581 = CARTESIAN_POINT ( 'NONE',  ( -305.0000000000000568, -76.88706545914891421, 37.77875505479673279 ) ) ;
#32582 = CARTESIAN_POINT ( 'NONE',  ( -138.3705904895685705, -177.1207230881787780, -86.85922373029296750 ) ) ;
#32583 = LINE ( 'NONE', #12605, #24523 ) ;
#32584 = EDGE_LOOP ( 'NONE', ( #19664, #26266, #42155, #45305 ) ) ;
#32585 = EDGE_CURVE ( 'NONE', #13145, #42367, #38388, .T. ) ;
#32586 = CARTESIAN_POINT ( 'NONE',  ( -168.3100285466275636, -189.7472609257535510, -31.88354567335001377 ) ) ;
#32587 = DIRECTION ( 'NONE',  ( 0.000000000000000000, 0.000000000000000000, 1.000000000000000000 ) ) ;
#32588 = VERTEX_POINT ( 'NONE', #22628 ) ;
#32589 = VECTOR ( 'NONE', #23115, 1000.000000000000000 ) ;
#32590 = CARTESIAN_POINT ( 'NONE',  ( -135.4449840867448813, -189.7472609257535510, -88.39086586114741806 ) ) ;
#32591 = ADVANCED_FACE ( 'NONE', ( #2641 ), #30756, .T. ) ;
#32592 = VERTEX_POINT ( 'NONE', #3164 ) ;
#32593 = VERTEX_POINT ( 'NONE', #10524 ) ;
#32594 = DIRECTION ( 'NONE',  ( -0.000000000000000000, 1.000000000000000000, -0.000000000000000000 ) ) ;
#32595 = EDGE_CURVE ( 'NONE', #23874, #30234, #34949, .T. ) ;
#32596 = EDGE_CURVE ( 'NONE', #11859, #44930, #35214, .T. ) ;
#32597 = DIRECTION ( 'NONE',  ( 0.000000000000000000, 1.000000000000000000, 0.000000000000000000 ) ) ;
#32598 = LINE ( 'NONE', #24202, #5105 ) ;
#32599 = PRODUCT_DEFINITION_FORMATION_WITH_SPECIFIED_SOURCE ( 'ANY', '', #49932, .NOT_KNOWN. ) ;
#32602 = EDGE_LOOP ( 'NONE', ( #17736, #22658, #527, #45696 ) ) ;
#32601 = DIRECTION ( 'NONE',  ( -1.000000000000000000, -6.921107616850733752E-15, 7.812315528781911911E-15 ) ) ;
#32600 = CARTESIAN_POINT ( 'NONE',  ( -169.6719064342497916, -183.6283474603465606, 30.61552143554989414 ) ) ;
#32603 = AXIS2_PLACEMENT_3D ( 'NONE', #36895, #17182, #48983 ) ;
#32604 = EDGE_CURVE ( 'NONE', #40906, #36985, #18428, .T. ) ;
#32605 = VECTOR ( 'NONE', #46506, 1000.000000000000227 ) ;
#32606 = DIRECTION ( 'NONE',  ( 0.000000000000000000, 1.000000000000000000, 0.000000000000000000 ) ) ;
#32607 = ORIENTED_EDGE ( 'NONE', *, *, #6385, .F. ) ;
#32608 = DIRECTION ( 'NONE',  ( 0.000000000000000000, -0.6631226582407863113, 0.7485107481711089639 ) ) ;
#32610 = CIRCLE ( 'NONE', #3207, 15.24495751795539000 ) ;
#32609 = LINE ( 'NONE', #28394, #21596 ) ;
#32611 = ORIENTED_EDGE ( 'NONE', *, *, #27507, .F. ) ;
#32612 = CARTESIAN_POINT ( 'NONE',  ( -49.47517659412407198, -193.5000000000000000, 0.08879589532293177823 ) ) ;
#32613 = DIRECTION ( 'NONE',  ( -0.5586467658036535777, 0.000000000000000000, 0.8294056854502011022 ) ) ;
#32615 = CARTESIAN_POINT ( 'NONE',  ( -336.3521761649654422, -76.43926241122620979, -35.68215131113738181 ) ) ;
#32614 = CARTESIAN_POINT ( 'NONE',  ( -47.66663987350317910, -183.6283474603465606, 0.5829794791144832233 ) ) ;
#32616 = EDGE_LOOP ( 'NONE', ( #39367, #19802, #9231, #40629 ) ) ;
#32617 = CIRCLE ( 'NONE', #6605, 125.0000000000000000 ) ;
#32618 = LINE ( 'NONE', #5035, #11420 ) ;
#32619 = FACE_OUTER_BOUND ( 'NONE', #20992, .T. ) ;
#32620 = DIRECTION ( 'NONE',  ( 0.000000000000000000, 1.000000000000000000, 0.000000000000000000 ) ) ;
#32621 = ORIENTED_EDGE ( 'NONE', *, *, #9538, .F. ) ;
#32622 = EDGE_CURVE ( 'NONE', #26442, #9007, #43302, .T. ) ;
#32623 = DIRECTION ( 'NONE',  ( -1.000000000000000000, 0.000000000000000000, 0.000000000000000000 ) ) ;
#32624 = DIRECTION ( 'NONE',  ( 0.000000000000000000, 0.7485107481710999711, -0.6631226582407964143 ) ) ;
#32625 = PLANE ( 'NONE',  #49207 ) ;
#32626 = VERTEX_POINT ( 'NONE', #6606 ) ;
#32627 = CARTESIAN_POINT ( 'NONE',  ( -167.9436818089035626, -183.6283474603465606, 36.78613984830037253 ) ) ;
#32628 = AXIS2_PLACEMENT_3D ( 'NONE', #41147, #4369, #8560 ) ;
#32629 = ORIENTED_EDGE ( 'NONE', *, *, #6639, .T. ) ;
#32630 = LINE ( 'NONE', #24232, #40868 ) ;
#32631 = ORIENTED_EDGE ( 'NONE', *, *, #35550, .F. ) ;
#32632 = DIRECTION ( 'NONE',  ( -0.000000000000000000, 0.6631226582408039638, 0.7485107481710934207 ) ) ;
#32633 = DIRECTION ( 'NONE',  ( 0.000000000000000000, 0.000000000000000000, -1.000000000000000000 ) ) ;
#32634 = DIRECTION ( 'NONE',  ( 0.000000000000000000, 0.000000000000000000, -1.000000000000000000 ) ) ;
#32635 = DIRECTION ( 'NONE',  ( 0.000000000000000000, -0.000000000000000000, -1.000000000000000000 ) ) ;
#32636 = PLANE ( 'NONE',  #1435 ) ;
#32637 = DIRECTION ( 'NONE',  ( 0.000000000000000000, -1.000000000000000000, 0.000000000000000000 ) ) ;
#32638 = VECTOR ( 'NONE', #32580, 1000.000000000000227 ) ;
#32639 = CYLINDRICAL_SURFACE ( 'NONE', #22799, 124.9999999999999858 ) ;
#32640 = DIRECTION ( 'NONE',  ( 0.000000000000000000, 0.8854560256532093554, -0.4647231720437695057 ) ) ;
#32642 = VERTEX_POINT ( 'NONE', #7378 ) ;
#32641 = CARTESIAN_POINT ( 'NONE',  ( -339.1964088526558498, -115.8919814278862503, 58.50955523165745831 ) ) ;
#32643 = AXIS2_PLACEMENT_3D ( 'NONE', #17560, #21485, #24639 ) ;
#32644 = ORIENTED_EDGE ( 'NONE', *, *, #38355, .T. ) ;
#32645 = EDGE_CURVE ( 'NONE', #16943, #9203, #18141, .T. ) ;
#32646 = ADVANCED_FACE ( 'NONE', ( #10793 ), #23400, .T. ) ;
#32647 = LINE ( 'NONE', #585, #40021 ) ;
#32648 = DIRECTION ( 'NONE',  ( 0.000000000000000000, -1.000000000000000000, -0.000000000000000000 ) ) ;
#32649 = VERTEX_POINT ( 'NONE', #46294 ) ;
#32650 = AXIS2_PLACEMENT_3D ( 'NONE', #42203, #22238, #34333 ) ;
#32651 = VERTEX_POINT ( 'NONE', #46807 ) ;
#32652 = EDGE_LOOP ( 'NONE', ( #13258, #47324, #1901, #28880 ) ) ;
#32653 = PLANE ( 'NONE',  #27506 ) ;
#32654 = EDGE_CURVE ( 'NONE', #21416, #20906, #34445, .T. ) ;
#32655 = DIRECTION ( 'NONE',  ( 0.000000000000000000, 1.000000000000000000, 0.000000000000000000 ) ) ;
#32656 = CARTESIAN_POINT ( 'NONE',  ( -339.1964088526558498, -143.9541802141663709, 55.34326076196097688 ) ) ;
#32657 = ORIENTED_EDGE ( 'NONE', *, *, #25379, .F. ) ;
#32658 = ORIENTED_EDGE ( 'NONE', *, *, #46606, .F. ) ;
#32659 = EDGE_CURVE ( 'NONE', #39601, #31150, #34697, .T. ) ;
#32660 = CIRCLE ( 'NONE', #41058, 125.0000000000000000 ) ;
#32661 = CARTESIAN_POINT ( 'NONE',  ( -332.3517673607765914, -146.8829211657874794, -54.23253582808848705 ) ) ;
#32662 = DIRECTION ( 'NONE',  ( 0.000000000000000000, 0.000000000000000000, -1.000000000000000000 ) ) ;
#32664 = EDGE_LOOP ( 'NONE', ( #4349, #38658, #4382, #44802 ) ) ;
#32663 = CARTESIAN_POINT ( 'NONE',  ( -66.46933728415693565, -177.1207230881787780, 122.6885491605231522 ) ) ;
#32665 = ADVANCED_FACE ( 'NONE', ( #19440 ), #35462, .F. ) ;
#32666 = CARTESIAN_POINT ( 'NONE',  ( -31.47951320919342777, -183.6283474603465606, -122.8300162461135301 ) ) ;
#32667 = CARTESIAN_POINT ( 'NONE',  ( -152.3176060415594861, -183.6283474603465606, -69.58857822034966034 ) ) ;
#32668 = ORIENTED_EDGE ( 'NONE', *, *, #12429, .T. ) ;
#32669 = LINE ( 'NONE', #36611, #48188 ) ;
#32670 = ADVANCED_FACE ( 'NONE', ( #44662 ), #40692, .T. ) ;
#32671 = EDGE_LOOP ( 'NONE', ( #2178, #11351, #49654, #9521 ) ) ;
#32672 = CARTESIAN_POINT ( 'NONE',  ( -160.9694636715425702, -189.7472609257535510, 54.50618404931039862 ) ) ;
#32673 = DIRECTION ( 'NONE',  ( 0.000000000000000000, 0.000000000000000000, 1.000000000000000000 ) ) ;
#32674 = CARTESIAN_POINT ( 'NONE',  ( 10.73478887071927623, -183.6283474603465606, -110.0850225811106924 ) ) ;
#32675 = VERTEX_POINT ( 'NONE', #48622 ) ;
#32676 = ORIENTED_EDGE ( 'NONE', *, *, #41095, .F. ) ;
#32677 = DIRECTION ( 'NONE',  ( 0.000000000000000000, 0.000000000000000000, 1.000000000000000000 ) ) ;
#32679 = VECTOR ( 'NONE', #36387, 1000.000000000000000 ) ;
#32678 = DIRECTION ( 'NONE',  ( -1.000000000000000000, 0.000000000000000000, 0.000000000000000000 ) ) ;
#32680 = ORIENTED_EDGE ( 'NONE', *, *, #24044, .F. ) ;
#32681 = DIRECTION ( 'NONE',  ( 0.000000000000000000, -0.000000000000000000, -1.000000000000000000 ) ) ;
#32682 = PRESENTATION_LAYER_ASSIGNMENT (  '', '', ( #10041 ) ) ;
#32683 = DIRECTION ( 'NONE',  ( 0.000000000000000000, 1.000000000000000000, -0.000000000000000000 ) ) ;
#32684 = ORIENTED_EDGE ( 'NONE', *, *, #39240, .T. ) ;
#32685 = PLANE ( 'NONE',  #6622 ) ;
#32686 = CARTESIAN_POINT ( 'NONE',  ( -339.1964088526558498, -143.9541802141663709, 55.34326076196097688 ) ) ;
#32687 = PRODUCT_DEFINITION_SHAPE ( 'NONE', 'NONE',  #52050 ) ;
#32688 = ORIENTED_EDGE ( 'NONE', *, *, #39706, .F. ) ;
#32689 = DIRECTION ( 'NONE',  ( 0.4031234292879600778, 0.000000000000000000, 0.9151456172430237901 ) ) ;
#32690 = VERTEX_POINT ( 'NONE', #43620 ) ;
#32691 = CARTESIAN_POINT ( 'NONE',  ( -332.3517673607765914, -91.32752733096738496, -49.48329383994654052 ) ) ;
#32692 = VERTEX_POINT ( 'NONE', #15791 ) ;
#32693 = CARTESIAN_POINT ( 'NONE',  ( 20.66186849114819069, -175.3837268820161057, -104.1370384486465070 ) ) ;
#32694 = DIRECTION ( 'NONE',  ( 1.000000000000000000, 0.000000000000000000, -0.000000000000000000 ) ) ;
#32695 = CYLINDRICAL_SURFACE ( 'NONE', #24058, 124.9999999999999858 ) ;
#32696 = DIRECTION ( 'NONE',  ( 0.000000000000000000, -1.000000000000000000, -0.000000000000000000 ) ) ;
#32697 = AXIS2_PLACEMENT_3D ( 'NONE', #18419, #50735, #21847 ) ;
#32698 = EDGE_LOOP ( 'NONE', ( #21679, #45562, #5973, #49823 ) ) ;
#32699 = CARTESIAN_POINT ( 'NONE',  ( 1.755575411425451593, -189.7472609257535510, 114.4616734920527108 ) ) ;
#32700 = ORIENTED_EDGE ( 'NONE', *, *, #11850, .F. ) ;
#32701 = ADVANCED_FACE ( 'NONE', ( #4204 ), #16283, .T. ) ;
#32702 = ORIENTED_EDGE ( 'NONE', *, *, #36819, .T. ) ;
#32703 = DIRECTION ( 'NONE',  ( 0.000000000000000000, 0.000000000000000000, 1.000000000000000000 ) ) ;
#32705 = ORIENTED_EDGE ( 'NONE', *, *, #24358, .T. ) ;
#32704 = DIRECTION ( 'NONE',  ( 0.000000000000000000, 0.000000000000000000, -1.000000000000000000 ) ) ;
#32706 = EDGE_CURVE ( 'NONE', #39306, #21525, #44412, .T. ) ;
#32707 = EDGE_LOOP ( 'NONE', ( #40437, #5212, #41374, #46266 ) ) ;
#32708 = EDGE_CURVE ( 'NONE', #34125, #50975, #24850, .T. ) ;
#32709 = LINE ( 'NONE', #9069, #27393 ) ;
#32710 = ADVANCED_FACE ( 'NONE', ( #19969 ), #41607, .T. ) ;
#32711 = EDGE_CURVE ( 'NONE', #51319, #11294, #40775, .T. ) ;
#32712 = LINE ( 'NONE', #4597, #10037 ) ;
#32713 = EDGE_LOOP ( 'NONE', ( #21510, #36152, #36670, #29280 ) ) ;
#32714 = AXIS2_PLACEMENT_3D ( 'NONE', #15804, #48104, #12075 ) ;
#32715 = LINE ( 'NONE', #8792, #41545 ) ;
#32716 = EDGE_CURVE ( 'NONE', #12665, #37026, #19694, .T. ) ;
#32717 = ORIENTED_EDGE ( 'NONE', *, *, #16409, .F. ) ;
#32718 = CARTESIAN_POINT ( 'NONE',  ( -46.00000000000000711, 20.00000000000000000, -4.999999999999988454 ) ) ;
#32719 = DIRECTION ( 'NONE',  ( -0.8294056854502090959, 0.000000000000000000, 0.5586467658036415873 ) ) ;
#32720 = ADVANCED_FACE ( 'NONE', ( #7620 ), #3945, .F. ) ;
#32721 = CARTESIAN_POINT ( 'NONE',  ( -32.87124591993210743, -193.5000000000000000, 124.0217483183788119 ) ) ;
#32722 = FACE_OUTER_BOUND ( 'NONE', #45528, .T. ) ;
#32723 = EDGE_LOOP ( 'NONE', ( #48945, #42238, #22478, #43229 ) ) ;
#32724 = ORIENTED_EDGE ( 'NONE', *, *, #45780, .T. ) ;
#32725 = EDGE_CURVE ( 'NONE', #23338, #50146, #11806, .T. ) ;
#32726 = ORIENTED_EDGE ( 'NONE', *, *, #33678, .F. ) ;
#32727 = LINE ( 'NONE', #48247, #48419 ) ;
#32728 = CARTESIAN_POINT ( 'NONE',  ( -330.4913330509368166, -144.8891964568517778, 54.98865587491845730 ) ) ;
#32729 = EDGE_CURVE ( 'NONE', #7333, #21574, #51784, .T. ) ;
#32730 = DIRECTION ( 'NONE',  ( -1.000000000000000000, 0.000000000000000000, 0.000000000000000000 ) ) ;
#32731 = FACE_BOUND ( 'NONE', #11678, .T. ) ;
#32732 = CARTESIAN_POINT ( 'NONE',  ( -339.1964088526558498, -109.6270296344155923, 58.37414404713457117 ) ) ;
#32733 = ORIENTED_EDGE ( 'NONE', *, *, #13500, .F. ) ;
#32734 = ADVANCED_FACE ( 'NONE', ( #32038 ), #12331, .T. ) ;
#32735 = EDGE_CURVE ( 'NONE', #21250, #26284, #39655, .T. ) ;
#32736 = AXIS2_PLACEMENT_3D ( 'NONE', #3506, #7203, #4285 ) ;
#32737 = CIRCLE ( 'NONE', #10089, 125.0000000000000000 ) ;
#32738 = VERTEX_POINT ( 'NONE', #16034 ) ;
#32740 = VERTEX_POINT ( 'NONE', #39914 ) ;
#32739 = DIRECTION ( 'NONE',  ( -0.000000000000000000, 1.000000000000000000, -0.000000000000000000 ) ) ;
#32741 = DIRECTION ( 'NONE',  ( 0.1476465640024851034, 0.000000000000000000, -0.9890401873221634776 ) ) ;
#32742 = ORIENTED_EDGE ( 'NONE', *, *, #46148, .T. ) ;
#32743 = CARTESIAN_POINT ( 'NONE',  ( -339.1964088526558498, -182.5000000000000568, -0.4999999999999543698 ) ) ;
#32744 = CARTESIAN_POINT ( 'NONE',  ( -48.77118352214583297, -193.5000000000000000, 0.9564009842765270886 ) ) ;
#32745 = LINE ( 'NONE', #694, #8700 ) ;
#32746 = LINE ( 'NONE', #36415, #36837 ) ;
#32747 = VERTEX_POINT ( 'NONE', #48084 ) ;
#32748 = CARTESIAN_POINT ( 'NONE',  ( -336.3521761649654422, -65.24746378767824240, -9.724760635741734660 ) ) ;
#32749 = VERTEX_POINT ( 'NONE', #12062 ) ;
#32750 = EDGE_CURVE ( 'NONE', #41700, #794, #21521, .T. ) ;
#32751 = EDGE_CURVE ( 'NONE', #33603, #34940, #36243, .T. ) ;
#32752 = ORIENTED_EDGE ( 'NONE', *, *, #5806, .F. ) ;
#32753 = FACE_OUTER_BOUND ( 'NONE', #49923, .T. ) ;
#32754 = AXIS2_PLACEMENT_3D ( 'NONE', #48298, #12283, #12798 ) ;
#32755 = DIRECTION ( 'NONE',  ( 0.000000000000000000, 0.000000000000000000, 1.000000000000000000 ) ) ;
#32756 = CARTESIAN_POINT ( 'NONE',  ( 19.33815737959698566, -183.6283474603465606, 105.0038855142078091 ) ) ;
#32757 = CARTESIAN_POINT ( 'NONE',  ( -173.0563034899574859, -193.5000000000000000, -10.27263529369817618 ) ) ;
#32758 = DIRECTION ( 'NONE',  ( -0.000000000000000000, 1.000000000000000000, -0.000000000000000000 ) ) ;
#32759 = CARTESIAN_POINT ( 'NONE',  ( 6.443011874827243801, -193.5000000000000000, 112.2878385610370771 ) ) ;
#32760 = LINE ( 'NONE', #33279, #22022 ) ;
#32761 = VERTEX_POINT ( 'NONE', #239 ) ;
#32762 = DIRECTION ( 'NONE',  ( -0.000000000000000000, -1.000000000000000000, 0.000000000000000000 ) ) ;
#32763 = DIRECTION ( 'NONE',  ( -1.000000000000000000, 0.000000000000000000, 0.000000000000000000 ) ) ;
#32764 = CARTESIAN_POINT ( 'NONE',  ( -167.8725343822893024, -193.5000000000000000, 33.48461921608603120 ) ) ;
#32765 = FACE_BOUND ( 'NONE', #44599, .T. ) ;
#32766 = EDGE_LOOP ( 'NONE', ( #36236, #18806, #27531, #27679 ) ) ;
#32767 = FACE_OUTER_BOUND ( 'NONE', #42446, .T. ) ;
#32768 = ORIENTED_EDGE ( 'NONE', *, *, #28055, .F. ) ;
#32769 = CARTESIAN_POINT ( 'NONE',  ( -30.48891621885993430, -177.1207230881787780, -122.6885491605229959 ) ) ;
#32770 = ADVANCED_FACE ( 'NONE', ( #24426 ), #4458, .T. ) ;
#32771 = EDGE_LOOP ( 'NONE', ( #35742, #19627, #18714, #41575 ) ) ;
#32772 = EDGE_CURVE ( 'NONE', #18907, #18264, #13940, .T. ) ;
#32773 = DIRECTION ( 'NONE',  ( -1.000000000000000000, -0.000000000000000000, -0.000000000000000000 ) ) ;
#32774 = ORIENTED_EDGE ( 'NONE', *, *, #21853, .T. ) ;
#32775 = CIRCLE ( 'NONE', #50314, 60.00000000000000000 ) ;
#32776 = EDGE_CURVE ( 'NONE', #1404, #47168, #24956, .T. ) ;
#32777 = VECTOR ( 'NONE', #32108, 1000.000000000000000 ) ;
#32778 = EDGE_CURVE ( 'NONE', #15315, #16523, #44923, .T. ) ;
#32779 = CARTESIAN_POINT ( 'NONE',  ( 55.10060313344061456, -177.1207230881787780, 68.17212999877223467 ) ) ;
#32780 = CARTESIAN_POINT ( 'NONE',  ( -330.4913330509368166, -123.5000000000000284, 0.000000000000000000 ) ) ;
#32782 = VERTEX_POINT ( 'NONE', #8912 ) ;
#32781 = CARTESIAN_POINT ( 'NONE',  ( -98.31070548515602070, -193.5000000000000000, -113.5465278748093283 ) ) ;
#32783 = LINE ( 'NONE', #24135, #11769 ) ;
#32784 = EDGE_LOOP ( 'NONE', ( #33818, #48973, #8182, #4081 ) ) ;
#32785 = ORIENTED_EDGE ( 'NONE', *, *, #27363, .T. ) ;
#32786 = CARTESIAN_POINT ( 'NONE',  ( -180.0000000000000568, -123.5000000000000284, 0.000000000000000000 ) ) ;
#32787 = DIRECTION ( 'NONE',  ( 0.6528221181905227155, 0.000000000000000000, -0.7575112421616191360 ) ) ;
#32788 = VECTOR ( 'NONE', #21412, 1000.000000000000000 ) ;
#32789 = EDGE_LOOP ( 'NONE', ( #41810, #34855, #34188, #14009 ) ) ;
#32790 = FILL_AREA_STYLE ('',( #4952 ) ) ;
#32791 = DIRECTION ( 'NONE',  ( -1.000000000000000000, 0.000000000000000000, 0.000000000000000000 ) ) ;
#32792 = CARTESIAN_POINT ( 'NONE',  ( 76.01188277843579044, -175.3837268820161057, 11.26891947860284482 ) ) ;
#32793 = ADVANCED_FACE ( 'NONE', ( #40972 ), #22929, .T. ) ;
#32794 = DIRECTION ( 'NONE',  ( 0.3482016354343928088, 0.000000000000000000, 0.9374196611341231167 ) ) ;
#32795 = CARTESIAN_POINT ( 'NONE',  ( -96.65280530915693191, -193.5000000000000000, -115.3442529744087466 ) ) ;
#32796 = EDGE_LOOP ( 'NONE', ( #9142, #15251, #18263, #23317 ) ) ;
#32799 = VERTEX_POINT ( 'NONE', #26859 ) ;
#32798 =( NAMED_UNIT ( * ) SI_UNIT ( $, .STERADIAN. ) SOLID_ANGLE_UNIT ( ) );
#32797 = CARTESIAN_POINT ( 'NONE',  ( -339.1964088526558498, -66.09477493971894546, 13.63415328425207917 ) ) ;
#32800 = ORIENTED_EDGE ( 'NONE', *, *, #5076, .F. ) ;
#32801 = LINE ( 'NONE', #24925, #8877 ) ;
#32802 = VERTEX_POINT ( 'NONE', #31064 ) ;
#32803 = AXIS2_PLACEMENT_3D ( 'NONE', #31073, #35023, #7929 ) ;
#32804 = ORIENTED_EDGE ( 'NONE', *, *, #30121, .F. ) ;
#32805 = DIRECTION ( 'NONE',  ( 0.000000000000000000, 0.000000000000000000, 1.000000000000000000 ) ) ;
#32806 = DIRECTION ( 'NONE',  ( -0.000000000000000000, 1.000000000000000000, -0.000000000000000000 ) ) ;
#32807 = ORIENTED_EDGE ( 'NONE', *, *, #9246, .T. ) ;
#32809 = CARTESIAN_POINT ( 'NONE',  ( 42.89728982752368580, -189.7472609257535510, 83.82333043185313670 ) ) ;
#32808 = DIRECTION ( 'NONE',  ( -1.000000000000000000, -0.000000000000000000, -0.000000000000000000 ) ) ;
#32810 = EDGE_LOOP ( 'NONE', ( #18367, #9638, #44391, #28352 ) ) ;
#32811 = AXIS2_PLACEMENT_3D ( 'NONE', #27594, #19697, #35730 ) ;
#32812 = VERTEX_POINT ( 'NONE', #15062 ) ;
#32813 = DIRECTION ( 'NONE',  ( 0.9890401873221623674, 0.000000000000000000, 0.1476465640024917925 ) ) ;
#32814 = CARTESIAN_POINT ( 'NONE',  ( -48.47912675150885065, -120.5000000000000284, -14.00000000000000355 ) ) ;
#32815 = FACE_OUTER_BOUND ( 'NONE', #51915, .T. ) ;
#32816 = DIRECTION ( 'NONE',  ( 0.000000000000000000, -0.9927088740980548609, -0.1205366802553164696 ) ) ;
#32817 = ORIENTED_EDGE ( 'NONE', *, *, #30878, .T. ) ;
#32818 = CARTESIAN_POINT ( 'NONE',  ( -87.88805327685028601, -193.5000000000000000, 117.5715283571807106 ) ) ;
#32819 = FACE_OUTER_BOUND ( 'NONE', #46974, .T. ) ;
#32820 = CARTESIAN_POINT ( 'NONE',  ( -158.6498865914718408, -183.6283474603465606, 56.90809649257569447 ) ) ;
#32821 = CARTESIAN_POINT ( 'NONE',  ( -336.3521761649654422, -72.48138011061176655, -29.74944317415788930 ) ) ;
#32822 = DIRECTION ( 'NONE',  ( 0.000000000000000000, -0.9709418174260544543, -0.2393156642875482742 ) ) ;
#32823 = EDGE_LOOP ( 'NONE', ( #4926, #48768, #50852, #36388 ) ) ;
#32824 = ORIENTED_EDGE ( 'NONE', *, *, #14943, .T. ) ;
#32825 = AXIS2_PLACEMENT_3D ( 'NONE', #10050, #9271, #16898 ) ;
#32826 = DIRECTION ( 'NONE',  ( 1.000000000000000000, 0.000000000000000000, 0.000000000000000000 ) ) ;
#32827 = CARTESIAN_POINT ( 'NONE',  ( -48.65601702663141737, -175.3837268820161057, -0.9842305779475923888 ) ) ;
#32828 = LINE ( 'NONE', #40977, #37172 ) ;
#32829 = ORIENTED_EDGE ( 'NONE', *, *, #8860, .F. ) ;
#32830 = ADVANCED_FACE ( 'NONE', ( #27113 ), #38940, .F. ) ;
#32831 = ORIENTED_EDGE ( 'NONE', *, *, #36868, .F. ) ;
#32832 = VERTEX_POINT ( 'NONE', #50795 ) ;
#32833 = DIRECTION ( 'NONE',  ( -0.000000000000000000, 1.000000000000000000, -0.000000000000000000 ) ) ;
#32834 = CARTESIAN_POINT ( 'NONE',  ( -330.4913330509368166, -63.87926739338325888, 6.735595255825880479 ) ) ;
#32835 = CARTESIAN_POINT ( 'NONE',  ( -69.59623518921149810, -193.5000000000000000, 122.1886788576024117 ) ) ;
#32836 = DIRECTION ( 'NONE',  ( 0.000000000000000000, 0.000000000000000000, 1.000000000000000000 ) ) ;
#32837 = VECTOR ( 'NONE', #17780, 1000.000000000000000 ) ;
#32838 = EDGE_LOOP ( 'NONE', ( #47025, #11213, #1693, #38533 ) ) ;
#32839 = DIRECTION ( 'NONE',  ( 0.000000000000000000, -0.4647231720437573488, 0.8854560256532157947 ) ) ;
#32840 = LINE ( 'NONE', #20766, #34408 ) ;
#32841 = VECTOR ( 'NONE', #32242, 1000.000000000000000 ) ;
#32842 = DIRECTION ( 'NONE',  ( 0.000000000000000000, 0.7485107481710977506, -0.6631226582407989678 ) ) ;
#32843 = VERTEX_POINT ( 'NONE', #22419 ) ;
#32844 = PRODUCT_RELATED_PRODUCT_CATEGORY ( 'part', '', ( #49932 ) ) ;
#32845 = ORIENTED_EDGE ( 'NONE', *, *, #50656, .F. ) ;
#32846 = EDGE_CURVE ( 'NONE', #42603, #23845, #3462, .T. ) ;
#32847 = DIRECTION ( 'NONE',  ( 1.000000000000000000, -0.000000000000000000, -0.000000000000000000 ) ) ;
#32848 = AXIS2_PLACEMENT_3D ( 'NONE', #3031, #44012, #35597 ) ;
#32849 = LINE ( 'NONE', #40214, #41671 ) ;
#32852 = ORIENTED_EDGE ( 'NONE', *, *, #35002, .T. ) ;
#32851 = CARTESIAN_POINT ( 'NONE',  ( -332.3517673607765914, -113.7752393642576720, 58.25253621232167944 ) ) ;
#32850 = DIRECTION ( 'NONE',  ( -0.000000000000000000, -0.2393156642875482742, 0.9709418174260544543 ) ) ;
#32853 = AXIS2_PLACEMENT_3D ( 'NONE', #18826, #30922, #27491 ) ;
#32854 = DIRECTION ( 'NONE',  ( 0.000000000000000000, 1.000000000000000000, 0.000000000000000000 ) ) ;
#32855 = EDGE_LOOP ( 'NONE', ( #26014, #33482, #50796, #36898 ) ) ;
#32856 = DIRECTION ( 'NONE',  ( 0.000000000000000000, 0.000000000000000000, 1.000000000000000000 ) ) ;
#32857 = CARTESIAN_POINT ( 'NONE',  ( -332.3517673607765914, -111.9361751271348879, -57.91551518289410438 ) ) ;
#32858 = VERTEX_POINT ( 'NONE', #34489 ) ;
#32859 = EDGE_CURVE ( 'NONE', #16210, #23109, #42891, .T. ) ;
#32860 = LINE ( 'NONE', #24997, #10753 ) ;
#32862 = DIRECTION ( 'NONE',  ( 0.000000000000000000, -1.000000000000000000, 0.000000000000000000 ) ) ;
#32861 = CARTESIAN_POINT ( 'NONE',  ( 32.34187644556187990, -193.5000000000000000, 94.04236105995857997 ) ) ;
#32863 = EDGE_LOOP ( 'NONE', ( #44333, #1499, #3867, #12951 ) ) ;
#32864 = DIRECTION ( 'NONE',  ( 0.9995608365087944591, 0.000000000000000000, -0.02963332782255633305 ) ) ;
#32865 = CARTESIAN_POINT ( 'NONE',  ( -260.0000000000000000, 0.000000000000000000, 0.000000000000000000 ) ) ;
#32866 = DIRECTION ( 'NONE',  ( -0.000000000000000000, 1.000000000000000000, -0.000000000000000000 ) ) ;
#32867 = EDGE_CURVE ( 'NONE', #5084, #28167, #8904, .T. ) ;
#32868 = VERTEX_POINT ( 'NONE', #7156 ) ;
#32869 = CARTESIAN_POINT ( 'NONE',  ( -49.47517659412407198, -183.6283474603465606, 0.08879589532293177823 ) ) ;
#32870 = AXIS2_PLACEMENT_3D ( 'NONE', #22861, #6588, #31251 ) ;
#32871 = CARTESIAN_POINT ( 'NONE',  ( -48.47912675150885065, -183.6283474603465606, 6.938893903907228378E-15 ) ) ;
#32872 = EDGE_LOOP ( 'NONE', ( #10418, #51303, #47656, #6224 ) ) ;
#32873 = PLANE ( 'NONE',  #34035 ) ;
#32874 = AXIS2_PLACEMENT_3D ( 'NONE', #27661, #11635, #3735 ) ;
#32875 = ADVANCED_FACE ( 'NONE', ( #46860 ), #10844, .F. ) ;
#32876 = CARTESIAN_POINT ( 'NONE',  ( -165.5546359831674295, -183.6283474603465606, 43.79868877201490562 ) ) ;
#32877 = VERTEX_POINT ( 'NONE', #51069 ) ;
#32878 = DIRECTION ( 'NONE',  ( 0.6965510290629932655, 0.000000000000000000, 0.7175072570443347120 ) ) ;
#32879 = CARTESIAN_POINT ( 'NONE',  ( -34.51936650669028239, -189.7472609257535510, -124.2180546213278092 ) ) ;
#32880 = LINE ( 'NONE', #24751, #39478 ) ;
#32881 = CARTESIAN_POINT ( 'NONE',  ( 0.000000000000000000, -63.50000000000000000, 0.000000000000000000 ) ) ;
#32882 = FACE_OUTER_BOUND ( 'NONE', #47633, .T. ) ;
#32883 = EDGE_CURVE ( 'NONE', #21993, #29517, #51313, .T. ) ;
#32884 = VECTOR ( 'NONE', #47655, 1000.000000000000000 ) ;
#32885 = EDGE_CURVE ( 'NONE', #9853, #33172, #30292, .T. ) ;
#32886 = CARTESIAN_POINT ( 'NONE',  ( -92.16375985330356002, -193.5000000000000000, 117.1181148702521710 ) ) ;
#32887 = CIRCLE ( 'NONE', #1877, 125.0000000000000000 ) ;
#32888 = EDGE_CURVE ( 'NONE', #38482, #42654, #31319, .T. ) ;
#32889 = VECTOR ( 'NONE', #11904, 1000.000000000000000 ) ;
#32890 = DIRECTION ( 'NONE',  ( -0.000000000000000000, 1.000000000000000000, -0.000000000000000000 ) ) ;
#32892 = ORIENTED_EDGE ( 'NONE', *, *, #32203, .F. ) ;
#32891 = DIRECTION ( 'NONE',  ( -0.000000000000000000, 1.000000000000000000, -0.000000000000000000 ) ) ;
#32893 = ORIENTED_EDGE ( 'NONE', *, *, #36556, .T. ) ;
#32894 = CARTESIAN_POINT ( 'NONE',  ( -22.44626007086656472, -183.6283474603465606, 122.2591094863196872 ) ) ;
#32895 = FACE_OUTER_BOUND ( 'NONE', #23001, .T. ) ;
#32896 = VERTEX_POINT ( 'NONE', #3223 ) ;
#32897 = ORIENTED_EDGE ( 'NONE', *, *, #28955, .F. ) ;
#32898 = EDGE_LOOP ( 'NONE', ( #40289, #42276, #14624, #10653 ) ) ;
#32899 = ADVANCED_FACE ( 'NONE', ( #26348 ), #19253, .T. ) ;
#32900 = DIRECTION ( 'NONE',  ( 0.9266896074318343723, 0.000000000000000000, -0.3758275821142357809 ) ) ;
#32901 = VECTOR ( 'NONE', #33592, 1000.000000000000000 ) ;
#32902 = CARTESIAN_POINT ( 'NONE',  ( 46.00000000000000711, 20.00000000000000000, 41.00000000000000000 ) ) ;
#32903 = CARTESIAN_POINT ( 'NONE',  ( -49.13194886969938580, -175.3837268820161057, 0.7575112421616214675 ) ) ;
#32904 = EDGE_LOOP ( 'NONE', ( #2618, #42567, #6295, #42163 ) ) ;
#32905 = EDGE_CURVE ( 'NONE', #32592, #33172, #29869, .T. ) ;
#32906 = VERTEX_POINT ( 'NONE', #6655 ) ;
#32907 = AXIS2_PLACEMENT_3D ( 'NONE', #49658, #2348, #42795 ) ;
#32908 = FACE_OUTER_BOUND ( 'NONE', #36329, .T. ) ;
#32910 = ORIENTED_EDGE ( 'NONE', *, *, #17309, .T. ) ;
#32909 = DIRECTION ( 'NONE',  ( -0.6965510290629882695, 0.000000000000000000, -0.7175072570443395970 ) ) ;
#32911 = FACE_OUTER_BOUND ( 'NONE', #42295, .T. ) ;
#32912 = ORIENTED_EDGE ( 'NONE', *, *, #38701, .T. ) ;
#32913 = CARTESIAN_POINT ( 'NONE',  ( -63.43218022845228887, -175.3837268820161057, 124.1024020384604540 ) ) ;
#32914 = ORIENTED_EDGE ( 'NONE', *, *, #12121, .F. ) ;
#32915 = DIRECTION ( 'NONE',  ( -0.6068001458186002006, 0.000000000000000000, 0.7948544414133481562 ) ) ;
#32916 = DIRECTION ( 'NONE',  ( 0.000000000000000000, 0.000000000000000000, 1.000000000000000000 ) ) ;
#32917 = DIRECTION ( 'NONE',  ( -0.000000000000000000, 1.000000000000000000, -0.000000000000000000 ) ) ;
#32918 = VECTOR ( 'NONE', #21610, 1000.000000000000000 ) ;
#32919 = CIRCLE ( 'NONE', #11129, 9.999999999999994671 ) ;
#32920 = ORIENTED_EDGE ( 'NONE', *, *, #48824, .T. ) ;
#32921 = VECTOR ( 'NONE', #16218, 1000.000000000000000 ) ;
#32922 = ORIENTED_EDGE ( 'NONE', *, *, #20495, .T. ) ;
#32923 = AXIS2_PLACEMENT_3D ( 'NONE', #5673, #22199, #21942 ) ;
#32924 = PLANE ( 'NONE',  #1321 ) ;
#32925 = CARTESIAN_POINT ( 'NONE',  ( -47.55243714407702527, -183.6283474603465606, 0.3758275821142491591 ) ) ;
#32926 = ORIENTED_EDGE ( 'NONE', *, *, #537, .F. ) ;
#32927 = DIRECTION ( 'NONE',  ( 0.000000000000000000, -1.000000000000000000, 0.000000000000000000 ) ) ;
#32928 = CARTESIAN_POINT ( 'NONE',  ( -336.3521761649654422, -140.1754235130667610, -56.65561927338005432 ) ) ;
#32929 = EDGE_CURVE ( 'NONE', #35901, #15345, #11342, .T. ) ;
#32930 = EDGE_CURVE ( 'NONE', #12684, #22789, #7431, .T. ) ;
#32931 = ORIENTED_EDGE ( 'NONE', *, *, #43639, .T. ) ;
#32932 = PLANE ( 'NONE',  #24206 ) ;
#32933 = LINE ( 'NONE', #29261, #41641 ) ;
#32934 = ORIENTED_EDGE ( 'NONE', *, *, #44071, .T. ) ;
#32935 = DIRECTION ( 'NONE',  ( -0.6965510290630033685, 0.000000000000000000, 0.7175072570443249420 ) ) ;
#32936 = VERTEX_POINT ( 'NONE', #10326 ) ;
#32937 = DIRECTION ( 'NONE',  ( -0.000000000000000000, 1.000000000000000000, -0.000000000000000000 ) ) ;
#32938 = DIRECTION ( 'NONE',  ( 0.000000000000000000, -1.000000000000000000, 0.000000000000000000 ) ) ;
#32939 = ORIENTED_EDGE ( 'NONE', *, *, #44336, .T. ) ;
#32940 = CIRCLE ( 'NONE', #21218, 124.9999999999999858 ) ;
#32941 = CARTESIAN_POINT ( 'NONE',  ( 46.01898237923985846, -177.1207230881787780, -81.82363577055903647 ) ) ;
#32942 = DIRECTION ( 'NONE',  ( 0.000000000000000000, -1.216619397818400625E-13, 1.000000000000000000 ) ) ;
#32943 = LINE ( 'NONE', #9054, #567 ) ;
#32944 = EDGE_CURVE ( 'NONE', #8829, #22651, #38439, .T. ) ;
#32945 = LINE ( 'NONE', #12711, #38342 ) ;
#32946 = EDGE_CURVE ( 'NONE', #44462, #22776, #10577, .T. ) ;
#32947 = VECTOR ( 'NONE', #18175, 1000.000000000000000 ) ;
#32948 = ORIENTED_EDGE ( 'NONE', *, *, #16894, .T. ) ;
#32949 = PLANE ( 'NONE',  #6030 ) ;
#32950 = ORIENTED_EDGE ( 'NONE', *, *, #9758, .F. ) ;
#32951 = ORIENTED_EDGE ( 'NONE', *, *, #48112, .T. ) ;
#32952 = EDGE_CURVE ( 'NONE', #12133, #12684, #18730, .T. ) ;
#32953 = LINE ( 'NONE', #25587, #14294 ) ;
#32955 = ORIENTED_EDGE ( 'NONE', *, *, #11621, .T. ) ;
#32954 = PLANE ( 'NONE',  #22814 ) ;
#32956 = EDGE_CURVE ( 'NONE', #31485, #728, #42472, .T. ) ;
#32957 = ORIENTED_EDGE ( 'NONE', *, *, #23812, .T. ) ;
#32958 = LINE ( 'NONE', #5127, #47525 ) ;
#32959 = VECTOR ( 'NONE', #6806, 1000.000000000000000 ) ;
#32960 = DIRECTION ( 'NONE',  ( 0.000000000000000000, 1.000000000000000000, 0.000000000000000000 ) ) ;
#32961 = LINE ( 'NONE', #2133, #8407 ) ;
#32962 = VECTOR ( 'NONE', #51401, 1000.000000000000000 ) ;
#32963 = AXIS2_PLACEMENT_3D ( 'NONE', #39665, #46816, #23153 ) ;
#32964 = VERTEX_POINT ( 'NONE', #7667 ) ;
#32965 = CARTESIAN_POINT ( 'NONE',  ( -332.3517673607765914, -73.44864141332200802, 31.34948880313848107 ) ) ;
#32966 = ORIENTED_EDGE ( 'NONE', *, *, #50570, .T. ) ;
#32967 = CARTESIAN_POINT ( 'NONE',  ( -165.7578939544008847, -177.1207230881787780, -43.25148278810626579 ) ) ;
#32968 = DIRECTION ( 'NONE',  ( 0.000000000000000000, 0.4647231720437724478, 0.8854560256532078011 ) ) ;
#32969 = VECTOR ( 'NONE', #48817, 1000.000000000000000 ) ;
#32970 = DIRECTION ( 'NONE',  ( 0.000000000000000000, -0.4647231720437724478, -0.8854560256532078011 ) ) ;
#32971 = DIRECTION ( 'NONE',  ( 1.000000000000000000, -7.719741424018524829E-17, -4.051632851310624584E-17 ) ) ;
#32972 = ORIENTED_EDGE ( 'NONE', *, *, #4766, .T. ) ;
#32973 = ORIENTED_EDGE ( 'NONE', *, *, #45549, .F. ) ;
#32974 = ORIENTED_EDGE ( 'NONE', *, *, #46778, .T. ) ;
#32975 = LINE ( 'NONE', #45353, #41696 ) ;
#32976 = CARTESIAN_POINT ( 'NONE',  ( -145.0195698084541505, -189.7472609257535510, 79.40367028273128369 ) ) ;
#32977 = FACE_OUTER_BOUND ( 'NONE', #25114, .T. ) ;
#32978 = CARTESIAN_POINT ( 'NONE',  ( -46.00000000000000711, 20.00000000000000000, 5.000000000000006217 ) ) ;
#32979 = DIRECTION ( 'NONE',  ( 0.000000000000000000, -0.8229838658936613482, -0.5680647467311485954 ) ) ;
#32980 = VECTOR ( 'NONE', #43737, 1000.000000000000000 ) ;
#32981 = VERTEX_POINT ( 'NONE', #20017 ) ;
#32982 = VECTOR ( 'NONE', #25598, 1000.000000000000000 ) ;
#32983 = EDGE_LOOP ( 'NONE', ( #33055, #33782, #45657, #35431 ) ) ;
#32985 = ORIENTED_EDGE ( 'NONE', *, *, #3406, .T. ) ;
#32984 = DIRECTION ( 'NONE',  ( 0.000000000000000000, 0.000000000000000000, 1.000000000000000000 ) ) ;
#32986 = ORIENTED_EDGE ( 'NONE', *, *, #51886, .T. ) ;
#32987 = CARTESIAN_POINT ( 'NONE',  ( -336.3521761649654422, -87.81784868886214213, 47.06073758877343494 ) ) ;
#32988 = EDGE_CURVE ( 'NONE', #44162, #6148, #51561, .T. ) ;
#32989 = FACE_OUTER_BOUND ( 'NONE', #36094, .T. ) ;
#32990 = LINE ( 'NONE', #29316, #39666 ) ;
#32991 = EDGE_CURVE ( 'NONE', #13340, #21757, #31848, .T. ) ;
#32992 = LINE ( 'NONE', #24860, #47244 ) ;
#32993 = ADVANCED_FACE ( 'NONE', ( #15562 ), #32625, .T. ) ;
#32994 = ADVANCED_FACE ( 'NONE', ( #43925 ), #12639, .T. ) ;
#32995 = FACE_OUTER_BOUND ( 'NONE', #49100, .T. ) ;
#32996 = ORIENTED_EDGE ( 'NONE', *, *, #12762, .T. ) ;
#32997 = FACE_OUTER_BOUND ( 'NONE', #24063, .T. ) ;
#32998 = AXIS2_PLACEMENT_3D ( 'NONE', #28152, #25018, #36304 ) ;
#32999 = ORIENTED_EDGE ( 'NONE', *, *, #9582, .F. ) ;
#33000 = EDGE_CURVE ( 'NONE', #2282, #19065, #33250, .T. ) ;
#33001 = VERTEX_POINT ( 'NONE', #47886 ) ;
#33002 = DIRECTION ( 'NONE',  ( 0.7765238627180349740, 0.000000000000000000, 0.6300878435817203194 ) ) ;
#33003 = AXIS2_PLACEMENT_3D ( 'NONE', #35529, #47651, #27391 ) ;
#33004 = PRESENTATION_STYLE_ASSIGNMENT (( #28793 ) ) ;
#33005 = EDGE_CURVE ( 'NONE', #17543, #14548, #48137, .T. ) ;
#33006 = CARTESIAN_POINT ( 'NONE',  ( -336.3521761649654422, -136.0347666902908372, 57.67619951860663718 ) ) ;
#33007 = EDGE_CURVE ( 'NONE', #46248, #33039, #21475, .T. ) ;
#33008 = CARTESIAN_POINT ( 'NONE',  ( -114.1105527140175440, -183.6283474603465606, 106.3838142112217326 ) ) ;
#33009 = DIRECTION ( 'NONE',  ( 0.000000000000000000, 0.000000000000000000, -1.000000000000000000 ) ) ;
#33010 = CARTESIAN_POINT ( 'NONE',  ( -332.3517673607765914, -177.7325358280884586, 23.38292116578760726 ) ) ;
#33011 = AXIS2_PLACEMENT_3D ( 'NONE', #23014, #2526, #3035 ) ;
#33012 = ADVANCED_FACE ( 'NONE', ( #48402 ), #35514, .T. ) ;
#33013 = VERTEX_POINT ( 'NONE', #23693 ) ;
#33014 = PLANE ( 'NONE',  #23011 ) ;
#33015 = DIRECTION ( 'NONE',  ( 0.9929810960135178055, 0.000000000000000000, -0.1182731709213592358 ) ) ;
#33016 = EDGE_CURVE ( 'NONE', #9665, #50565, #23952, .T. ) ;
#33017 = CARTESIAN_POINT ( 'NONE',  ( 68.79964045138289919, -177.1207230881787780, 43.25148278810711133 ) ) ;
#33018 = FACE_BOUND ( 'NONE', #9773, .T. ) ;
#33019 = VERTEX_POINT ( 'NONE', #4249 ) ;
#33020 = EDGE_CURVE ( 'NONE', #6834, #47944, #11439, .T. ) ;
#33021 = CARTESIAN_POINT ( 'NONE',  ( -94.25732089370191602, -177.1207230881787780, 116.3157639405754935 ) ) ;
#33022 = ORIENTED_EDGE ( 'NONE', *, *, #1355, .F. ) ;
#33023 = CIRCLE ( 'NONE', #10370, 60.00000000000000000 ) ;
#33024 = DIRECTION ( 'NONE',  ( 1.000000000000000000, 0.000000000000000000, 0.000000000000000000 ) ) ;
#33025 = EDGE_CURVE ( 'NONE', #26931, #12201, #28144, .T. ) ;
#33026 = ORIENTED_EDGE ( 'NONE', *, *, #47370, .F. ) ;
#33027 = DIRECTION ( 'NONE',  ( -0.3758275821142488260, 0.000000000000000000, 0.9266896074318291543 ) ) ;
#33028 = ORIENTED_EDGE ( 'NONE', *, *, #39410, .F. ) ;
#33029 = ADVANCED_FACE ( 'NONE', ( #24225 ), #27645, .T. ) ;
#33030 = CIRCLE ( 'NONE', #39720, 60.00000000000000000 ) ;
#33031 = CARTESIAN_POINT ( 'NONE',  ( -46.00000000000000711, 20.00000000000000000, 8.673617379884035472E-15 ) ) ;
#33032 = LINE ( 'NONE', #5195, #30965 ) ;
#33034 = ORIENTED_EDGE ( 'NONE', *, *, #12656, .T. ) ;
#33033 = DIRECTION ( 'NONE',  ( -1.000000000000000000, 0.000000000000000000, 0.000000000000000000 ) ) ;
#33036 = AXIS2_PLACEMENT_3D ( 'NONE', #42633, #18978, #42363 ) ;
#33035 = DIRECTION ( 'NONE',  ( -0.000000000000000000, 1.000000000000000000, -0.000000000000000000 ) ) ;
#33037 = EDGE_CURVE ( 'NONE', #43333, #22832, #44457, .T. ) ;
#33038 = VERTEX_POINT ( 'NONE', #24739 ) ;
#33039 = VERTEX_POINT ( 'NONE', #36554 ) ;
#33040 = ORIENTED_EDGE ( 'NONE', *, *, #19845, .T. ) ;
#33041 = FACE_BOUND ( 'NONE', #21613, .T. ) ;
#33042 = FACE_OUTER_BOUND ( 'NONE', #41957, .T. ) ;
#33043 = ORIENTED_EDGE ( 'NONE', *, *, #37236, .F. ) ;
#33044 = DIRECTION ( 'NONE',  ( -0.000000000000000000, 1.000000000000000000, -0.000000000000000000 ) ) ;
#33045 = DIRECTION ( 'NONE',  ( 0.000000000000000000, 0.000000000000000000, 1.000000000000000000 ) ) ;
#33046 = DIRECTION ( 'NONE',  ( 0.000000000000000000, 0.000000000000000000, 1.000000000000000000 ) ) ;
#33047 = EDGE_CURVE ( 'NONE', #26606, #28239, #4773, .T. ) ;
#33048 = DIRECTION ( 'NONE',  ( 0.000000000000000000, -0.8229838658936494689, 0.5680647467311658039 ) ) ;
#33049 = ORIENTED_EDGE ( 'NONE', *, *, #21373, .T. ) ;
#33052 = ORIENTED_EDGE ( 'NONE', *, *, #30168, .F. ) ;
#33051 = DIRECTION ( 'NONE',  ( 0.000000000000000000, -0.9709418174260534551, -0.2393156642875516327 ) ) ;
#33050 = CARTESIAN_POINT ( 'NONE',  ( -171.7589556598192360, -177.1207230881787780, -13.35228579481114863 ) ) ;
#33053 = ORIENTED_EDGE ( 'NONE', *, *, #11956, .F. ) ;
#33054 = CYLINDRICAL_SURFACE ( 'NONE', #49188, 125.0000000000000000 ) ;
#33055 = ORIENTED_EDGE ( 'NONE', *, *, #21703, .F. ) ;
#33056 = LINE ( 'NONE', #9670, #37338 ) ;
#33057 = AXIS2_PLACEMENT_3D ( 'NONE', #29136, #45198, #25720 ) ;
#33058 = ORIENTED_EDGE ( 'NONE', *, *, #3836, .F. ) ;
#33059 = VECTOR ( 'NONE', #10924, 1000.000000000000000 ) ;
#33060 = EDGE_CURVE ( 'NONE', #16046, #9877, #40752, .T. ) ;
#33061 = LINE ( 'NONE', #12825, #20401 ) ;
#33062 = EDGE_CURVE ( 'NONE', #12928, #33549, #33422, .T. ) ;
#33063 = ADVANCED_FACE ( 'NONE', ( #5302 ), #49700, .F. ) ;
#33064 = DIRECTION ( 'NONE',  ( -0.9473263538541946138, 0.000000000000000000, 0.3202698538628279690 ) ) ;
#33065 = ORIENTED_EDGE ( 'NONE', *, *, #20435, .T. ) ;
#33066 = PLANE ( 'NONE',  #45121 ) ;
#33067 = ORIENTED_EDGE ( 'NONE', *, *, #3241, .T. ) ;
#33068 = CIRCLE ( 'NONE', #42281, 125.0000000000000000 ) ;
#33069 = EDGE_CURVE ( 'NONE', #1251, #38255, #1855, .T. ) ;
#33070 = ORIENTED_EDGE ( 'NONE', *, *, #31699, .F. ) ;
#33071 = LINE ( 'NONE', #16807, #6111 ) ;
#33072 = CARTESIAN_POINT ( 'NONE',  ( -332.3517673607765914, -160.6539403396202772, 45.90766452162722544 ) ) ;
#33073 = CARTESIAN_POINT ( 'NONE',  ( -34.63763967761164508, -189.7472609257535510, -123.2250735253142864 ) ) ;
#33074 = CARTESIAN_POINT ( 'NONE',  ( 72.31641062551800303, -193.5000000000000000, 32.14713283941990341 ) ) ;
#33075 = ORIENTED_EDGE ( 'NONE', *, *, #4414, .F. ) ;
#33076 = DIRECTION ( 'NONE',  ( 0.000000000000000000, 1.000000000000000000, -0.000000000000000000 ) ) ;
#33077 = APPLICATION_PROTOCOL_DEFINITION ( 'draft international standard', 'automotive_design', 1998, #38416 ) ;
#33078 = CARTESIAN_POINT ( 'NONE',  ( 42.89728982752369291, -175.3837268820161057, 83.82333043185313670 ) ) ;
#33079 = PLANE ( 'NONE',  #42985 ) ;
#33080 = VECTOR ( 'NONE', #27220, 1000.000000000000114 ) ;
#33081 = FACE_OUTER_BOUND ( 'NONE', #38350, .T. ) ;
#33082 = CARTESIAN_POINT ( 'NONE',  ( 74.49773146996547268, -177.1207230881787780, -22.39848972532282190 ) ) ;
#33083 = LINE ( 'NONE', #28612, #44173 ) ;
#33084 = ORIENTED_EDGE ( 'NONE', *, *, #7394, .T. ) ;
#33085 = VERTEX_POINT ( 'NONE', #1342 ) ;
#33086 = ADVANCED_FACE ( 'NONE', ( #48923 ), #26036, .F. ) ;
#33087 = DIRECTION ( 'NONE',  ( -0.000000000000000000, 1.000000000000000000, -0.000000000000000000 ) ) ;
#33088 = ADVANCED_FACE ( 'NONE', ( #12904 ), #20805, .T. ) ;
#33089 = PLANE ( 'NONE',  #38733 ) ;
#33090 = VERTEX_POINT ( 'NONE', #5043 ) ;
#33091 = ORIENTED_EDGE ( 'NONE', *, *, #29231, .F. ) ;
#33092 = ORIENTED_EDGE ( 'NONE', *, *, #14379, .T. ) ;
#33093 = ADVANCED_FACE ( 'NONE', ( #9241 ), #37077, .T. ) ;
#33094 = DIRECTION ( 'NONE',  ( -0.000000000000000000, 1.000000000000000000, -0.000000000000000000 ) ) ;
#33095 = DIRECTION ( 'NONE',  ( -0.8124868780056783146, 0.000000000000000000, -0.5829794791144762289 ) ) ;
#33096 = CARTESIAN_POINT ( 'NONE',  ( -79.88691714431335811, -193.5000000000000000, 119.9572859573367367 ) ) ;
#33097 = CARTESIAN_POINT ( 'NONE',  ( 27.23560471289044571, -175.3837268820161057, 99.45993886622845537 ) ) ;
#33098 = AXIS2_PLACEMENT_3D ( 'NONE', #21633, #29752, #30026 ) ;
#33099 = ORIENTED_EDGE ( 'NONE', *, *, #44227, .F. ) ;
#33100 = VECTOR ( 'NONE', #22087, 1000.000000000000000 ) ;
#33101 = CARTESIAN_POINT ( 'NONE',  ( 29.27398957514434130, -177.1207230881787780, -97.87467957287998388 ) ) ;
#33102 = DIRECTION ( 'NONE',  ( 0.000000000000000000, 1.000000000000000000, 0.000000000000000000 ) ) ;
#33103 = ORIENTED_EDGE ( 'NONE', *, *, #16293, .F. ) ;
#33104 = VECTOR ( 'NONE', #40049, 1000.000000000000227 ) ;
#33105 = CARTESIAN_POINT ( 'NONE',  ( 69.99104047056317768, -193.5000000000000000, -39.87254040532513244 ) ) ;
#33106 = ORIENTED_EDGE ( 'NONE', *, *, #19483, .F. ) ;
#33107 = FACE_OUTER_BOUND ( 'NONE', #40088, .T. ) ;
#33108 = EDGE_LOOP ( 'NONE', ( #12932, #5715, #6020, #11092 ) ) ;
#33109 = FACE_OUTER_BOUND ( 'NONE', #45598, .T. ) ;
#33110 = AXIS2_PLACEMENT_3D ( 'NONE', #44561, #49028, #679 ) ;
#33111 = CARTESIAN_POINT ( 'NONE',  ( -169.0855799822425638, -177.1207230881787780, -28.81338593823975103 ) ) ;
#33112 = DIRECTION ( 'NONE',  ( -0.000000000000000000, -0.8229838658936596829, -0.5680647467311510379 ) ) ;
#33115 = VERTEX_POINT ( 'NONE', #21320 ) ;
#33114 = LINE ( 'NONE', #28906, #9036 ) ;
#33113 = CARTESIAN_POINT ( 'NONE',  ( -129.4514457347087273, -189.7472609257535510, 95.22858582633115532 ) ) ;
#33116 = SHAPE_REPRESENTATION ( 'Center Pivot Base Stud', ( #31742 ), #3199 ) ;
#33117 = DIRECTION ( 'NONE',  ( 0.000000000000000000, 0.000000000000000000, 1.000000000000000000 ) ) ;
#33118 = VERTEX_POINT ( 'NONE', #37339 ) ;
#33119 = DIRECTION ( 'NONE',  ( 0.000000000000000000, 0.000000000000000000, -1.000000000000000000 ) ) ;
#33120 = DIRECTION ( 'NONE',  ( 1.043714542225393697E-14, 0.8854560256532044704, -0.4647231720437789981 ) ) ;
#33121 = ORIENTED_EDGE ( 'NONE', *, *, #9124, .F. ) ;
#33122 = ADVANCED_FACE ( 'NONE', ( #9752 ), #49959, .T. ) ;
#33123 = ADVANCED_FACE ( 'NONE', ( #825 ), #37615, .F. ) ;
#33124 = CARTESIAN_POINT ( 'NONE',  ( -47.74129347246712740, -193.5000000000000000, -0.6749830015182022303 ) ) ;
#33126 = DIRECTION ( 'NONE',  ( -0.000000000000000000, 0.4647231720437664526, -0.8854560256532110207 ) ) ;
#33125 = CARTESIAN_POINT ( 'NONE',  ( -336.3521761649654422, -178.0871407151310279, 22.44790492310219676 ) ) ;
#33127 = ORIENTED_EDGE ( 'NONE', *, *, #6044, .F. ) ;
#33128 = DIRECTION ( 'NONE',  ( 0.000000000000000000, 0.000000000000000000, 1.000000000000000000 ) ) ;
#33129 = CARTESIAN_POINT ( 'NONE',  ( -69.59623518921151231, -189.7472609257535510, 122.1886788576023974 ) ) ;
#33130 = AXIS2_PLACEMENT_3D ( 'NONE', #4444, #9174, #17065 ) ;
#33131 = CARTESIAN_POINT ( 'NONE',  ( 76.37123734610607073, -183.6283474603465606, 6.114457023561872262 ) ) ;
#33132 = EDGE_LOOP ( 'NONE', ( #51816, #24183, #13246, #46991 ) ) ;
#33133 = SURFACE_STYLE_USAGE ( .BOTH. , #36043 ) ;
#33134 =( NAMED_UNIT ( * ) PLANE_ANGLE_UNIT ( ) SI_UNIT ( $, .RADIAN. ) );
#33135 = PLANE ( 'NONE',  #47792 ) ;
#33136 = VECTOR ( 'NONE', #45485, 1000.000000000000000 ) ;
#33137 = CARTESIAN_POINT ( 'NONE',  ( 35.45604639379469347, -183.6283474603465606, 91.27439114664649367 ) ) ;
#33138 = VECTOR ( 'NONE', #47902, 1000.000000000000114 ) ;
#33139 = ORIENTED_EDGE ( 'NONE', *, *, #34439, .F. ) ;
#33140 = CARTESIAN_POINT ( 'NONE',  ( -45.06671089634843952, -193.5000000000000000, -124.9534129907280402 ) ) ;
#33142 = VECTOR ( 'NONE', #27658, 999.9999999999998863 ) ;
#33141 = CYLINDRICAL_SURFACE ( 'NONE', #22292, 25.00456841203573077 ) ;
#33143 = CARTESIAN_POINT ( 'NONE',  ( -172.7479958471413966, -183.6283474603465606, -13.49993235881363418 ) ) ;
#33144 = EDGE_LOOP ( 'NONE', ( #42617, #27833, #35586, #33774 ) ) ;
#33145 = DIRECTION ( 'NONE',  ( 0.000000000000000000, 0.000000000000000000, -1.000000000000000000 ) ) ;
#33146 = CARTESIAN_POINT ( 'NONE',  ( -166.9492939735806090, -175.3837268820161057, 39.87254040532603483 ) ) ;
#33148 = EDGE_CURVE ( 'NONE', #34248, #51567, #10633, .T. ) ;
#33147 = AXIS2_PLACEMENT_3D ( 'NONE', #35180, #15485, #34664 ) ;
#33149 = AXIS2_PLACEMENT_3D ( 'NONE', #49013, #44297, #16441 ) ;
#33150 = CARTESIAN_POINT ( 'NONE',  ( 6.443011874827243801, -183.6283474603465606, 112.2878385610370771 ) ) ;
#33151 = DIRECTION ( 'NONE',  ( 0.6068001458186002006, 0.000000000000000000, -0.7948544414133481562 ) ) ;
#33152 = VECTOR ( 'NONE', #28452, 1000.000000000000000 ) ;
#33153 = EDGE_CURVE ( 'NONE', #22526, #13663, #41277, .T. ) ;
#33154 = CARTESIAN_POINT ( 'NONE',  ( -47.53180039765466347, -175.3837268820161057, 0.3202698538628485636 ) ) ;
#33155 = DIRECTION ( 'NONE',  ( 0.000000000000000000, 1.000000000000000000, 0.000000000000000000 ) ) ;
#33156 = LINE ( 'NONE', #33681, #27878 ) ;
#33158 = ORIENTED_EDGE ( 'NONE', *, *, #47286, .T. ) ;
#33157 = LINE ( 'NONE', #2409, #9422 ) ;
#33159 = VERTEX_POINT ( 'NONE', #25515 ) ;
#33160 = CARTESIAN_POINT ( 'NONE',  ( -92.16375985330356002, -175.3837268820161057, 117.1181148702521710 ) ) ;
#33161 = DIRECTION ( 'NONE',  ( 0.000000000000000000, -1.000000000000000000, -0.000000000000000000 ) ) ;
#33163 = ORIENTED_EDGE ( 'NONE', *, *, #14637, .T. ) ;
#33162 = CYLINDRICAL_SURFACE ( 'NONE', #10242, 124.9999999999999858 ) ;
#33164 = VERTEX_POINT ( 'NONE', #41024 ) ;
#33165 = VECTOR ( 'NONE', #7160, 1000.000000000000000 ) ;
#33166 = VERTEX_POINT ( 'NONE', #33137 ) ;
#33167 = DIRECTION ( 'NONE',  ( 0.000000000000000000, 1.000000000000000000, 0.000000000000000000 ) ) ;
#33168 = VECTOR ( 'NONE', #9415, 1000.000000000000114 ) ;
#33169 = CIRCLE ( 'NONE', #19732, 125.0000000000000000 ) ;
#33170 = DIRECTION ( 'NONE',  ( -0.000000000000000000, -0.2393156642875615969, -0.9709418174260511236 ) ) ;
#33171 = CYLINDRICAL_SURFACE ( 'NONE', #22437, 125.0000000000000000 ) ;
#33172 = VERTEX_POINT ( 'NONE', #29980 ) ;
#33173 = VECTOR ( 'NONE', #49588, 1000.000000000000000 ) ;
#33174 = EDGE_CURVE ( 'NONE', #48781, #44562, #28251, .T. ) ;
#33175 = CYLINDRICAL_SURFACE ( 'NONE', #37799, 125.0000000000000000 ) ;
#33177 = ORIENTED_EDGE ( 'NONE', *, *, #12696, .T. ) ;
#33176 = LINE ( 'NONE', #49226, #18271 ) ;
#33178 = AXIS2_PLACEMENT_3D ( 'NONE', #28273, #16459, #44564 ) ;
#33179 = AXIS2_PLACEMENT_3D ( 'NONE', #2602, #5798, #2355 ) ;
#33180 = LINE ( 'NONE', #41063, #50759 ) ;
#33181 = EDGE_LOOP ( 'NONE', ( #24151, #581, #27111, #18070 ) ) ;
#33182 = DIRECTION ( 'NONE',  ( 0.000000000000000000, 1.000000000000000000, 0.000000000000000000 ) ) ;
#33183 = EDGE_LOOP ( 'NONE', ( #45404, #49537, #22421, #45055 ) ) ;
#33184 = EDGE_CURVE ( 'NONE', #27201, #20956, #17400, .T. ) ;
#33185 = CARTESIAN_POINT ( 'NONE',  ( 59.80284513346456521, -177.1207230881787780, 62.45009659481583242 ) ) ;
#33186 = VECTOR ( 'NONE', #29693, 1000.000000000000000 ) ;
#33187 = CARTESIAN_POINT ( 'NONE',  ( 74.18685885783123979, -189.7472609257535510, -18.13990644964003707 ) ) ;
#33188 = DIRECTION ( 'NONE',  ( 0.8455960035018234011, 0.000000000000000000, 0.5338233779647948429 ) ) ;
#33189 = CIRCLE ( 'NONE', #10536, 4.000000000000003553 ) ;
#33190 = ORIENTED_EDGE ( 'NONE', *, *, #38328, .F. ) ;
#33191 = EDGE_CURVE ( 'NONE', #39306, #5601, #5563, .T. ) ;
#33192 = EDGE_LOOP ( 'NONE', ( #51555, #32128, #17133, #8533 ) ) ;
#33193 = DIRECTION ( 'NONE',  ( 0.000000000000000000, 0.000000000000000000, -1.000000000000000000 ) ) ;
#33194 = CARTESIAN_POINT ( 'NONE',  ( 26.52087324849106054, -198.5000000000000000, -80.00000000000002842 ) ) ;
#33195 = EDGE_LOOP ( 'NONE', ( #30665, #14764, #38694, #18000 ) ) ;
#33196 = FACE_OUTER_BOUND ( 'NONE', #40026, .T. ) ;
#33197 = DIRECTION ( 'NONE',  ( 0.000000000000000000, 0.000000000000000000, 1.000000000000000000 ) ) ;
#33198 = ORIENTED_EDGE ( 'NONE', *, *, #41666, .T. ) ;
#33199 = CARTESIAN_POINT ( 'NONE',  ( 62.13187335169531167, -177.1207230881787780, -58.22548115875872554 ) ) ;
#33200 = CARTESIAN_POINT ( 'NONE',  ( -332.3517673607765914, -75.87119766449505676, -34.85916744524372746 ) ) ;
#33201 = ORIENTED_EDGE ( 'NONE', *, *, #21971, .F. ) ;
#33202 = FACE_OUTER_BOUND ( 'NONE', #13944, .T. ) ;
#33203 = EDGE_LOOP ( 'NONE', ( #49681, #31517, #11260, #39079 ) ) ;
#33204 = AXIS2_PLACEMENT_3D ( 'NONE', #17337, #33356, #37024 ) ;
#33205 = PLANE ( 'NONE',  #23705 ) ;
#33206 = LINE ( 'NONE', #25330, #50529 ) ;
#33207 = ADVANCED_FACE ( 'NONE', ( #29711 ), #45756, .F. ) ;
#33208 = VERTEX_POINT ( 'NONE', #26283 ) ;
#33209 = AXIS2_PLACEMENT_3D ( 'NONE', #12173, #20862, #44507 ) ;
#33210 = AXIS2_PLACEMENT_3D ( 'NONE', #16873, #40242, #31857 ) ;
#33211 = CARTESIAN_POINT ( 'NONE',  ( 59.00260725618641544, -183.6283474603465606, -63.81752780152991278 ) ) ;
#33212 = LINE ( 'NONE', #36642, #27202 ) ;
#33213 = CYLINDRICAL_SURFACE ( 'NONE', #16526, 125.0000000000000000 ) ;
#33214 = CARTESIAN_POINT ( 'NONE',  ( -330.4913330509368166, -123.5000000000000284, 0.000000000000000000 ) ) ;
#33215 = EDGE_LOOP ( 'NONE', ( #3961, #42923, #18706, #42802 ) ) ;
#33216 = CARTESIAN_POINT ( 'NONE',  ( -330.4913330509368166, -116.7644047441735182, -59.62073260661671270 ) ) ;
#33217 = VERTEX_POINT ( 'NONE', #30242 ) ;
#33218 = ORIENTED_EDGE ( 'NONE', *, *, #11714, .F. ) ;
#33219 = VECTOR ( 'NONE', #2240, 1000.000000000000000 ) ;
#33220 = PLANE ( 'NONE',  #36942 ) ;
#33222 = ORIENTED_EDGE ( 'NONE', *, *, #48615, .F. ) ;
#33221 = PLANE ( 'NONE',  #28752 ) ;
#33223 = AXIS2_PLACEMENT_3D ( 'NONE', #24294, #35338, #51390 ) ;
#33224 = EDGE_LOOP ( 'NONE', ( #4327, #19887, #28409, #5107 ) ) ;
#33225 = LINE ( 'NONE', #40844, #45877 ) ;
#33226 = VECTOR ( 'NONE', #45247, 1000.000000000000114 ) ;
#33227 = VECTOR ( 'NONE', #745, 1000.000000000000000 ) ;
#33228 = FACE_BOUND ( 'NONE', #20123, .T. ) ;
#33229 = LINE ( 'NONE', #50251, #35224 ) ;
#33230 = ORIENTED_EDGE ( 'NONE', *, *, #26665, .T. ) ;
#33231 = DIRECTION ( 'NONE',  ( 1.000000000000000000, -0.000000000000000000, -0.000000000000000000 ) ) ;
#33232 = ORIENTED_EDGE ( 'NONE', *, *, #42848, .F. ) ;
#33233 = CARTESIAN_POINT ( 'NONE',  ( -48.47912675150885065, -177.1207230881787780, 6.938893903907228378E-15 ) ) ;
#33234 = LINE ( 'NONE', #41632, #24180 ) ;
#33235 = ADVANCED_FACE ( 'NONE', ( #38379 ), #51258, .T. ) ;
#33236 = CARTESIAN_POINT ( 'NONE',  ( -32.87124591993210743, -189.7472609257535510, 124.0217483183788119 ) ) ;
#33237 = CYLINDRICAL_SURFACE ( 'NONE', #13992, 125.0000000000000000 ) ;
#33238 = ORIENTED_EDGE ( 'NONE', *, *, #41691, .F. ) ;
#33239 = ORIENTED_EDGE ( 'NONE', *, *, #27742, .F. ) ;
#33240 = ORIENTED_EDGE ( 'NONE', *, *, #27299, .F. ) ;
#33241 = EDGE_CURVE ( 'NONE', #45545, #32138, #34939, .T. ) ;
#33242 = DIRECTION ( 'NONE',  ( 0.000000000000000000, 0.000000000000000000, -1.000000000000000000 ) ) ;
#33243 = FACE_OUTER_BOUND ( 'NONE', #14790, .T. ) ;
#33244 = CONICAL_SURFACE ( 'NONE', #40846, 14.00000000000001066, 0.7853981633974491672 ) ;
#33245 = VECTOR ( 'NONE', #35925, 1000.000000000000000 ) ;
#33246 = CIRCLE ( 'NONE', #40774, 60.00000000000000000 ) ;
#33247 = DIRECTION ( 'NONE',  ( -0.000000000000000000, 1.000000000000000000, -0.000000000000000000 ) ) ;
#33248 = CARTESIAN_POINT ( 'NONE',  ( -117.0614752283615161, -189.7472609257535510, 103.3076327631967786 ) ) ;
#33249 = EDGE_LOOP ( 'NONE', ( #8383, #11181, #25043, #31543 ) ) ;
#33250 = CIRCLE ( 'NONE', #39940, 125.0000000000000000 ) ;
#33251 = EDGE_CURVE ( 'NONE', #27409, #15990, #2112, .T. ) ;
#33252 = ADVANCED_FACE ( 'NONE', ( #38888 ), #50483, .T. ) ;
#33253 = EDGE_CURVE ( 'NONE', #15864, #10230, #18420, .T. ) ;
#33254 = ORIENTED_EDGE ( 'NONE', *, *, #14163, .T. ) ;
#33256 = ORIENTED_EDGE ( 'NONE', *, *, #49818, .T. ) ;
#33255 = CARTESIAN_POINT ( 'NONE',  ( -152.3176060415594861, -193.5000000000000000, -69.58857822034967455 ) ) ;
#33257 = CARTESIAN_POINT ( 'NONE',  ( -154.0877180371535928, -175.3837268820161057, -66.87170886601927577 ) ) ;
#33258 = EDGE_LOOP ( 'NONE', ( #16267, #43069, #15797, #34714 ) ) ;
#33259 = ADVANCED_FACE ( 'NONE', ( #42308 ), #30743, .T. ) ;
#33260 = DIRECTION ( 'NONE',  ( -0.9929810960135185827, 0.000000000000000000, 0.1182731709213523247 ) ) ;
#33261 = AXIS2_PLACEMENT_3D ( 'NONE', #29538, #12984, #12724 ) ;
#33262 = DIRECTION ( 'NONE',  ( 1.000000000000000000, -0.000000000000000000, 0.000000000000000000 ) ) ;
#33263 = VECTOR ( 'NONE', #46232, 1000.000000000000000 ) ;
#33264 = AXIS2_PLACEMENT_3D ( 'NONE', #29708, #22348, #25261 ) ;
#33265 = DIRECTION ( 'NONE',  ( -1.000000000000000000, 0.000000000000000000, 0.000000000000000000 ) ) ;
#33266 = CARTESIAN_POINT ( 'NONE',  ( -10.02015192278479816, -183.6283474603465606, -117.8859915627474493 ) ) ;
#33267 = CARTESIAN_POINT ( 'NONE',  ( -49.03777351731249468, -193.5000000000000000, -0.8294056854502022125 ) ) ;
#33268 = ORIENTED_EDGE ( 'NONE', *, *, #44624, .F. ) ;
#33269 = DIRECTION ( 'NONE',  ( -0.000000000000000000, 1.000000000000000000, -0.000000000000000000 ) ) ;
#33270 = AXIS2_PLACEMENT_3D ( 'NONE', #7093, #3397, #39639 ) ;
#33271 = VERTEX_POINT ( 'NONE', #3154 ) ;
#33272 = AXIS2_PLACEMENT_3D ( 'NONE', #4832, #32917, #48971 ) ;
#33273 = ORIENTED_EDGE ( 'NONE', *, *, #32905, .T. ) ;
#33274 = DIRECTION ( 'NONE',  ( 0.4031234292879600778, 0.000000000000000000, 0.9151456172430237901 ) ) ;
#33275 = LINE ( 'NONE', #703, #34524 ) ;
#33276 = ORIENTED_EDGE ( 'NONE', *, *, #5095, .T. ) ;
#33277 = CARTESIAN_POINT ( 'NONE',  ( 75.95066919219054569, -189.7472609257535510, -11.92584929509535385 ) ) ;
#33278 = CARTESIAN_POINT ( 'NONE',  ( -49.25565061422690150, -177.1207230881787780, 0.6300878435817109935 ) ) ;
#33279 = CARTESIAN_POINT ( 'NONE',  ( -134.9506378406916554, -175.3837268820161057, 90.26448786734091811 ) ) ;
#33280 = CARTESIAN_POINT ( 'NONE',  ( -68.09401750944518028, -177.1207230881787780, -122.4396006697294581 ) ) ;
#33281 = DIRECTION ( 'NONE',  ( 0.000000000000000000, -1.000000000000000000, 0.000000000000000000 ) ) ;
#33282 = CARTESIAN_POINT ( 'NONE',  ( -305.0000000000000568, -123.9999999999993747, 59.99791663049644086 ) ) ;
#33283 = CARTESIAN_POINT ( 'NONE',  ( 46.00000000000000711, -42.50000000000000000, -46.00000000000000000 ) ) ;
#33284 = EDGE_LOOP ( 'NONE', ( #6417, #1237, #24566, #17084 ) ) ;
#33285 = AXIS2_PLACEMENT_3D ( 'NONE', #6851, #34952, #23146 ) ;
#33286 = AXIS2_PLACEMENT_3D ( 'NONE', #20819, #31862, #32110 ) ;
#33287 = CARTESIAN_POINT ( 'NONE',  ( -305.0000000000000568, -82.50558083279611310, 43.81161486573607533 ) ) ;
#33288 = ORIENTED_EDGE ( 'NONE', *, *, #8570, .F. ) ;
#33289 = AXIS2_PLACEMENT_3D ( 'NONE', #12384, #40233, #20270 ) ;
#33290 = DIRECTION ( 'NONE',  ( -0.000000000000000000, 1.000000000000000000, -0.000000000000000000 ) ) ;
#33291 = ORIENTED_EDGE ( 'NONE', *, *, #3178, .F. ) ;
#33292 = PLANE ( 'NONE',  #48968 ) ;
#33293 = ORIENTED_EDGE ( 'NONE', *, *, #33153, .T. ) ;
#33294 = CARTESIAN_POINT ( 'NONE',  ( -48.47912675150885065, -189.7472609257535510, 6.938893903907228378E-15 ) ) ;
#33295 = VECTOR ( 'NONE', #47107, 1000.000000000000000 ) ;
#33296 = CARTESIAN_POINT ( 'NONE',  ( 21.21056010634072564, -175.3837268820161057, 103.7706487676302061 ) ) ;
#33297 = AXIS2_PLACEMENT_3D ( 'NONE', #31365, #39505, #11133 ) ;
#33299 = EDGE_LOOP ( 'NONE', ( #34824, #11957, #22927, #15168 ) ) ;
#33298 = CARTESIAN_POINT ( 'NONE',  ( 0.000000000000000000, -157.0158200571384555, -48.55604808772557845 ) ) ;
#33300 = VECTOR ( 'NONE', #16131, 1000.000000000000000 ) ;
#33301 = ADVANCED_FACE ( 'NONE', ( #10512 ), #46796, .T. ) ;
#33302 = EDGE_CURVE ( 'NONE', #42355, #5112, #42582, .T. ) ;
#33303 = EDGE_CURVE ( 'NONE', #35003, #5877, #14223, .T. ) ;
#33304 = AXIS2_PLACEMENT_3D ( 'NONE', #34777, #2221, #14840 ) ;
#33305 = DIRECTION ( 'NONE',  ( 0.000000000000000000, -0.000000000000000000, 1.000000000000000000 ) ) ;
#33306 = ORIENTED_EDGE ( 'NONE', *, *, #41392, .T. ) ;
#33307 = ORIENTED_EDGE ( 'NONE', *, *, #2039, .F. ) ;
#33308 = ORIENTED_EDGE ( 'NONE', *, *, #49284, .T. ) ;
#33309 = CIRCLE ( 'NONE', #49300, 125.0000000000000000 ) ;
#33310 = DIRECTION ( 'NONE',  ( 0.9564009842765244240, 0.000000000000000000, -0.2920567706369695538 ) ) ;
#33311 = DIRECTION ( 'NONE',  ( 0.000000000000000000, 0.000000000000000000, -1.000000000000000000 ) ) ;
#33312 = EDGE_LOOP ( 'NONE', ( #35570, #30916, #51783, #19192 ) ) ;
#33313 = CARTESIAN_POINT ( 'NONE',  ( -145.4373324222573842, -189.7472609257535510, -78.89300572996837957 ) ) ;
#33314 = ADVANCED_FACE ( 'NONE', ( #34183, #6599 ), #2891, .F. ) ;
#33315 = LINE ( 'NONE', #4678, #36231 ) ;
#33316 = CARTESIAN_POINT ( 'NONE',  ( -166.6265240196292439, -189.7472609257535510, 40.81902153125349741 ) ) ;
#33317 = EDGE_LOOP ( 'NONE', ( #35969, #33099, #12403, #46096 ) ) ;
#33318 = EDGE_CURVE ( 'NONE', #34006, #46012, #24066, .T. ) ;
#33319 = ADVANCED_FACE ( 'NONE', ( #15001 ), #31007, .T. ) ;
#33320 = DIRECTION ( 'NONE',  ( -0.000000000000000000, -0.6631226582407911962, 0.7485107481711046340 ) ) ;
#33321 = LINE ( 'NONE', #21492, #51661 ) ;
#33322 = ORIENTED_EDGE ( 'NONE', *, *, #51421, .T. ) ;
#33325 = ORIENTED_EDGE ( 'NONE', *, *, #43430, .F. ) ;
#33324 = CARTESIAN_POINT ( 'NONE',  ( -336.3521761649654422, -113.7752393642576720, 58.25253621232167944 ) ) ;
#33323 = FACE_OUTER_BOUND ( 'NONE', #27914, .T. ) ;
#33326 = CIRCLE ( 'NONE', #35826, 125.0000000000000000 ) ;
#33327 = ORIENTED_EDGE ( 'NONE', *, *, #23639, .F. ) ;
#33328 = VECTOR ( 'NONE', #48936, 999.9999999999998863 ) ;
#33329 = EDGE_CURVE ( 'NONE', #27048, #36669, #11025, .T. ) ;
#33330 = VERTEX_POINT ( 'NONE', #7101 ) ;
#33331 = PLANE ( 'NONE',  #41532 ) ;
#33332 = EDGE_LOOP ( 'NONE', ( #36127, #46238, #8144, #38963 ) ) ;
#33333 = AXIS2_PLACEMENT_3D ( 'NONE', #5854, #36587, #49209 ) ;
#33334 = EDGE_CURVE ( 'NONE', #23304, #13064, #23132, .T. ) ;
#33335 = DIRECTION ( 'NONE',  ( -0.4566292373937140270, 0.000000000000000000, 0.8896570909947467687 ) ) ;
#33336 = LINE ( 'NONE', #20454, #25064 ) ;
#33337 = ORIENTED_EDGE ( 'NONE', *, *, #50112, .T. ) ;
#33338 = DIRECTION ( 'NONE',  ( -0.4031234292879600778, 0.000000000000000000, -0.9151456172430237901 ) ) ;
#33339 = ORIENTED_EDGE ( 'NONE', *, *, #15984, .F. ) ;
#33340 = EDGE_LOOP ( 'NONE', ( #14404, #4281, #34648, #28828 ) ) ;
#33341 = DIRECTION ( 'NONE',  ( -0.000000000000000000, 1.000000000000000000, -0.000000000000000000 ) ) ;
#33342 = AXIS2_PLACEMENT_3D ( 'NONE', #46381, #14845, #15104 ) ;
#33343 = CARTESIAN_POINT ( 'NONE',  ( -332.3517673607765914, -123.5000000000000284, 0.000000000000000000 ) ) ;
#33344 = AXIS2_PLACEMENT_3D ( 'NONE', #25055, #41061, #5078 ) ;
#33345 = DIRECTION ( 'NONE',  ( -0.000000000000000000, 1.000000000000000000, -0.000000000000000000 ) ) ;
#33346 = ORIENTED_EDGE ( 'NONE', *, *, #51534, .T. ) ;
#33347 = AXIS2_PLACEMENT_3D ( 'NONE', #40222, #24459, #8431 ) ;
#33348 = DIRECTION ( 'NONE',  ( 0.8980129913408357867, -0.4399689391117104220, 0.000000000000000000 ) ) ;
#33349 = DIRECTION ( 'NONE',  ( 0.000000000000000000, 0.000000000000000000, -1.000000000000000000 ) ) ;
#33350 =( NAMED_UNIT ( * ) PLANE_ANGLE_UNIT ( ) SI_UNIT ( $, .RADIAN. ) );
#33351 = DIRECTION ( 'NONE',  ( 1.000000000000000000, -0.000000000000000000, -0.000000000000000000 ) ) ;
#33352 = FACE_OUTER_BOUND ( 'NONE', #31895, .T. ) ;
#33353 = VECTOR ( 'NONE', #23991, 1000.000000000000227 ) ;
#33354 = CARTESIAN_POINT ( 'NONE',  ( -332.3517673607765914, -67.40061919120938683, 18.46045550523129819 ) ) ;
#33355 = ADVANCED_FACE ( 'NONE', ( #35203 ), #47311, .T. ) ;
#33356 = DIRECTION ( 'NONE',  ( 0.000000000000000000, 1.000000000000000000, 0.000000000000000000 ) ) ;
#33357 = AXIS2_PLACEMENT_3D ( 'NONE', #38419, #18455, #22137 ) ;
#33358 = DIRECTION ( 'NONE',  ( -0.000000000000000000, 1.000000000000000000, -0.000000000000000000 ) ) ;
#33359 = EDGE_LOOP ( 'NONE', ( #45374, #11690, #19667, #64 ) ) ;
#33360 = DIRECTION ( 'NONE',  ( -0.000000000000000000, 0.000000000000000000, -1.000000000000000000 ) ) ;
#33361 = DIRECTION ( 'NONE',  ( 0.000000000000000000, -0.000000000000000000, -1.000000000000000000 ) ) ;
#33362 = ORIENTED_EDGE ( 'NONE', *, *, #5746, .F. ) ;
#33363 = CARTESIAN_POINT ( 'NONE',  ( 76.48781641346532467, -193.5000000000000000, 2.874563619424060246 ) ) ;
#33364 = VERTEX_POINT ( 'NONE', #25947 ) ;
#33365 = ADVANCED_FACE ( 'NONE', ( #38023 ), #45943, .T. ) ;
#33366 = AXIS2_PLACEMENT_3D ( 'NONE', #24724, #10179, #26198 ) ;
#33367 = CARTESIAN_POINT ( 'NONE',  ( -17.07133635870349408, -183.6283474603465606, -119.9572859573364809 ) ) ;
#33368 = AXIS2_PLACEMENT_3D ( 'NONE', #24163, #35979, #32021 ) ;
#33369 = DIRECTION ( 'NONE',  ( -1.000000000000000000, 0.000000000000000000, 0.000000000000000000 ) ) ;
#33370 = CARTESIAN_POINT ( 'NONE',  ( -339.1964088526558498, -68.15673923803930734, -20.45418021416698551 ) ) ;
#33371 = LINE ( 'NONE', #25994, #5306 ) ;
#33372 = AXIS2_PLACEMENT_3D ( 'NONE', #28889, #41237, #1301 ) ;
#33373 = ORIENTED_EDGE ( 'NONE', *, *, #2516, .F. ) ;
#33374 = EDGE_CURVE ( 'NONE', #8761, #48687, #34923, .T. ) ;
#33375 = EDGE_CURVE ( 'NONE', #18747, #11111, #41969, .T. ) ;
#33376 = EDGE_CURVE ( 'NONE', #30289, #44345, #51756, .T. ) ;
#33377 = EDGE_CURVE ( 'NONE', #16002, #51805, #38555, .T. ) ;
#33378 = CARTESIAN_POINT ( 'NONE',  ( -24.23284180386169240, -177.1207230881787780, -121.6072260099953439 ) ) ;
#33379 = ORIENTED_EDGE ( 'NONE', *, *, #13723, .F. ) ;
#33380 = EDGE_CURVE ( 'NONE', #48966, #42243, #32418, .T. ) ;
#33381 = CARTESIAN_POINT ( 'NONE',  ( -330.4913330509368166, -176.8578783931340581, -27.43969411971497152 ) ) ;
#33382 = ORIENTED_EDGE ( 'NONE', *, *, #6550, .T. ) ;
#33383 = DIRECTION ( 'NONE',  ( -8.718379230999707126E-17, 0.8229838658936575735, 0.5680647467311540355 ) ) ;
#33384 = CIRCLE ( 'NONE', #38433, 125.0000000000000000 ) ;
#33385 = VECTOR ( 'NONE', #32601, 1000.000000000000000 ) ;
#33386 = VERTEX_POINT ( 'NONE', #6238 ) ;
#33387 = ADVANCED_FACE ( 'NONE', ( #29887 ), #10695, .T. ) ;
#33388 = CARTESIAN_POINT ( 'NONE',  ( 12.12533326292403935, -177.1207230881787780, 109.3256576763158847 ) ) ;
#33389 = CIRCLE ( 'NONE', #42602, 60.00000000000000000 ) ;
#33390 = ORIENTED_EDGE ( 'NONE', *, *, #41256, .T. ) ;
#33391 = AXIS2_PLACEMENT_3D ( 'NONE', #24416, #8900, #20464 ) ;
#33392 = EDGE_CURVE ( 'NONE', #31250, #4273, #46196, .T. ) ;
#33393 = ADVANCED_FACE ( 'NONE', ( #38285 ), #26193, .T. ) ;
#33394 = AXIS2_PLACEMENT_3D ( 'NONE', #50459, #6820, #18647 ) ;
#33395 = DIRECTION ( 'NONE',  ( -0.000000000000000000, 1.000000000000000000, -0.000000000000000000 ) ) ;
#33396 = ORIENTED_EDGE ( 'NONE', *, *, #22494, .T. ) ;
#33399 = VERTEX_POINT ( 'NONE', #38794 ) ;
#33398 = DIRECTION ( 'NONE',  ( -0.000000000000000000, 1.000000000000000000, -0.000000000000000000 ) ) ;
#33397 = PLANE ( 'NONE',  #3187 ) ;
#33400 = EDGE_CURVE ( 'NONE', #48052, #32649, #34355, .T. ) ;
#33401 = DIRECTION ( 'NONE',  ( 0.000000000000000000, 1.000000000000000000, -0.000000000000000000 ) ) ;
#33402 = VERTEX_POINT ( 'NONE', #10951 ) ;
#33403 = CARTESIAN_POINT ( 'NONE',  ( 24.63024857337166296, -177.1207230881787780, 101.3904297239426597 ) ) ;
#33404 = VERTEX_POINT ( 'NONE', #50646 ) ;
#33405 = ADVANCED_FACE ( 'NONE', ( #2301 ), #18338, .F. ) ;
#33406 = CARTESIAN_POINT ( 'NONE',  ( -339.1964088526558498, -95.63860483659040312, 52.00954392751717847 ) ) ;
#33409 = EDGE_LOOP ( 'NONE', ( #49215, #26199, #620, #21837 ) ) ;
#33408 = CARTESIAN_POINT ( 'NONE',  ( -163.6979789053106629, -189.7472609257535510, -45.83253885719557985 ) ) ;
#33407 = CARTESIAN_POINT ( 'NONE',  ( -95.37971604807246706, -177.1207230881787780, -114.7887733785763942 ) ) ;
#33410 = ORIENTED_EDGE ( 'NONE', *, *, #921, .T. ) ;
#33411 = ADVANCED_FACE ( 'NONE', ( #14915 ), #14383, .F. ) ;
#33412 = DIRECTION ( 'NONE',  ( 0.000000000000000000, 1.000000000000000000, 0.000000000000000000 ) ) ;
#33413 = CIRCLE ( 'NONE', #10737, 125.0000000000000000 ) ;
#33414 = LINE ( 'NONE', #41807, #35417 ) ;
#33415 = VECTOR ( 'NONE', #7794, 1000.000000000000000 ) ;
#33416 = LINE ( 'NONE', #44981, #31514 ) ;
#33417 = VERTEX_POINT ( 'NONE', #34852 ) ;
#33418 = FACE_OUTER_BOUND ( 'NONE', #50862, .T. ) ;
#33419 =( LENGTH_UNIT ( ) NAMED_UNIT ( * ) SI_UNIT ( .MILLI., .METRE. ) );
#33420 = DIRECTION ( 'NONE',  ( -0.000000000000000000, 1.000000000000000000, -0.000000000000000000 ) ) ;
#33421 = CONICAL_SURFACE ( 'NONE', #1516, 25.00456841203573077, 0.5765357807043077765 ) ;
#33422 = LINE ( 'NONE', #13181, #49244 ) ;
#33423 = ORIENTED_EDGE ( 'NONE', *, *, #23322, .F. ) ;
#33424 = DIRECTION ( 'NONE',  ( -1.000000000000000000, 0.000000000000000000, 0.000000000000000000 ) ) ;
#33425 = EDGE_CURVE ( 'NONE', #16252, #31640, #3920, .T. ) ;
#33426 = CARTESIAN_POINT ( 'NONE',  ( -330.4913330509368166, -123.5000000000000284, 0.000000000000000000 ) ) ;
#33427 = EDGE_CURVE ( 'NONE', #32311, #46014, #43009, .T. ) ;
#33428 = DIRECTION ( 'NONE',  ( 0.2635871660690581320, 0.000000000000000000, 0.9646355819083614058 ) ) ;
#33429 = VERTEX_POINT ( 'NONE', #2803 ) ;
#33430 = DIRECTION ( 'NONE',  ( 0.000000000000000000, 0.000000000000000000, 1.000000000000000000 ) ) ;
#33431 = CARTESIAN_POINT ( 'NONE',  ( -49.32472275501067571, -189.7472609257535510, -0.5338233779647935107 ) ) ;
#33432 = DIRECTION ( 'NONE',  ( 0.000000000000000000, 0.000000000000000000, -1.000000000000000000 ) ) ;
#33433 = DIRECTION ( 'NONE',  ( 0.000000000000000000, 0.000000000000000000, 1.000000000000000000 ) ) ;
#33435 = VECTOR ( 'NONE', #30217, 999.9999999999998863 ) ;
#33434 = DIRECTION ( 'NONE',  ( -1.000000000000000000, 0.000000000000000000, 0.000000000000000000 ) ) ;
#33436 = LINE ( 'NONE', #837, #15260 ) ;
#33437 = DIRECTION ( 'NONE',  ( -1.000000000000000000, 0.000000000000000000, 0.000000000000000000 ) ) ;
#33439 = VERTEX_POINT ( 'NONE', #18831 ) ;
#33438 = FACE_OUTER_BOUND ( 'NONE', #36197, .T. ) ;
#33440 = ORIENTED_EDGE ( 'NONE', *, *, #44543, .F. ) ;
#33441 = ADVANCED_FACE ( 'NONE', ( #50915 ), #3065, .F. ) ;
#33442 = EDGE_CURVE ( 'NONE', #48594, #177, #7783, .T. ) ;
#33443 = DIRECTION ( 'NONE',  ( -0.9890401873221644768, 0.000000000000000000, 0.1476465640024779702 ) ) ;
#33444 = EDGE_CURVE ( 'NONE', #37576, #30515, #43263, .T. ) ;
#33445 = DIRECTION ( 'NONE',  ( 0.1182731709213660498, 0.000000000000000000, -0.9929810960135169173 ) ) ;
#33447 = ORIENTED_EDGE ( 'NONE', *, *, #32362, .T. ) ;
#33446 = CARTESIAN_POINT ( 'NONE',  ( -141.5426765053792906, -177.1207230881787780, 81.94739446021134199 ) ) ;
#33448 = VERTEX_POINT ( 'NONE', #43780 ) ;
#33449 = VECTOR ( 'NONE', #32319, 1000.000000000000000 ) ;
#33450 = ORIENTED_EDGE ( 'NONE', *, *, #16775, .T. ) ;
#33451 = CARTESIAN_POINT ( 'NONE',  ( -143.3583119192899744, -177.1207230881787780, -81.38144888055202841 ) ) ;
#33452 = SHAPE_REPRESENTATION ( 'bin', ( #31742 ), #18326 ) ;
#33453 = AXIS2_PLACEMENT_3D ( 'NONE', #29739, #45789, #48952 ) ;
#33454 = FACE_OUTER_BOUND ( 'NONE', #469, .T. ) ;
#33455 = CARTESIAN_POINT ( 'NONE',  ( -332.3517673607765914, -123.5000000000000284, 0.000000000000000000 ) ) ;
#33456 = ORIENTED_EDGE ( 'NONE', *, *, #35981, .T. ) ;
#33457 = CARTESIAN_POINT ( 'NONE',  ( -172.5669052183642123, -193.5000000000000000, 15.07392567185553567 ) ) ;
#33458 = VECTOR ( 'NONE', #42214, 999.9999999999998863 ) ;
#33460 = ORIENTED_EDGE ( 'NONE', *, *, #34651, .F. ) ;
#33459 = DIRECTION ( 'NONE',  ( 0.000000000000000000, -1.000000000000000000, 0.000000000000000000 ) ) ;
#33461 = ADVANCED_FACE ( 'NONE', ( #23313 ), #11974, .T. ) ;
#33462 = DIRECTION ( 'NONE',  ( 0.000000000000000000, 0.000000000000000000, 1.000000000000000000 ) ) ;
#33463 = ORIENTED_EDGE ( 'NONE', *, *, #18868, .T. ) ;
#33464 = CARTESIAN_POINT ( 'NONE',  ( -49.21696003055058810, -183.6283474603465606, 0.6749830015182108900 ) ) ;
#33465 = VERTEX_POINT ( 'NONE', #19612 ) ;
#33466 = FACE_OUTER_BOUND ( 'NONE', #38366, .T. ) ;
#33467 = CARTESIAN_POINT ( 'NONE',  ( -142.6204786402482227, -183.6283474603465606, -80.70646587903385694 ) ) ;
#33468 = FACE_OUTER_BOUND ( 'NONE', #47674, .T. ) ;
#33469 = EDGE_CURVE ( 'NONE', #17674, #27996, #8045, .T. ) ;
#33470 = VECTOR ( 'NONE', #14984, 999.9999999999998863 ) ;
#33471 = EDGE_LOOP ( 'NONE', ( #11295, #9147, #36321, #4065 ) ) ;
#33472 = ORIENTED_EDGE ( 'NONE', *, *, #4473, .F. ) ;
#33473 = CARTESIAN_POINT ( 'NONE',  ( 49.10711742958948633, -189.7472609257535510, 78.11481899503480975 ) ) ;
#33474 = DIRECTION ( 'NONE',  ( -0.7378332790417333475, 0.000000000000000000, 0.6749830015182038956 ) ) ;
#33475 = ORIENTED_EDGE ( 'NONE', *, *, #10219, .F. ) ;
#33476 = DIRECTION ( 'NONE',  ( -0.000000000000000000, 1.000000000000000000, -0.000000000000000000 ) ) ;
#33477 = ORIENTED_EDGE ( 'NONE', *, *, #42864, .T. ) ;
#33478 = CARTESIAN_POINT ( 'NONE',  ( -336.3521761649654422, -101.0520950768976149, 54.58714071513087873 ) ) ;
#33479 = FACE_OUTER_BOUND ( 'NONE', #44386, .T. ) ;
#33480 = VERTEX_POINT ( 'NONE', #15167 ) ;
#33481 = CARTESIAN_POINT ( 'NONE',  ( -150.1390659022305840, -175.3837268820161057, 72.73415134496006829 ) ) ;
#33482 = ORIENTED_EDGE ( 'NONE', *, *, #42970, .F. ) ;
#33483 = AXIS2_PLACEMENT_3D ( 'NONE', #15507, #12053, #15785 ) ;
#33484 = VECTOR ( 'NONE', #44459, 1000.000000000000000 ) ;
#33485 = LINE ( 'NONE', #30047, #39626 ) ;
#33486 = CARTESIAN_POINT ( 'NONE',  ( -48.47912675150885065, -183.6283474603465606, 6.938893903907228378E-15 ) ) ;
#33487 = ORIENTED_EDGE ( 'NONE', *, *, #23854, .F. ) ;
#33488 = CIRCLE ( 'NONE', #17549, 125.0000000000000000 ) ;
#33489 = FACE_OUTER_BOUND ( 'NONE', #24809, .T. ) ;
#33490 = DIRECTION ( 'NONE',  ( 0.000000000000000000, -1.000000000000000000, -0.000000000000000000 ) ) ;
#33491 = DIRECTION ( 'NONE',  ( -0.05924062789372142729, 0.000000000000000000, 0.9982437317643209074 ) ) ;
#33492 = CARTESIAN_POINT ( 'NONE',  ( -170.4669447856608997, -183.6283474603465606, 22.25084316132123874 ) ) ;
#33493 = ORIENTED_EDGE ( 'NONE', *, *, #2418, .T. ) ;
#33494 = LINE ( 'NONE', #24817, #25344 ) ;
#33495 = EDGE_LOOP ( 'NONE', ( #3233, #19152, #28201, #5987 ) ) ;
#33496 = EDGE_LOOP ( 'NONE', ( #16105, #31770, #8440, #42252 ) ) ;
#33497 = VECTOR ( 'NONE', #40380, 1000.000000000000227 ) ;
#33498 = CARTESIAN_POINT ( 'NONE',  ( -260.0000000000000000, -113.5000000000000000, 60.00000000000000711 ) ) ;
#33500 = EDGE_LOOP ( 'NONE', ( #49953, #8654, #35184, #44770 ) ) ;
#33499 = DIRECTION ( 'NONE',  ( -0.08879589532294572540, 0.000000000000000000, 0.9960498426152160079 ) ) ;
#33501 = ORIENTED_EDGE ( 'NONE', *, *, #47800, .F. ) ;
#33502 = DIRECTION ( 'NONE',  ( 0.000000000000000000, 0.000000000000000000, 1.000000000000000000 ) ) ;
#33503 = EDGE_CURVE ( 'NONE', #44745, #26454, #3850, .T. ) ;
#33504 = CIRCLE ( 'NONE', #17564, 4.999999999999997335 ) ;
#33505 = LINE ( 'NONE', #37170, #8651 ) ;
#33506 = VERTEX_POINT ( 'NONE', #15430 ) ;
#33507 = DIRECTION ( 'NONE',  ( -8.718379230999704661E-17, 0.9927088740980544168, 0.1205366802553199113 ) ) ;
#33508 = ORIENTED_EDGE ( 'NONE', *, *, #9012, .F. ) ;
#33509 = CARTESIAN_POINT ( 'NONE',  ( 11.61413489515543418, -193.5000000000000000, -109.6074810615842381 ) ) ;
#33510 = CARTESIAN_POINT ( 'NONE',  ( -330.4913330509368166, -90.39567187580871632, -48.84008046109136814 ) ) ;
#33511 = CARTESIAN_POINT ( 'NONE',  ( 60.19403481868997829, -193.5000000000000000, -59.71720175837096889 ) ) ;
#33512 = CARTESIAN_POINT ( 'NONE',  ( 46.00000000000000711, 35.00000000000000000, -46.00000000000000000 ) ) ;
#33513 = ORIENTED_EDGE ( 'NONE', *, *, #33555, .T. ) ;
#33514 = EDGE_LOOP ( 'NONE', ( #23657, #46708, #35843, #51278 ) ) ;
#33515 = ORIENTED_EDGE ( 'NONE', *, *, #30813, .T. ) ;
#33516 = DIRECTION ( 'NONE',  ( -0.000000000000000000, -0.5680647467311596976, -0.8229838658936536877 ) ) ;
#33517 = FACE_OUTER_BOUND ( 'NONE', #50804, .T. ) ;
#33518 = AXIS2_PLACEMENT_3D ( 'NONE', #24376, #44080, #51996 ) ;
#33519 = EDGE_CURVE ( 'NONE', #9591, #39115, #35374, .T. ) ;
#33520 = PLANE ( 'NONE',  #34573 ) ;
#33521 = FACE_OUTER_BOUND ( 'NONE', #29544, .T. ) ;
#33522 = ORIENTED_EDGE ( 'NONE', *, *, #22392, .T. ) ;
#33523 =( GEOMETRIC_REPRESENTATION_CONTEXT ( 3 ) GLOBAL_UNCERTAINTY_ASSIGNED_CONTEXT ( ( #22721 ) ) GLOBAL_UNIT_ASSIGNED_CONTEXT ( ( #29615, #28829, #456 ) ) REPRESENTATION_CONTEXT ( 'NONE', 'WORKASPACE' ) );
#33524 = ORIENTED_EDGE ( 'NONE', *, *, #7696, .T. ) ;
#33526 = ORIENTED_EDGE ( 'NONE', *, *, #43916, .F. ) ;
#33525 = DIRECTION ( 'NONE',  ( 0.000000000000000000, -1.000000000000000000, 0.000000000000000000 ) ) ;
#33527 = ORIENTED_EDGE ( 'NONE', *, *, #41312, .F. ) ;
#33528 = CARTESIAN_POINT ( 'NONE',  ( -336.3521761649654422, -76.88706545914891421, 37.77875505479673279 ) ) ;
#33529 = EDGE_CURVE ( 'NONE', #18469, #7899, #22418, .T. ) ;
#33530 = CARTESIAN_POINT ( 'NONE',  ( -72.96029774493611342, -177.1207230881787780, 122.5792489240759409 ) ) ;
#33531 = CARTESIAN_POINT ( 'NONE',  ( -166.8403286750647680, -193.5000000000000000, -40.19484891389966918 ) ) ;
#33532 = CARTESIAN_POINT ( 'NONE',  ( -339.1964088526558498, -109.8658467157473666, -57.40522506028092664 ) ) ;
#33533 = ORIENTED_EDGE ( 'NONE', *, *, #14000, .F. ) ;
#33535 = EDGE_CURVE ( 'NONE', #26711, #28978, #19107, .T. ) ;
#33534 = DIRECTION ( 'NONE',  ( -0.000000000000000000, 1.000000000000000000, -0.000000000000000000 ) ) ;
#33536 = ORIENTED_EDGE ( 'NONE', *, *, #45292, .F. ) ;
#33537 = CIRCLE ( 'NONE', #32697, 125.0000000000000000 ) ;
#33538 = VERTEX_POINT ( 'NONE', #11724 ) ;
#33539 = LINE ( 'NONE', #13031, #32120 ) ;
#33540 = CARTESIAN_POINT ( 'NONE',  ( -171.6469053867625121, -193.5000000000000000, -14.34663989163543008 ) ) ;
#33541 = ORIENTED_EDGE ( 'NONE', *, *, #37476, .T. ) ;
#33542 = FACE_OUTER_BOUND ( 'NONE', #29860, .T. ) ;
#33543 = CARTESIAN_POINT ( 'NONE',  ( -48.47912675150885065, -175.3837268820161057, 6.938893903907228378E-15 ) ) ;
#33544 = CARTESIAN_POINT ( 'NONE',  ( -109.0835867659424565, -177.1207230881787780, -109.3256576763154726 ) ) ;
#33545 = CARTESIAN_POINT ( 'NONE',  ( 0.000000000000000000, -180.7855672281372108, -14.11962419296555105 ) ) ;
#33546 = EDGE_CURVE ( 'NONE', #36985, #28401, #31702, .T. ) ;
#33547 = DIRECTION ( 'NONE',  ( 0.000000000000000000, -0.2393156642875685636, -0.9709418174260492362 ) ) ;
#33548 = FACE_OUTER_BOUND ( 'NONE', #12645, .T. ) ;
#33549 = VERTEX_POINT ( 'NONE', #51432 ) ;
#33550 = VECTOR ( 'NONE', #43758, 1000.000000000000000 ) ;
#33551 = CARTESIAN_POINT ( 'NONE',  ( 75.48400724637755843, -177.1207230881787780, -16.06677968424457958 ) ) ;
#33552 = VERTEX_POINT ( 'NONE', #31953 ) ;
#33553 = ORIENTED_EDGE ( 'NONE', *, *, #51576, .F. ) ;
#33554 = DIRECTION ( 'NONE',  ( 0.000000000000000000, -1.000000000000000000, 0.000000000000000000 ) ) ;
#33555 = EDGE_CURVE ( 'NONE', #47219, #49227, #23814, .T. ) ;
#33556 = EDGE_LOOP ( 'NONE', ( #26399, #47811, #51722, #5971 ) ) ;
#33557 = EDGE_CURVE ( 'NONE', #38799, #11493, #27222, .T. ) ;
#33558 = PRODUCT_DEFINITION_SHAPE ( 'NONE', 'NONE',  #52049 ) ;
#33559 = CARTESIAN_POINT ( 'NONE',  ( -31.30262293407085039, -193.5000000000000000, -123.8142468240611294 ) ) ;
#33560 = EDGE_CURVE ( 'NONE', #50970, #35187, #12343, .T. ) ;
#33561 = LINE ( 'NONE', #30630, #40191 ) ;
#33563 = VERTEX_POINT ( 'NONE', #27747 ) ;
#33562 = LINE ( 'NONE', #5719, #22054 ) ;
#33564 = PLANE ( 'NONE',  #44535 ) ;
#33565 = EDGE_LOOP ( 'NONE', ( #14689, #41205, #4044, #10398 ) ) ;
#33566 = EDGE_LOOP ( 'NONE', ( #19298, #33487, #4998, #7585 ) ) ;
#33567 = VECTOR ( 'NONE', #4672, 1000.000000000000000 ) ;
#33568 = VERTEX_POINT ( 'NONE', #28005 ) ;
#33569 = CARTESIAN_POINT ( 'NONE',  ( -332.3517673607765914, -140.1754235130667610, -56.65561927338005432 ) ) ;
#33570 = LINE ( 'NONE', #20970, #34395 ) ;
#33571 = ORIENTED_EDGE ( 'NONE', *, *, #19478, .F. ) ;
#33572 = EDGE_CURVE ( 'NONE', #27694, #20353, #51687, .T. ) ;
#33573 = CARTESIAN_POINT ( 'NONE',  ( -48.07600332222088468, -193.5000000000000000, 0.9151456172430280089 ) ) ;
#33574 = CARTESIAN_POINT ( 'NONE',  ( -48.30901192927175458, -193.5000000000000000, -123.9998842437354227 ) ) ;
#33575 = ORIENTED_EDGE ( 'NONE', *, *, #10517, .F. ) ;
#33576 = FILL_AREA_STYLE ('',( #1519 ) ) ;
#33577 = VERTEX_POINT ( 'NONE', #39821 ) ;
#33579 = ORIENTED_EDGE ( 'NONE', *, *, #40249, .F. ) ;
#33578 = CARTESIAN_POINT ( 'NONE',  ( 50.08808042611237710, -183.6283474603465606, -76.87330921200083367 ) ) ;
#33580 = ORIENTED_EDGE ( 'NONE', *, *, #13391, .T. ) ;
#33581 = CIRCLE ( 'NONE', #32714, 125.0000000000000000 ) ;
#33582 = ORIENTED_EDGE ( 'NONE', *, *, #27023, .F. ) ;
#33583 = CARTESIAN_POINT ( 'NONE',  ( -330.4913330509368166, -183.1207326066166559, 6.735595255827131922 ) ) ;
#33584 = DIRECTION ( 'NONE',  ( 1.000000000000000000, -0.000000000000000000, 0.000000000000000000 ) ) ;
#33585 = ORIENTED_EDGE ( 'NONE', *, *, #22338, .T. ) ;
#33586 = CARTESIAN_POINT ( 'NONE',  ( -26.71218532227686637, -189.7472609257535510, 122.0745693923550732 ) ) ;
#33587 = DIRECTION ( 'NONE',  ( 1.000000000000000000, 0.000000000000000000, 0.000000000000000000 ) ) ;
#33588 = VERTEX_POINT ( 'NONE', #47992 ) ;
#33589 = DIRECTION ( 'NONE',  ( 0.000000000000000000, 0.000000000000000000, 1.000000000000000000 ) ) ;
#33590 = ORIENTED_EDGE ( 'NONE', *, *, #9888, .T. ) ;
#33591 = ORIENTED_EDGE ( 'NONE', *, *, #5138, .T. ) ;
#33592 = DIRECTION ( 'NONE',  ( -0.000000000000000000, -0.000000000000000000, 1.000000000000000000 ) ) ;
#33593 = DIRECTION ( 'NONE',  ( -0.000000000000000000, 0.7485107481711069655, 0.6631226582407885317 ) ) ;
#33594 = DIRECTION ( 'NONE',  ( -0.000000000000000000, 1.000000000000000000, -0.000000000000000000 ) ) ;
#33595 = DIRECTION ( 'NONE',  ( 0.8455960035018272869, 0.000000000000000000, -0.5338233779647886257 ) ) ;
#33596 = EDGE_LOOP ( 'NONE', ( #33803, #8299, #35508, #43770 ) ) ;
#33597 = PLANE ( 'NONE',  #31546 ) ;
#33598 = CARTESIAN_POINT ( 'NONE',  ( -48.47912675150885065, -183.6283474603465606, 6.938893903907228378E-15 ) ) ;
#33599 = EDGE_CURVE ( 'NONE', #26525, #10132, #14562, .T. ) ;
#33600 = EDGE_CURVE ( 'NONE', #2622, #46969, #34969, .T. ) ;
#33601 = CARTESIAN_POINT ( 'NONE',  ( -171.0948786228703113, -189.7472609257535510, -18.47640724094506126 ) ) ;
#33602 = PLANE ( 'NONE',  #4390 ) ;
#33603 = VERTEX_POINT ( 'NONE', #10096 ) ;
#33604 = LINE ( 'NONE', #33354, #3680 ) ;
#33605 = CARTESIAN_POINT ( 'NONE',  ( -48.47912675150885065, -175.3837268820161057, 6.938893903907228378E-15 ) ) ;
#33606 = CIRCLE ( 'NONE', #19320, 125.0000000000000000 ) ;
#33607 = VECTOR ( 'NONE', #22685, 1000.000000000000000 ) ;
#33608 = PLANE ( 'NONE',  #24033 ) ;
#33609 = ORIENTED_EDGE ( 'NONE', *, *, #5233, .F. ) ;
#33610 = FACE_BOUND ( 'NONE', #27805, .T. ) ;
#33611 = CARTESIAN_POINT ( 'NONE',  ( -339.1964088526558498, -182.5000000000000568, -0.4999999999999543698 ) ) ;
#33612 = VERTEX_POINT ( 'NONE', #34269 ) ;
#33613 = FACE_OUTER_BOUND ( 'NONE', #43804, .T. ) ;
#33614 = EDGE_CURVE ( 'NONE', #2659, #15614, #42670, .T. ) ;
#33615 = EDGE_LOOP ( 'NONE', ( #19860, #47688, #35178, #15030 ) ) ;
#33616 = EDGE_CURVE ( 'NONE', #7764, #6309, #27140, .T. ) ;
#33617 = CARTESIAN_POINT ( 'NONE',  ( 65.38692482895591240, -177.1207230881787780, -51.57055649762701677 ) ) ;
#33618 = EDGE_CURVE ( 'NONE', #2420, #40551, #11112, .T. ) ;
#33619 = CIRCLE ( 'NONE', #37815, 125.0000000000000000 ) ;
#33620 = DIRECTION ( 'NONE',  ( -0.000000000000000000, 0.000000000000000000, -1.000000000000000000 ) ) ;
#33621 = PLANE ( 'NONE',  #41352 ) ;
#33622 = DIRECTION ( 'NONE',  ( -0.000000000000000000, 1.000000000000000000, -0.000000000000000000 ) ) ;
#33623 = ADVANCED_FACE ( 'NONE', ( #6426 ), #50315, .F. ) ;
#33624 = FACE_OUTER_BOUND ( 'NONE', #33359, .T. ) ;
#33625 = DIRECTION ( 'NONE',  ( -0.000000000000000000, 1.000000000000000000, -0.000000000000000000 ) ) ;
#33626 = ORIENTED_EDGE ( 'NONE', *, *, #19102, .T. ) ;
#33627 = CARTESIAN_POINT ( 'NONE',  ( 67.66641500972446011, -175.3837268820161057, 46.20836643931067300 ) ) ;
#33628 = ORIENTED_EDGE ( 'NONE', *, *, #18036, .T. ) ;
#33629 = PLANE ( 'NONE',  #9932 ) ;
#33630 = EDGE_LOOP ( 'NONE', ( #123, #19031, #10061, #21304 ) ) ;
#33631 = CARTESIAN_POINT ( 'NONE',  ( -305.0000000000000568, -183.2372378732723632, -5.609136410542876483 ) ) ;
#33632 = CIRCLE ( 'NONE', #1860, 124.9999999999999858 ) ;
#33633 = ORIENTED_EDGE ( 'NONE', *, *, #866, .F. ) ;
#33634 = AXIS2_PLACEMENT_3D ( 'NONE', #50180, #45452, #45709 ) ;
#33635 = DIRECTION ( 'NONE',  ( 1.000000000000000000, 0.000000000000000000, 0.000000000000000000 ) ) ;
#33636 = DIRECTION ( 'NONE',  ( 0.000000000000000000, 0.000000000000000000, -1.000000000000000000 ) ) ;
#33637 = ORIENTED_EDGE ( 'NONE', *, *, #47006, .F. ) ;
#33640 = ORIENTED_EDGE ( 'NONE', *, *, #37358, .T. ) ;
#33639 = DIRECTION ( 'NONE',  ( -0.000000000000000000, 1.000000000000000000, -0.000000000000000000 ) ) ;
#33638 = DIRECTION ( 'NONE',  ( 0.2920567706369764371, 0.000000000000000000, -0.9564009842765223146 ) ) ;
#33641 = PLANE ( 'NONE',  #32312 ) ;
#33642 = ORIENTED_EDGE ( 'NONE', *, *, #793, .T. ) ;
#33643 = LINE ( 'NONE', #12886, #33136 ) ;
#33644 = VERTEX_POINT ( 'NONE', #6679 ) ;
#33645 = LINE ( 'NONE', #1602, #40952 ) ;
#33648 = ORIENTED_EDGE ( 'NONE', *, *, #43692, .F. ) ;
#33647 = PLANE ( 'NONE',  #29151 ) ;
#33646 = DIRECTION ( 'NONE',  ( -1.000000000000000000, -0.000000000000000000, -0.000000000000000000 ) ) ;
#33649 = VERTEX_POINT ( 'NONE', #22957 ) ;
#33650 = ADVANCED_FACE ( 'NONE', ( #26884 ), #50824, .T. ) ;
#33651 = DIRECTION ( 'NONE',  ( -0.9995608365087942371, 0.000000000000000000, -0.02963332782256331357 ) ) ;
#33652 = FACE_OUTER_BOUND ( 'NONE', #383, .T. ) ;
#33654 = AXIS2_PLACEMENT_3D ( 'NONE', #34776, #18510, #6436 ) ;
#33653 = CARTESIAN_POINT ( 'NONE',  ( -48.47912675150885065, -177.1207230881787780, 6.938893903907228378E-15 ) ) ;
#33655 = ORIENTED_EDGE ( 'NONE', *, *, #20786, .F. ) ;
#33656 = DIRECTION ( 'NONE',  ( -0.000000000000000000, -1.000000000000000000, 0.000000000000000000 ) ) ;
#33657 = DIRECTION ( 'NONE',  ( -0.000000000000000000, 1.000000000000000000, -0.000000000000000000 ) ) ;
#33658 = CARTESIAN_POINT ( 'NONE',  ( -64.08700758308647494, -193.5000000000000000, -124.0217483183786840 ) ) ;
#33659 = EDGE_CURVE ( 'NONE', #46918, #26606, #34766, .T. ) ;
#33660 = EDGE_CURVE ( 'NONE', #50992, #28039, #44245, .T. ) ;
#33661 = ORIENTED_EDGE ( 'NONE', *, *, #49052, .T. ) ;
#33662 = EDGE_CURVE ( 'NONE', #28777, #41926, #30068, .T. ) ;
#33663 = DIRECTION ( 'NONE',  ( -1.000000000000000000, 0.000000000000000000, 0.000000000000000000 ) ) ;
#33664 = DIRECTION ( 'NONE',  ( -0.9993908270190956511, 4.273955692857142571E-18, -0.03489949670250096919 ) ) ;
#33665 = EDGE_CURVE ( 'NONE', #7704, #28470, #22698, .T. ) ;
#33666 = CARTESIAN_POINT ( 'NONE',  ( -305.0000000000000568, -168.7406467949206785, -39.41172259083884910 ) ) ;
#33667 = ORIENTED_EDGE ( 'NONE', *, *, #24520, .T. ) ;
#33668 = DIRECTION ( 'NONE',  ( -0.000000000000000000, -0.9927088740980534176, 0.1205366802553268502 ) ) ;
#33669 = EDGE_CURVE ( 'NONE', #43478, #47044, #43175, .T. ) ;
#33670 = DIRECTION ( 'NONE',  ( -0.000000000000000000, 1.000000000000000000, 0.000000000000000000 ) ) ;
#33671 = CIRCLE ( 'NONE', #20236, 60.00000000000000000 ) ;
#33672 = DIRECTION ( 'NONE',  ( -0.9995608365087940150, 0.000000000000000000, -0.02963332782257007206 ) ) ;
#33673 = CARTESIAN_POINT ( 'NONE',  ( 52.16997862029127475, -193.5000000000000000, 72.42760398749085482 ) ) ;
#33674 = ADVANCED_FACE ( 'NONE', ( #35290 ), #18502, .F. ) ;
#33675 = EDGE_CURVE ( 'NONE', #11325, #5201, #46764, .T. ) ;
#33676 = AXIS2_PLACEMENT_3D ( 'NONE', #23844, #39855, #35667 ) ;
#33677 = CARTESIAN_POINT ( 'NONE',  ( -336.3521761649654422, -170.5607375887735770, 35.68215131113770155 ) ) ;
#33678 = EDGE_CURVE ( 'NONE', #23489, #36830, #46365, .T. ) ;
#33679 = AXIS2_PLACEMENT_3D ( 'NONE', #40062, #374, #23527 ) ;
#33680 = CARTESIAN_POINT ( 'NONE',  ( 54.18765407974402848, -183.6283474603465606, -69.53890913632879744 ) ) ;
#33681 = CARTESIAN_POINT ( 'NONE',  ( 60.90550954139435902, -175.3837268820161057, 60.49794494914085874 ) ) ;
#33683 = ORIENTED_EDGE ( 'NONE', *, *, #27610, .F. ) ;
#33682 = PLANE ( 'NONE',  #42982 ) ;
#33684 = EDGE_CURVE ( 'NONE', #50065, #14521, #35042, .T. ) ;
#33685 = VERTEX_POINT ( 'NONE', #42405 ) ;
#33686 = DIRECTION ( 'NONE',  ( 0.000000000000000000, -0.000000000000000000, 1.000000000000000000 ) ) ;
#33687 = EDGE_CURVE ( 'NONE', #6776, #21227, #31087, .T. ) ;
#33688 = CARTESIAN_POINT ( 'NONE',  ( -172.9701362814535912, -189.7472609257535510, -11.26891947860197440 ) ) ;
#33690 = ORIENTED_EDGE ( 'NONE', *, *, #23861, .T. ) ;
#33689 = LINE ( 'NONE', #21874, #30372 ) ;
#33691 = ORIENTED_EDGE ( 'NONE', *, *, #13498, .F. ) ;
#33692 = VECTOR ( 'NONE', #7463, 1000.000000000000000 ) ;
#33693 = ORIENTED_EDGE ( 'NONE', *, *, #50958, .T. ) ;
#33694 = CARTESIAN_POINT ( 'NONE',  ( 0.000000000000000000, -63.50000000000000000, 20.00000000000000000 ) ) ;
#33695 = LINE ( 'NONE', #5337, #107 ) ;
#33696 = CARTESIAN_POINT ( 'NONE',  ( -339.1964088526558498, -175.5095439275177398, -27.86139516340860212 ) ) ;
#33697 = ORIENTED_EDGE ( 'NONE', *, *, #36828, .F. ) ;
#33698 = ADVANCED_FACE ( 'NONE', ( #3251 ), #46116, .T. ) ;
#33699 = DIRECTION ( 'NONE',  ( -0.000000000000000000, 1.000000000000000000, -0.000000000000000000 ) ) ;
#33701 = ORIENTED_EDGE ( 'NONE', *, *, #26085, .T. ) ;
#33700 = CARTESIAN_POINT ( 'NONE',  ( -332.3517673607765914, -69.26746417191145611, -23.38292116578723068 ) ) ;
#33702 = DIRECTION ( 'NONE',  ( -0.000000000000000000, 1.000000000000000000, -0.000000000000000000 ) ) ;
#33703 = ORIENTED_EDGE ( 'NONE', *, *, #21077, .F. ) ;
#33704 = PLANE ( 'NONE',  #49051 ) ;
#33705 = VECTOR ( 'NONE', #28805, 1000.000000000000000 ) ;
#33706 = EDGE_LOOP ( 'NONE', ( #42511, #17030, #14561, #19566 ) ) ;
#33707 = DIRECTION ( 'NONE',  ( 0.9890401873221633666, 0.000000000000000000, 0.1476465640024850756 ) ) ;
#33708 = DIRECTION ( 'NONE',  ( 0.6965510290629932655, 0.000000000000000000, 0.7175072570443347120 ) ) ;
#33709 = AXIS2_PLACEMENT_3D ( 'NONE', #167, #3346, #12254 ) ;
#33710 = LINE ( 'NONE', #26079, #7276 ) ;
#33711 = VECTOR ( 'NONE', #13454, 1000.000000000000114 ) ;
#33712 = VERTEX_POINT ( 'NONE', #27918 ) ;
#33713 = ORIENTED_EDGE ( 'NONE', *, *, #22870, .F. ) ;
#33714 = PLANE ( 'NONE',  #41567 ) ;
#33715 = PLANE ( 'NONE',  #48496 ) ;
#33716 = ORIENTED_EDGE ( 'NONE', *, *, #10815, .T. ) ;
#33717 = LINE ( 'NONE', #26086, #35064 ) ;
#33718 = ADVANCED_FACE ( 'NONE', ( #43698 ), #43950, .T. ) ;
#33719 = EDGE_CURVE ( 'NONE', #1947, #15758, #3487, .T. ) ;
#33720 = ORIENTED_EDGE ( 'NONE', *, *, #38531, .T. ) ;
#33721 = FACE_OUTER_BOUND ( 'NONE', #51173, .T. ) ;
#33722 = AXIS2_PLACEMENT_3D ( 'NONE', #17920, #17419, #13974 ) ;
#33723 = DIRECTION ( 'NONE',  ( 0.7575112421616236880, 0.000000000000000000, -0.6528221181905174975 ) ) ;
#33724 = EDGE_CURVE ( 'NONE', #34754, #51254, #32122, .T. ) ;
#33725 = EDGE_CURVE ( 'NONE', #25328, #8967, #7940, .T. ) ;
#33726 = ORIENTED_EDGE ( 'NONE', *, *, #8613, .T. ) ;
#33727 = CARTESIAN_POINT ( 'NONE',  ( -336.3521761649654422, -123.5000000000000284, 0.000000000000000000 ) ) ;
#33728 = EDGE_LOOP ( 'NONE', ( #35419, #40870, #7547, #24513 ) ) ;
#33729 = VECTOR ( 'NONE', #35630, 1000.000000000000000 ) ;
#33730 = DIRECTION ( 'NONE',  ( 0.5085311186492094127, 0.000000000000000000, 0.8610436117673619938 ) ) ;
#33731 = CARTESIAN_POINT ( 'NONE',  ( 62.86098202833237281, -183.6283474603465606, 56.81883646197908888 ) ) ;
#33732 = FACE_OUTER_BOUND ( 'NONE', #33224, .T. ) ;
#33733 = VERTEX_POINT ( 'NONE', #51584 ) ;
#33734 = CARTESIAN_POINT ( 'NONE',  ( -126.2322430781613605, -193.5000000000000000, 97.87467957288053810 ) ) ;
#33735 = CARTESIAN_POINT ( 'NONE',  ( 11.61413489515543418, -177.1207230881787780, -109.6074810615842381 ) ) ;
#33736 = CARTESIAN_POINT ( 'NONE',  ( -336.3521761649654422, -145.9479049231020440, -54.58714071513102795 ) ) ;
#33737 = CARTESIAN_POINT ( 'NONE',  ( 34.98161733638497850, -183.6283474603465606, -91.70840728318314916 ) ) ;
#33738 = ORIENTED_EDGE ( 'NONE', *, *, #28506, .F. ) ;
#33739 = DIRECTION ( 'NONE',  ( -0.000000000000000000, 0.1205366802553199113, -0.9927088740980544168 ) ) ;
#33740 = ORIENTED_EDGE ( 'NONE', *, *, #18488, .F. ) ;
#33741 = EDGE_CURVE ( 'NONE', #14876, #40260, #15711, .T. ) ;
#33742 = DIRECTION ( 'NONE',  ( -0.000000000000000000, 1.000000000000000000, -0.000000000000000000 ) ) ;
#33743 = LINE ( 'NONE', #45840, #11051 ) ;
#33744 = VECTOR ( 'NONE', #18149, 1000.000000000000114 ) ;
#33745 = VERTEX_POINT ( 'NONE', #31869 ) ;
#33746 = CYLINDRICAL_SURFACE ( 'NONE', #48378, 5.000000000000001776 ) ;
#33747 = AXIS2_PLACEMENT_3D ( 'NONE', #47374, #30825, #6910 ) ;
#33748 = EDGE_CURVE ( 'NONE', #8114, #49438, #15859, .T. ) ;
#33749 = AXIS2_PLACEMENT_3D ( 'NONE', #29669, #17609, #33620 ) ;
#33750 = CARTESIAN_POINT ( 'NONE',  ( -48.47912675150885065, -120.5000000000000284, -14.00000000000000355 ) ) ;
#33751 = EDGE_LOOP ( 'NONE', ( #3491, #46309, #35968, #16872 ) ) ;
#33752 = PLANE ( 'NONE',  #10484 ) ;
#33753 = ORIENTED_EDGE ( 'NONE', *, *, #1257, .F. ) ;
#33754 = PLANE ( 'NONE',  #31722 ) ;
#33755 = DIRECTION ( 'NONE',  ( 0.9051968626821054187, 0.4249925173346860707, 0.000000000000000000 ) ) ;
#33756 = CARTESIAN_POINT ( 'NONE',  ( -172.4422607493951602, -177.1207230881787780, 16.06677968424543934 ) ) ;
#33757 = DIRECTION ( 'NONE',  ( -0.000000000000000000, -0.8854560256532079121, 0.4647231720437724478 ) ) ;
#33758 = VERTEX_POINT ( 'NONE', #11368 ) ;
#33759 = VECTOR ( 'NONE', #46820, 1000.000000000000000 ) ;
#33760 = EDGE_LOOP ( 'NONE', ( #28060, #4464, #39377, #10332 ) ) ;
#33761 = CIRCLE ( 'NONE', #43918, 125.0000000000000000 ) ;
#33762 = ORIENTED_EDGE ( 'NONE', *, *, #2236, .T. ) ;
#33763 = CARTESIAN_POINT ( 'NONE',  ( -336.3521761649654422, -182.3871109312487420, -4.498567634386014369 ) ) ;
#33764 = DIRECTION ( 'NONE',  ( -0.000000000000000000, -0.6631226582407964143, -0.7485107481710999711 ) ) ;
#33765 = VECTOR ( 'NONE', #1796, 1000.000000000000000 ) ;
#33766 = CIRCLE ( 'NONE', #8586, 125.0000000000000000 ) ;
#33767 = LINE ( 'NONE', #21692, #37094 ) ;
#33768 = DIRECTION ( 'NONE',  ( 0.000000000000000000, -0.4739294676984007193, 0.8805628084623552398 ) ) ;
#33769 = EDGE_LOOP ( 'NONE', ( #20262, #51558, #6109, #22774, #36923 ) ) ;
#33770 = UNCERTAINTY_MEASURE_WITH_UNIT (LENGTH_MEASURE( 1.000000000000000082E-05 ), #6076, 'distance_accuracy_value', 'NONE');
#33771 = ORIENTED_EDGE ( 'NONE', *, *, #36486, .F. ) ;
#33773 = ORIENTED_EDGE ( 'NONE', *, *, #22902, .T. ) ;
#33772 = LINE ( 'NONE', #5681, #8871 ) ;
#33774 = ORIENTED_EDGE ( 'NONE', *, *, #22474, .T. ) ;
#33775 = PLANE ( 'NONE',  #17437 ) ;
#33776 = FACE_OUTER_BOUND ( 'NONE', #6519, .T. ) ;
#33777 = AXIS2_PLACEMENT_3D ( 'NONE', #29640, #41208, #5235 ) ;
#33778 = DIRECTION ( 'NONE',  ( -1.000000000000000000, 0.000000000000000000, -0.000000000000000000 ) ) ;
#33779 = EDGE_CURVE ( 'NONE', #49533, #8359, #36066, .T. ) ;
#33781 = EDGE_CURVE ( 'NONE', #44141, #8140, #27400, .T. ) ;
#33780 = FACE_OUTER_BOUND ( 'NONE', #35159, .T. ) ;
#33782 = ORIENTED_EDGE ( 'NONE', *, *, #23151, .F. ) ;
#33783 = CARTESIAN_POINT ( 'NONE',  ( -113.5519059482138857, -183.6283474603465606, 105.5544085257715210 ) ) ;
#33784 = CIRCLE ( 'NONE', #32123, 60.00000000000000000 ) ;
#33785 = ORIENTED_EDGE ( 'NONE', *, *, #43268, .T. ) ;
#33786 = DIRECTION ( 'NONE',  ( -0.000000000000000000, -0.9927088740980530845, 0.1205366802553303057 ) ) ;
#33787 = LINE ( 'NONE', #2509, #32005 ) ;
#33788 = VERTEX_POINT ( 'NONE', #31606 ) ;
#33789 = CARTESIAN_POINT ( 'NONE',  ( 61.22907552172956969, -183.6283474603465606, -57.79541595648220920 ) ) ;
#33790 = PLANE ( 'NONE',  #17139 ) ;
#33791 = CARTESIAN_POINT ( 'NONE',  ( -48.47912675150885065, -175.3837268820161057, 6.938893903907228378E-15 ) ) ;
#33792 = DIRECTION ( 'NONE',  ( -8.718379230999707126E-17, 0.000000000000000000, -1.000000000000000000 ) ) ;
#33793 = VECTOR ( 'NONE', #1227, 999.9999999999998863 ) ;
#33794 = AXIS2_PLACEMENT_3D ( 'NONE', #1470, #33778, #38233 ) ;
#33795 = LINE ( 'NONE', #45903, #11036 ) ;
#33796 = FACE_BOUND ( 'NONE', #34213, .T. ) ;
#33797 = EDGE_LOOP ( 'NONE', ( #20242, #3503, #47673, #28649 ) ) ;
#33798 = AXIS2_PLACEMENT_3D ( 'NONE', #2832, #31729, #39847 ) ;
#33799 = VECTOR ( 'NONE', #22172, 1000.000000000000000 ) ;
#33800 = EDGE_CURVE ( 'NONE', #37750, #35361, #35012, .T. ) ;
#33801 = DIRECTION ( 'NONE',  ( 0.000000000000000000, 0.000000000000000000, 1.000000000000000000 ) ) ;
#33802 = ORIENTED_EDGE ( 'NONE', *, *, #33741, .F. ) ;
#33803 = ORIENTED_EDGE ( 'NONE', *, *, #36196, .F. ) ;
#33804 = LINE ( 'NONE', #49338, #7833 ) ;
#33805 = AXIS2_PLACEMENT_3D ( 'NONE', #17348, #42008, #6280 ) ;
#33806 = ORIENTED_EDGE ( 'NONE', *, *, #41378, .F. ) ;
#33807 = ADVANCED_FACE ( 'NONE', ( #23721 ), #27668, .F. ) ;
#33808 = FACE_OUTER_BOUND ( 'NONE', #248, .T. ) ;
#33809 = LINE ( 'NONE', #5454, #26763 ) ;
#33811 = EDGE_LOOP ( 'NONE', ( #39732, #41917, #40207, #40098 ) ) ;
#33810 = LINE ( 'NONE', #24899, #4417 ) ;
#33812 = EDGE_CURVE ( 'NONE', #2088, #33816, #20042, .T. ) ;
#33813 = CARTESIAN_POINT ( 'NONE',  ( -115.7878797639662025, -177.1207230881787780, -104.1428419024399687 ) ) ;
#33814 = LINE ( 'NONE', #13852, #35766 ) ;
#33815 = ORIENTED_EDGE ( 'NONE', *, *, #2576, .T. ) ;
#33816 = VERTEX_POINT ( 'NONE', #35809 ) ;
#33817 = AXIS2_PLACEMENT_3D ( 'NONE', #10097, #12986, #6166 ) ;
#33818 = ORIENTED_EDGE ( 'NONE', *, *, #51528, .F. ) ;
#33819 = CARTESIAN_POINT ( 'NONE',  ( -336.3521761649654422, -75.66382151296542702, -36.21739951675945690 ) ) ;
#33820 = DIRECTION ( 'NONE',  ( -0.000000000000000000, 1.000000000000000000, -0.000000000000000000 ) ) ;
#33821 = DIRECTION ( 'NONE',  ( 0.000000000000000000, 1.000000000000000000, 0.000000000000000000 ) ) ;
#33822 = DIRECTION ( 'NONE',  ( -0.7378332790417333475, 0.000000000000000000, 0.6749830015182038956 ) ) ;
#33823 = DIRECTION ( 'NONE',  ( 0.000000000000000000, 0.000000000000000000, 1.000000000000000000 ) ) ;
#33824 = ORIENTED_EDGE ( 'NONE', *, *, #2218, .T. ) ;
#33825 = AXIS2_PLACEMENT_3D ( 'NONE', #21325, #33917, #46538 ) ;
#33826 = VECTOR ( 'NONE', #35104, 1000.000000000000000 ) ;
#33827 = EDGE_CURVE ( 'NONE', #41514, #15304, #23477, .T. ) ;
#33828 = CARTESIAN_POINT ( 'NONE',  ( 76.28370911321322012, -193.5000000000000000, -7.696413904697510411 ) ) ;
#33829 = CARTESIAN_POINT ( 'NONE',  ( -339.1964088526558498, -162.9984922102927385, -43.83057281297435992 ) ) ;
#33830 = EDGE_LOOP ( 'NONE', ( #19870, #17213, #11906, #42941 ) ) ;
#33832 = VERTEX_POINT ( 'NONE', #8465 ) ;
#33831 = FACE_OUTER_BOUND ( 'NONE', #13231, .T. ) ;
#33833 = VECTOR ( 'NONE', #36845, 1000.000000000000000 ) ;
#33834 = ORIENTED_EDGE ( 'NONE', *, *, #42022, .T. ) ;
#33835 = VERTEX_POINT ( 'NONE', #11642 ) ;
#33836 = FACE_OUTER_BOUND ( 'NONE', #21778, .T. ) ;
#33837 = CARTESIAN_POINT ( 'NONE',  ( 69.04371411670899761, -189.7472609257535510, -39.55227055146231407 ) ) ;
#33838 = VERTEX_POINT ( 'NONE', #3743 ) ;
#33839 = CARTESIAN_POINT ( 'NONE',  ( -48.47912675150885065, -193.5000000000000000, 1.000000000000006883 ) ) ;
#33840 = ADVANCED_FACE ( 'NONE', ( #48427 ), #39487, .T. ) ;
#33841 = VECTOR ( 'NONE', #39025, 1000.000000000000000 ) ;
#33842 = LINE ( 'NONE', #29897, #30118 ) ;
#33843 = ORIENTED_EDGE ( 'NONE', *, *, #1663, .F. ) ;
#33844 = EDGE_CURVE ( 'NONE', #45175, #27293, #12306, .T. ) ;
#33845 = CARTESIAN_POINT ( 'NONE',  ( -170.4669447856608997, -177.1207230881787780, 22.25084316132123519 ) ) ;
#33846 = VERTEX_POINT ( 'NONE', #36324 ) ;
#33847 = VERTEX_POINT ( 'NONE', #319 ) ;
#33848 = DIRECTION ( 'NONE',  ( 1.000000000000000000, 0.000000000000000000, -0.000000000000000000 ) ) ;
#33849 = ADVANCED_FACE ( 'NONE', ( #44479 ), #16363, .T. ) ;
#33850 = LINE ( 'NONE', #46464, #39826 ) ;
#33851 = FILL_AREA_STYLE ('',( #45695 ) ) ;
#33852 = ORIENTED_EDGE ( 'NONE', *, *, #12016, .T. ) ;
#33853 = LINE ( 'NONE', #49893, #38261 ) ;
#33854 = CIRCLE ( 'NONE', #27954, 10.00000000000000000 ) ;
#33855 = PLANE ( 'NONE',  #33956 ) ;
#33856 = CARTESIAN_POINT ( 'NONE',  ( -336.3521761649654422, -76.43926241122620979, -35.68215131113738181 ) ) ;
#33857 = DIRECTION ( 'NONE',  ( -0.000000000000000000, 1.000000000000000000, -0.000000000000000000 ) ) ;
#33858 = VERTEX_POINT ( 'NONE', #21342 ) ;
#33859 = DIRECTION ( 'NONE',  ( 0.5085311186492154079, 0.000000000000000000, 0.8610436117673585521 ) ) ;
#33860 = CARTESIAN_POINT ( 'NONE',  ( -336.3521761649654422, -159.1821513111375452, -47.06073758877369073 ) ) ;
#33861 = PLANE ( 'NONE',  #17343 ) ;
#33862 = ORIENTED_EDGE ( 'NONE', *, *, #16794, .F. ) ;
#33863 = EDGE_CURVE ( 'NONE', #50025, #37621, #5060, .T. ) ;
#33864 = DIRECTION ( 'NONE',  ( -0.000000000000000000, 1.000000000000000000, -0.000000000000000000 ) ) ;
#33865 = LINE ( 'NONE', #13906, #41248 ) ;
#33866 = ORIENTED_EDGE ( 'NONE', *, *, #41424, .T. ) ;
#33867 = EDGE_LOOP ( 'NONE', ( #34251, #2775, #48531, #19461 ) ) ;
#33868 = VECTOR ( 'NONE', #22665, 1000.000000000000000 ) ;
#33869 = ORIENTED_EDGE ( 'NONE', *, *, #555, .T. ) ;
#33870 = CARTESIAN_POINT ( 'NONE',  ( 67.29303306501927295, -175.3837268820161057, 47.13604789772129777 ) ) ;
#33871 = VECTOR ( 'NONE', #23821, 1000.000000000000000 ) ;
#33872 = CARTESIAN_POINT ( 'NONE',  ( -330.4913330509368166, -108.8949048983204904, 57.16590939599316812 ) ) ;
#33873 = DIRECTION ( 'NONE',  ( -1.000000000000000000, -1.258058860540533984E-15, -1.036104688092336048E-14 ) ) ;
#33874 = DIRECTION ( 'NONE',  ( 0.000000000000000000, -0.000000000000000000, 1.000000000000000000 ) ) ;
#33875 = CARTESIAN_POINT ( 'NONE',  ( 60.90550954139435902, -193.5000000000000000, 60.49794494914085874 ) ) ;
#33876 = EDGE_LOOP ( 'NONE', ( #46582, #49587, #30034, #39761 ) ) ;
#33877 = CARTESIAN_POINT ( 'NONE',  ( -238.7407812814481076, -213.5000000000000000, -41.45482488023466061 ) ) ;
#33878 = EDGE_LOOP ( 'NONE', ( #2261, #31459, #7162, #17173 ) ) ;
#33879 = CARTESIAN_POINT ( 'NONE',  ( -129.3001299485802917, -193.5000000000000000, -94.04236105995796891 ) ) ;
#33880 = ORIENTED_EDGE ( 'NONE', *, *, #31286, .T. ) ;
#33881 = FACE_OUTER_BOUND ( 'NONE', #3796, .T. ) ;
#33882 = VECTOR ( 'NONE', #31976, 1000.000000000000114 ) ;
#33883 = ADVANCED_FACE ( 'NONE', ( #13205 ), #9262, .T. ) ;
#33884 = ORIENTED_EDGE ( 'NONE', *, *, #43033, .F. ) ;
#33885 = AXIS2_PLACEMENT_3D ( 'NONE', #50422, #35396, #43035 ) ;
#33886 = DIRECTION ( 'NONE',  ( -0.7948544414133608127, 0.000000000000000000, 0.6068001458185834363 ) ) ;
#33887 = DIRECTION ( 'NONE',  ( 0.000000000000000000, 0.9927088740980556381, 0.1205366802553095168 ) ) ;
#33888 = ORIENTED_EDGE ( 'NONE', *, *, #27553, .F. ) ;
#33891 = ORIENTED_EDGE ( 'NONE', *, *, #52012, .F. ) ;
#33890 = CARTESIAN_POINT ( 'NONE',  ( -22.44626007086657182, -193.5000000000000000, 122.2591094863196730 ) ) ;
#33889 = CARTESIAN_POINT ( 'NONE',  ( -1.162868876050039635, 58.00636336259468351, -16.50905505121457750 ) ) ;
#33892 = DIRECTION ( 'NONE',  ( 0.9842305779475954974, 0.000000000000000000, 0.1768902751225803205 ) ) ;
#33893 = ORIENTED_EDGE ( 'NONE', *, *, #23067, .F. ) ;
#33894 = CARTESIAN_POINT ( 'NONE',  ( -108.0638572795231909, -177.1207230881787780, 108.7464374498172646 ) ) ;
#33895 = ORIENTED_EDGE ( 'NONE', *, *, #45894, .T. ) ;
#33896 = ADVANCED_FACE ( 'NONE', ( #48688 ), #1366, .F. ) ;
#33897 = CARTESIAN_POINT ( 'NONE',  ( -130.2106798473772642, -189.7472609257535510, 94.57776286494221551 ) ) ;
#33900 = ORIENTED_EDGE ( 'NONE', *, *, #9171, .F. ) ;
#33899 = DIRECTION ( 'NONE',  ( -1.000000000000000000, -0.000000000000000000, -0.000000000000000000 ) ) ;
#33898 = LINE ( 'NONE', #814, #3107 ) ;
#33901 = CIRCLE ( 'NONE', #39773, 60.00000000000000000 ) ;
#33902 = ORIENTED_EDGE ( 'NONE', *, *, #25688, .T. ) ;
#33903 = EDGE_CURVE ( 'NONE', #37732, #1758, #25283, .T. ) ;
#33904 = LINE ( 'NONE', #10257, #7235 ) ;
#33905 = ORIENTED_EDGE ( 'NONE', *, *, #46090, .T. ) ;
#33906 = LINE ( 'NONE', #17647, #43788 ) ;
#33907 = EDGE_CURVE ( 'NONE', #48520, #36852, #32647, .T. ) ;
#33908 = DIRECTION ( 'NONE',  ( 0.000000000000000000, 0.000000000000000000, 1.000000000000000000 ) ) ;
#33909 = ORIENTED_EDGE ( 'NONE', *, *, #48158, .F. ) ;
#33910 = CARTESIAN_POINT ( 'NONE',  ( -238.7407812814481076, -213.5000000000000000, -41.45482488023466061 ) ) ;
#33911 = DIRECTION ( 'NONE',  ( 0.000000000000000000, 0.000000000000000000, 1.000000000000000000 ) ) ;
#33912 = DIRECTION ( 'NONE',  ( -0.000000000000000000, 0.1205366802553233113, 0.9927088740980539727 ) ) ;
#33913 = DIRECTION ( 'NONE',  ( -0.2920567706369694982, 0.000000000000000000, -0.9564009842765243130 ) ) ;
#33914 = ORIENTED_EDGE ( 'NONE', *, *, #19463, .F. ) ;
#33915 = CARTESIAN_POINT ( 'NONE',  ( -332.3517673607765914, -66.84097189748108292, 19.74220186498880736 ) ) ;
#33916 = LINE ( 'NONE', #13698, #19725 ) ;
#33917 = DIRECTION ( 'NONE',  ( 1.000000000000000000, -0.000000000000000000, 0.000000000000000000 ) ) ;
#33918 = VERTEX_POINT ( 'NONE', #29472 ) ;
#33919 = CARTESIAN_POINT ( 'NONE',  ( -160.9694636715425702, -193.5000000000000000, 54.50618404931040573 ) ) ;
#33920 = CARTESIAN_POINT ( 'NONE',  ( -336.3521761649654422, -66.84438072661991725, -16.67542351306652648 ) ) ;
#33921 = VECTOR ( 'NONE', #17164, 1000.000000000000000 ) ;
#33922 = AXIS2_PLACEMENT_3D ( 'NONE', #42831, #35200, #18416 ) ;
#33923 = LINE ( 'NONE', #49714, #29396 ) ;
#33924 = CARTESIAN_POINT ( 'NONE',  ( -339.1964088526558498, -63.50208336950359467, 0.4999999999999543698 ) ) ;
#33925 = FACE_BOUND ( 'NONE', #32254, .T. ) ;
#33926 = DIRECTION ( 'NONE',  ( 0.6528221181905227155, 0.000000000000000000, -0.7575112421616191360 ) ) ;
#33927 = CARTESIAN_POINT ( 'NONE',  ( 55.03325008324586776, -177.1207230881787780, -70.07273251429357686 ) ) ;
#33929 = VERTEX_POINT ( 'NONE', #32894 ) ;
#33928 = DIRECTION ( 'NONE',  ( -0.3202698538628487301, 0.000000000000000000, 0.9473263538541877304 ) ) ;
#33930 = VERTEX_POINT ( 'NONE', #17147 ) ;
#33931 = VECTOR ( 'NONE', #44037, 1000.000000000000114 ) ;
#33932 = CARTESIAN_POINT ( 'NONE',  ( -332.3517673607765914, -77.59233547837267508, 37.15394033962009246 ) ) ;
#33934 = ORIENTED_EDGE ( 'NONE', *, *, #4419, .T. ) ;
#33933 = CARTESIAN_POINT ( 'NONE',  ( -330.4913330509368166, -137.1341532842523918, 57.40522506028099770 ) ) ;
#33935 = ORIENTED_EDGE ( 'NONE', *, *, #1641, .T. ) ;
#33936 = ORIENTED_EDGE ( 'NONE', *, *, #42050, .F. ) ;
#33937 = FACE_OUTER_BOUND ( 'NONE', #1536, .T. ) ;
#33938 = ADVANCED_FACE ( 'NONE', ( #29224 ), #1639, .T. ) ;
#33939 = ADVANCED_FACE ( 'NONE', ( #45280 ), #17675, .F. ) ;
#33940 = EDGE_CURVE ( 'NONE', #47336, #37757, #5325, .T. ) ;
#33941 = CARTESIAN_POINT ( 'NONE',  ( -332.3517673607765914, -183.3224719910990643, -4.612141029301910500 ) ) ;
#33942 = DIRECTION ( 'NONE',  ( 0.000000000000000000, -0.000000000000000000, -1.000000000000000000 ) ) ;
#33943 = ORIENTED_EDGE ( 'NONE', *, *, #15408, .T. ) ;
#33944 = EDGE_CURVE ( 'NONE', #37834, #28928, #29732, .T. ) ;
#33945 = LINE ( 'NONE', #42096, #4150 ) ;
#33946 = FACE_OUTER_BOUND ( 'NONE', #12464, .T. ) ;
#33948 = EDGE_LOOP ( 'NONE', ( #20309, #24627, #28822, #14717 ) ) ;
#33947 = CARTESIAN_POINT ( 'NONE',  ( -153.7737137892885073, -175.3837268820161057, -65.49088066501643368 ) ) ;
#33949 = EDGE_CURVE ( 'NONE', #46831, #3996, #13460, .T. ) ;
#33950 = EDGE_CURVE ( 'NONE', #25168, #37719, #25535, .T. ) ;
#33951 = DIRECTION ( 'NONE',  ( -1.000000000000000000, -0.000000000000000000, -0.000000000000000000 ) ) ;
#33952 = AXIS2_PLACEMENT_3D ( 'NONE', #43075, #46776, #2617 ) ;
#33953 = VERTEX_POINT ( 'NONE', #41558 ) ;
#33954 = DIRECTION ( 'NONE',  ( 0.9473263538541923934, 0.000000000000000000, -0.3202698538628350744 ) ) ;
#33955 = ORIENTED_EDGE ( 'NONE', *, *, #33025, .T. ) ;
#33956 = AXIS2_PLACEMENT_3D ( 'NONE', #13375, #17835, #49894 ) ;
#33957 = DIRECTION ( 'NONE',  ( 0.000000000000000000, -0.000000000000000000, 1.000000000000000000 ) ) ;
#33958 = ADVANCED_FACE ( 'NONE', ( #41046 ), #44739, .T. ) ;
#33959 = CARTESIAN_POINT ( 'NONE',  ( -1.771278280434267272, -177.1207230881787780, -115.9455772817710226 ) ) ;
#33960 = FACE_OUTER_BOUND ( 'NONE', #36454, .T. ) ;
#33961 = CIRCLE ( 'NONE', #48268, 125.0000000000000000 ) ;
#33962 = EDGE_CURVE ( 'NONE', #23668, #12667, #7336, .T. ) ;
#33963 = VERTEX_POINT ( 'NONE', #25038 ) ;
#33964 = EDGE_CURVE ( 'NONE', #15918, #29184, #16636, .T. ) ;
#33965 = EDGE_LOOP ( 'NONE', ( #10109, #19371, #43963, #44395, #401 ) ) ;
#33966 = LINE ( 'NONE', #41864, #32326 ) ;
#33967 = EDGE_CURVE ( 'NONE', #20840, #8243, #4805, .T. ) ;
#33968 = DIRECTION ( 'NONE',  ( 0.000000000000000000, 0.000000000000000000, 1.000000000000000000 ) ) ;
#33969 = VERTEX_POINT ( 'NONE', #29159 ) ;
#33970 = VECTOR ( 'NONE', #33398, 1000.000000000000000 ) ;
#33971 = DIRECTION ( 'NONE',  ( 1.000000000000000000, 0.000000000000000000, 0.000000000000000000 ) ) ;
#33972 = EDGE_CURVE ( 'NONE', #39607, #30848, #13650, .T. ) ;
#33973 = EDGE_LOOP ( 'NONE', ( #13797, #32201, #29302, #29312 ) ) ;
#33974 = FACE_BOUND ( 'NONE', #32256, .T. ) ;
#33975 = VECTOR ( 'NONE', #3509, 1000.000000000000000 ) ;
#33976 = DIRECTION ( 'NONE',  ( 0.000000000000000000, 0.000000000000000000, 1.000000000000000000 ) ) ;
#33977 = PRODUCT_DEFINITION_SHAPE ( 'NONE', 'NONE',  #52043 ) ;
#33978 = ORIENTED_EDGE ( 'NONE', *, *, #24103, .F. ) ;
#33979 = LINE ( 'NONE', #50026, #46745 ) ;
#33980 = ORIENTED_EDGE ( 'NONE', *, *, #14170, .T. ) ;
#33981 = CARTESIAN_POINT ( 'NONE',  ( -332.3517673607765914, -123.5000000000000284, 0.000000000000000000 ) ) ;
#33982 = CARTESIAN_POINT ( 'NONE',  ( -48.47912675150885065, -120.5000000000000284, 14.00000000000001776 ) ) ;
#33983 = FACE_OUTER_BOUND ( 'NONE', #43522, .T. ) ;
#33984 = ORIENTED_EDGE ( 'NONE', *, *, #17724, .T. ) ;
#33985 = CARTESIAN_POINT ( 'NONE',  ( -46.00000000000000711, 0.000000000000000000, -51.00000000000000000 ) ) ;
#33986 = FACE_OUTER_BOUND ( 'NONE', #9033, .T. ) ;
#33987 = CARTESIAN_POINT ( 'NONE',  ( -80.17897391495031911, -177.1207230881787780, 120.9136869416132498 ) ) ;
#33988 = LINE ( 'NONE', #45834, #50929 ) ;
#33989 = ADVANCED_FACE ( 'NONE', ( #37574 ), #21022, .T. ) ;
#33990 = ORIENTED_EDGE ( 'NONE', *, *, #38305, .T. ) ;
#33991 = DIRECTION ( 'NONE',  ( 0.000000000000000000, 1.000000000000000000, -0.000000000000000000 ) ) ;
#33992 = ORIENTED_EDGE ( 'NONE', *, *, #22952, .F. ) ;
#33993 = AXIS2_PLACEMENT_3D ( 'NONE', #10075, #1673, #13757 ) ;
#33994 = DIRECTION ( 'NONE',  ( 0.000000000000000000, 0.000000000000000000, -1.000000000000000000 ) ) ;
#33996 = ORIENTED_EDGE ( 'NONE', *, *, #14250, .F. ) ;
#33995 = DIRECTION ( 'NONE',  ( -0.000000000000000000, -1.000000000000000000, -0.000000000000000000 ) ) ;
#33997 = AXIS2_PLACEMENT_3D ( 'NONE', #43844, #7844, #40668 ) ;
#33998 = VECTOR ( 'NONE', #2574, 1000.000000000000000 ) ;
#33999 = ORIENTED_EDGE ( 'NONE', *, *, #43796, .T. ) ;
#34000 = VECTOR ( 'NONE', #5956, 1000.000000000000000 ) ;
#34001 = EDGE_CURVE ( 'NONE', #26732, #8616, #23284, .T. ) ;
#34002 = CARTESIAN_POINT ( 'NONE',  ( -30.48891621885994496, -183.6283474603465606, -122.6885491605230101 ) ) ;
#34003 = ORIENTED_EDGE ( 'NONE', *, *, #15792, .T. ) ;
#34004 = CARTESIAN_POINT ( 'NONE',  ( 43.33156026654913262, 30.00000000000000355, -51.04247435516399634 ) ) ;
#34005 = AXIS2_PLACEMENT_3D ( 'NONE', #2026, #14141, #41971 ) ;
#34006 = VERTEX_POINT ( 'NONE', #16575 ) ;
#34007 = CARTESIAN_POINT ( 'NONE',  ( -25.72842157752850056, -189.7472609257535510, 121.8950816227734606 ) ) ;
#34008 = DIRECTION ( 'NONE',  ( 1.043714542225393381E-14, 0.9350162426854107256, -0.3546048870425463906 ) ) ;
#34009 = VECTOR ( 'NONE', #25870, 1000.000000000000000 ) ;
#34010 = EDGE_CURVE ( 'NONE', #12556, #9613, #48635, .T. ) ;
#34011 = EDGE_CURVE ( 'NONE', #664, #31150, #35053, .T. ) ;
#34012 = EDGE_CURVE ( 'NONE', #42165, #6625, #41496, .T. ) ;
#34013 = EDGE_CURVE ( 'NONE', #4631, #32588, #25478, .T. ) ;
#34015 = AXIS2_PLACEMENT_3D ( 'NONE', #23437, #19999, #23178 ) ;
#34014 = DIRECTION ( 'NONE',  ( -0.000000000000000000, 1.000000000000000000, -0.000000000000000000 ) ) ;
#34016 = CARTESIAN_POINT ( 'NONE',  ( -332.3517673607765914, -123.5000000000000284, 0.000000000000000000 ) ) ;
#34017 = VERTEX_POINT ( 'NONE', #513 ) ;
#34018 = VERTEX_POINT ( 'NONE', #789 ) ;
#34019 = EDGE_CURVE ( 'NONE', #48867, #21836, #8934, .T. ) ;
#34020 = VERTEX_POINT ( 'NONE', #17613 ) ;
#34021 = VECTOR ( 'NONE', #17045, 1000.000000000000000 ) ;
#34022 = DIRECTION ( 'NONE',  ( 0.000000000000000000, -1.000000000000000000, 0.000000000000000000 ) ) ;
#34023 = FACE_OUTER_BOUND ( 'NONE', #25014, .T. ) ;
#34024 = ADVANCED_FACE ( 'NONE', ( #4475 ), #37303, .F. ) ;
#34025 = EDGE_CURVE ( 'NONE', #23542, #19699, #32499, .T. ) ;
#34026 = CYLINDRICAL_SURFACE ( 'NONE', #26213, 4.000000000000003553 ) ;
#34027 = CARTESIAN_POINT ( 'NONE',  ( -336.3521761649654422, -114.7679482383557144, 58.37307289257701370 ) ) ;
#34028 = VERTEX_POINT ( 'NONE', #32586 ) ;
#34029 = ADVANCED_FACE ( 'NONE', ( #33624 ), #25226, .T. ) ;
#34030 = EDGE_CURVE ( 'NONE', #33013, #50209, #51020, .T. ) ;
#34031 = ORIENTED_EDGE ( 'NONE', *, *, #24184, .T. ) ;
#34033 = EDGE_LOOP ( 'NONE', ( #27226, #14653, #31253, #7356 ) ) ;
#34032 = CARTESIAN_POINT ( 'NONE',  ( -104.9497554727472561, -175.3837268820161057, -110.3950557015148775 ) ) ;
#34034 = CARTESIAN_POINT ( 'NONE',  ( -336.3521761649654422, -65.82380048139334860, 12.53476669029061519 ) ) ;
#34035 = AXIS2_PLACEMENT_3D ( 'NONE', #37862, #9757, #48927 ) ;
#34036 = ADVANCED_FACE ( 'NONE', ( #44943 ), #5263, .T. ) ;
#34037 = DIRECTION ( 'NONE',  ( 0.4827922027307366970, 0.000000000000000000, 0.8757349421956412971 ) ) ;
#34038 = DIRECTION ( 'NONE',  ( 0.9720229140804123036, 0.000000000000000000, -0.2348860457809775759 ) ) ;
#34039 = AXIS2_PLACEMENT_3D ( 'NONE', #39208, #39452, #27372 ) ;
#34040 = VECTOR ( 'NONE', #48412, 1000.000000000000000 ) ;
#34041 = EDGE_CURVE ( 'NONE', #7787, #22679, #40454, .T. ) ;
#34042 = LINE ( 'NONE', #33531, #49754 ) ;
#34043 = DIRECTION ( 'NONE',  ( 0.000000000000000000, -1.346129392433909288E-16, 1.000000000000000000 ) ) ;
#34044 = VERTEX_POINT ( 'NONE', #21805 ) ;
#34045 = DIRECTION ( 'NONE',  ( 0.000000000000000000, -1.000000000000000000, 0.000000000000000000 ) ) ;
#34046 = ORIENTED_EDGE ( 'NONE', *, *, #21077, .T. ) ;
#34047 = EDGE_CURVE ( 'NONE', #16943, #13171, #46491, .T. ) ;
#34048 = VERTEX_POINT ( 'NONE', #29936 ) ;
#34049 = FACE_OUTER_BOUND ( 'NONE', #35808, .T. ) ;
#34050 = VECTOR ( 'NONE', #24999, 1000.000000000000000 ) ;
#34051 = LINE ( 'NONE', #38242, #36206 ) ;
#34052 = ORIENTED_EDGE ( 'NONE', *, *, #6385, .T. ) ;
#34053 = AXIS2_PLACEMENT_3D ( 'NONE', #22963, #2980, #51591 ) ;
#34054 = CARTESIAN_POINT ( 'NONE',  ( -118.9967449635792462, -193.5000000000000000, -103.2098131075562009 ) ) ;
#34055 = CARTESIAN_POINT ( 'NONE',  ( 53.18081239921338721, -175.3837268820161057, -72.73415134495935774 ) ) ;
#34056 = CARTESIAN_POINT ( 'NONE',  ( -336.3521761649654422, -155.6724726690323450, 49.48329383994676078 ) ) ;
#34057 = VECTOR ( 'NONE', #14330, 1000.000000000000000 ) ;
#34058 = CARTESIAN_POINT ( 'NONE',  ( -162.0868781531755474, -183.6283474603465606, -49.69312418816313226 ) ) ;
#34059 = EDGE_CURVE ( 'NONE', #50178, #13839, #14187, .T. ) ;
#34061 = VECTOR ( 'NONE', #5089, 999.9999999999998863 ) ;
#34060 = CARTESIAN_POINT ( 'NONE',  ( 36.10886851198520731, -183.6283474603465606, 92.03190238880812046 ) ) ;
#34062 = ORIENTED_EDGE ( 'NONE', *, *, #27452, .T. ) ;
#34063 = CARTESIAN_POINT ( 'NONE',  ( -339.1964088526558498, -75.22798428563942252, 33.92731199008440512 ) ) ;
#34064 = ORIENTED_EDGE ( 'NONE', *, *, #8092, .F. ) ;
#34065 = EDGE_LOOP ( 'NONE', ( #44285, #22126, #48544, #38926 ) ) ;
#34066 = DIRECTION ( 'NONE',  ( 0.000000000000000000, 0.4647231720437631775, -0.8854560256532126861 ) ) ;
#34067 = ORIENTED_EDGE ( 'NONE', *, *, #1981, .T. ) ;
#34068 = DIRECTION ( 'NONE',  ( 0.6749830015182142207, 0.000000000000000000, -0.7378332790417239107 ) ) ;
#34069 = CIRCLE ( 'NONE', #17276, 125.0000000000000000 ) ;
#34070 = CARTESIAN_POINT ( 'NONE',  ( -260.0000000000000000, -63.50000000000000000, 60.00000000000000711 ) ) ;
#34072 = ORIENTED_EDGE ( 'NONE', *, *, #17202, .T. ) ;
#34071 = DIRECTION ( 'NONE',  ( -0.000000000000000000, 1.000000000000000000, -0.000000000000000000 ) ) ;
#34073 = PLANE ( 'NONE',  #16579 ) ;
#34074 = VECTOR ( 'NONE', #33593, 999.9999999999998863 ) ;
#34075 = VECTOR ( 'NONE', #15011, 1000.000000000000227 ) ;
#34076 = EDGE_CURVE ( 'NONE', #30532, #50591, #41775, .T. ) ;
#34077 = ADVANCED_FACE ( 'NONE', ( #30701 ), #45719, .F. ) ;
#34078 = CARTESIAN_POINT ( 'NONE',  ( -332.3517673607765914, -123.5000000000000284, 0.000000000000000000 ) ) ;
#34079 = CARTESIAN_POINT ( 'NONE',  ( -172.2289551866394106, -175.3837268820161057, -17.63462396184710101 ) ) ;
#34080 = ORIENTED_EDGE ( 'NONE', *, *, #44948, .T. ) ;
#34081 = EDGE_LOOP ( 'NONE', ( #32955, #29901, #44613, #44478 ) ) ;
#34082 = VERTEX_POINT ( 'NONE', #41776 ) ;
#34083 = LINE ( 'NONE', #50134, #20010 ) ;
#34084 = DIRECTION ( 'NONE',  ( -0.7765238627180393038, 0.000000000000000000, -0.6300878435817147682 ) ) ;
#34085 = AXIS2_PLACEMENT_3D ( 'NONE', #20016, #36832, #44456 ) ;
#34086 = DIRECTION ( 'NONE',  ( 1.000000000000000000, -8.654812430365565511E-17, 1.050884489711754678E-17 ) ) ;
#34087 = AXIS2_PLACEMENT_3D ( 'NONE', #33734, #12970, #28995 ) ;
#34088 = LINE ( 'NONE', #42218, #19460 ) ;
#34089 = CARTESIAN_POINT ( 'NONE',  ( -339.1964088526558498, -150.4759391377560576, -52.47426709956116042 ) ) ;
#34090 = VERTEX_POINT ( 'NONE', #1817 ) ;
#34091 = VECTOR ( 'NONE', #2379, 1000.000000000000000 ) ;
#34092 = AXIS2_PLACEMENT_3D ( 'NONE', #11393, #26914, #27430 ) ;
#34093 = DIRECTION ( 'NONE',  ( -0.000000000000000000, 1.000000000000000000, -0.000000000000000000 ) ) ;
#34094 = ORIENTED_EDGE ( 'NONE', *, *, #36588, .T. ) ;
#34096 = ORIENTED_EDGE ( 'NONE', *, *, #13093, .T. ) ;
#34095 = DIRECTION ( 'NONE',  ( 0.9890401873221633666, 0.000000000000000000, 0.1476465640024850756 ) ) ;
#34097 = ORIENTED_EDGE ( 'NONE', *, *, #42376, .F. ) ;
#34098 = PLANE ( 'NONE',  #29988 ) ;
#34099 = ADVANCED_FACE ( 'NONE', ( #9984 ), #26767, .F. ) ;
#34100 = VERTEX_POINT ( 'NONE', #9711 ) ;
#34101 = DIRECTION ( 'NONE',  ( 0.000000000000000000, 1.000000000000000000, 0.000000000000000000 ) ) ;
#34102 = ORIENTED_EDGE ( 'NONE', *, *, #43287, .T. ) ;
#34103 = CARTESIAN_POINT ( 'NONE',  ( -81.70897914701313880, -177.1207230881787780, -120.5021863277716534 ) ) ;
#34104 = DIRECTION ( 'NONE',  ( -0.000000000000000000, -1.000000000000000000, 0.000000000000000000 ) ) ;
#34105 = VERTEX_POINT ( 'NONE', #39553 ) ;
#34106 = DIRECTION ( 'NONE',  ( -1.000000000000000000, 0.000000000000000000, 0.000000000000000000 ) ) ;
#34107 = ORIENTED_EDGE ( 'NONE', *, *, #313, .T. ) ;
#34108 = EDGE_CURVE ( 'NONE', #30169, #25631, #10474, .T. ) ;
#34109 = ORIENTED_EDGE ( 'NONE', *, *, #35560, .T. ) ;
#34110 = CARTESIAN_POINT ( 'NONE',  ( -339.1964088526558498, -73.83865025250327108, -33.67120938215323633 ) ) ;
#34111 = AXIS2_PLACEMENT_3D ( 'NONE', #29917, #45978, #50427 ) ;
#34112 = DIRECTION ( 'NONE',  ( -0.5085311186492216251, 0.000000000000000000, 0.8610436117673548884 ) ) ;
#34113 = AXIS2_PLACEMENT_3D ( 'NONE', #23571, #39586, #28289 ) ;
#34114 = CARTESIAN_POINT ( 'NONE',  ( -59.28786813212838069, -193.5000000000000000, 124.5318076226587323 ) ) ;
#34115 = ORIENTED_EDGE ( 'NONE', *, *, #30406, .F. ) ;
#34116 = DIRECTION ( 'NONE',  ( -0.000000000000000000, -0.8854560256532062468, 0.4647231720437755564 ) ) ;
#34117 = LINE ( 'NONE', #18091, #24770 ) ;
#34118 = AXIS2_PLACEMENT_3D ( 'NONE', #30488, #42834, #6328 ) ;
#34119 = LINE ( 'NONE', #9435, #48986 ) ;
#34120 = DIRECTION ( 'NONE',  ( -0.000000000000000000, 0.4647231720437789981, 0.8854560256532044704 ) ) ;
#34121 = ORIENTED_EDGE ( 'NONE', *, *, #21491, .T. ) ;
#34122 = FACE_OUTER_BOUND ( 'NONE', #1689, .T. ) ;
#34123 = CARTESIAN_POINT ( 'NONE',  ( -47.49008656418669005, -193.5000000000000000, 0.1476465640024920423 ) ) ;
#34124 = CARTESIAN_POINT ( 'NONE',  ( 27.42205759510524032, -175.3837268820161057, 98.05618656931997634 ) ) ;
#34125 = VERTEX_POINT ( 'NONE', #37820 ) ;
#34126 = EDGE_LOOP ( 'NONE', ( #35228, #22911, #31287, #5109 ) ) ;
#34127 = AXIS2_PLACEMENT_3D ( 'NONE', #8247, #32417, #25320 ) ;
#34128 = VECTOR ( 'NONE', #45590, 1000.000000000000000 ) ;
#34129 = CARTESIAN_POINT ( 'NONE',  ( -336.3521761649654422, -173.5513585866778214, -31.34948880313881503 ) ) ;
#34130 = VECTOR ( 'NONE', #33358, 1000.000000000000000 ) ;
#34131 = CIRCLE ( 'NONE', #45063, 125.0000000000000000 ) ;
#34132 = CYLINDRICAL_SURFACE ( 'NONE', #30296, 125.0000000000000000 ) ;
#34133 = VERTEX_POINT ( 'NONE', #2070 ) ;
#34134 = FACE_OUTER_BOUND ( 'NONE', #43825, .T. ) ;
#34135 = AXIS2_PLACEMENT_3D ( 'NONE', #34016, #17744, #38481 ) ;
#34136 = ORIENTED_EDGE ( 'NONE', *, *, #13638, .F. ) ;
#34137 = AXIS2_PLACEMENT_3D ( 'NONE', #5090, #37659, #50014 ) ;
#34138 = DIRECTION ( 'NONE',  ( -0.000000000000000000, 1.000000000000000000, -0.000000000000000000 ) ) ;
#34139 = DIRECTION ( 'NONE',  ( 0.000000000000000000, 0.000000000000000000, -1.000000000000000000 ) ) ;
#34140 = CYLINDRICAL_SURFACE ( 'NONE', #14528, 125.0000000000000000 ) ;
#34141 = CARTESIAN_POINT ( 'NONE',  ( -15.24927435600541692, -177.1207230881787780, 120.5021863277719234 ) ) ;
#34142 = EDGE_CURVE ( 'NONE', #16904, #1525, #22306, .T. ) ;
#34143 = DIRECTION ( 'NONE',  ( 0.000000000000000000, 0.1205366802553095307, -0.9927088740980556381 ) ) ;
#34144 = EDGE_LOOP ( 'NONE', ( #45957, #15299, #29605, #3265 ) ) ;
#34145 = DIRECTION ( 'NONE',  ( -0.9785564922995017012, 0.000000000000000000, -0.2059786187411094538 ) ) ;
#34146 = ORIENTED_EDGE ( 'NONE', *, *, #49889, .T. ) ;
#34147 = DIRECTION ( 'NONE',  ( 0.000000000000000000, 1.000000000000000000, 0.000000000000000000 ) ) ;
#34148 = AXIS2_PLACEMENT_3D ( 'NONE', #30306, #6153, #25855 ) ;
#34149 = ORIENTED_EDGE ( 'NONE', *, *, #50526, .F. ) ;
#34150 = CARTESIAN_POINT ( 'NONE',  ( 0.000000000000000000, -53.50000000000000000, -20.00000000000000000 ) ) ;
#34151 = VECTOR ( 'NONE', #42915, 1000.000000000000000 ) ;
#34152 = FACE_OUTER_BOUND ( 'NONE', #45357, .T. ) ;
#34153 = CARTESIAN_POINT ( 'NONE',  ( 46.00000000000000000, 0.000000000000000000, -4.999999999999997335 ) ) ;
#34154 = EDGE_LOOP ( 'NONE', ( #20767, #18341, #41541, #28358 ) ) ;
#34157 = ORIENTED_EDGE ( 'NONE', *, *, #7258, .F. ) ;
#34156 = DIRECTION ( 'NONE',  ( 0.000000000000000000, 0.000000000000000000, 1.000000000000000000 ) ) ;
#34155 = CARTESIAN_POINT ( 'NONE',  ( -3.368532359847667301, 56.71706743982079502, -17.05735933465977894 ) ) ;
#34158 = VECTOR ( 'NONE', #38938, 1000.000000000000000 ) ;
#34159 = CIRCLE ( 'NONE', #11495, 60.00000000000000000 ) ;
#34160 = EDGE_CURVE ( 'NONE', #30471, #17498, #22052, .T. ) ;
#34161 = CIRCLE ( 'NONE', #42557, 125.0000000000000000 ) ;
#34162 = LINE ( 'NONE', #30220, #4644 ) ;
#34164 = ORIENTED_EDGE ( 'NONE', *, *, #23749, .F. ) ;
#34163 = VECTOR ( 'NONE', #12389, 1000.000000000000000 ) ;
#34165 = CARTESIAN_POINT ( 'NONE',  ( -47.49008656418669005, -177.1207230881787780, -0.1476465640024710591 ) ) ;
#34166 = ORIENTED_EDGE ( 'NONE', *, *, #47505, .T. ) ;
#34167 = CIRCLE ( 'NONE', #7315, 125.0000000000000000 ) ;
#34168 = LINE ( 'NONE', #6058, #45185 ) ;
#34171 = ORIENTED_EDGE ( 'NONE', *, *, #11651, .F. ) ;
#34170 = FACE_OUTER_BOUND ( 'NONE', #39713, .T. ) ;
#34169 = LINE ( 'NONE', #22333, #43402 ) ;
#34172 = ORIENTED_EDGE ( 'NONE', *, *, #5451, .F. ) ;
#34173 = AXIS2_PLACEMENT_3D ( 'NONE', #30993, #30726, #38617 ) ;
#34174 = DIRECTION ( 'NONE',  ( -0.000000000000000000, 1.000000000000000000, -0.000000000000000000 ) ) ;
#34175 = VERTEX_POINT ( 'NONE', #22583 ) ;
#34176 = DIRECTION ( 'NONE',  ( 0.000000000000000000, 0.000000000000000000, -1.000000000000000000 ) ) ;
#34177 = PLANE ( 'NONE',  #17329 ) ;
#34178 = ORIENTED_EDGE ( 'NONE', *, *, #33725, .T. ) ;
#34179 = CARTESIAN_POINT ( 'NONE',  ( -121.1142239062970276, -183.6283474603465606, 101.7307360698549417 ) ) ;
#34180 = CARTESIAN_POINT ( 'NONE',  ( -105.7090724259147976, -189.7472609257535510, 111.1293539894142839 ) ) ;
#34181 = CARTESIAN_POINT ( 'NONE',  ( 55.35935253854128746, -177.1207230881787780, 69.58857822035042773 ) ) ;
#34182 = CARTESIAN_POINT ( 'NONE',  ( -76.79768193946081567, -175.3837268820161057, 120.7230919990160629 ) ) ;
#34183 = FACE_BOUND ( 'NONE', #2119, .T. ) ;
#34184 = ORIENTED_EDGE ( 'NONE', *, *, #8663, .F. ) ;
#34185 = DIRECTION ( 'NONE',  ( -0.000000000000000000, 1.000000000000000000, -0.000000000000000000 ) ) ;
#34186 = LINE ( 'NONE', #42838, #51716 ) ;
#34187 = DIRECTION ( 'NONE',  ( -0.9890401873221623674, 0.000000000000000000, -0.1476465640024917925 ) ) ;
#34188 = ORIENTED_EDGE ( 'NONE', *, *, #9303, .F. ) ;
#34189 = AXIS2_PLACEMENT_3D ( 'NONE', #20389, #39828, #4121 ) ;
#34190 = VECTOR ( 'NONE', #35218, 1000.000000000000114 ) ;
#34191 = CARTESIAN_POINT ( 'NONE',  ( 5.139251539934009294, -177.1207230881787780, 111.8087531435658093 ) ) ;
#34192 = CARTESIAN_POINT ( 'NONE',  ( -339.1964088526558498, -66.33409060400650503, 14.60509510167813474 ) ) ;
#34193 = AXIS2_PLACEMENT_3D ( 'NONE', #12486, #15927, #31936 ) ;
#34194 = DIRECTION ( 'NONE',  ( -0.5586467658036594619, 0.000000000000000000, 0.8294056854501971054 ) ) ;
#34195 = ADVANCED_FACE ( 'NONE', ( #46755 ), #25742, .T. ) ;
#34196 = DIRECTION ( 'NONE',  ( 0.4300652022765245608, 0.000000000000000000, -0.9027978299657416494 ) ) ;
#34197 = DIRECTION ( 'NONE',  ( 0.000000000000000000, -0.9927088740980544168, -0.1205366802553199113 ) ) ;
#34198 = EDGE_CURVE ( 'NONE', #1575, #46127, #10220, .T. ) ;
#34199 = VECTOR ( 'NONE', #36082, 1000.000000000000000 ) ;
#34200 = VECTOR ( 'NONE', #51543, 1000.000000000000000 ) ;
#34201 = FACE_OUTER_BOUND ( 'NONE', #40588, .T. ) ;
#34202 = CARTESIAN_POINT ( 'NONE',  ( -128.2395503755045638, -177.1207230881787780, -96.24590808611421267 ) ) ;
#34203 = DIRECTION ( 'NONE',  ( 0.000000000000000000, 0.2393156642875482742, -0.9709418174260544543 ) ) ;
#34204 = AXIS2_PLACEMENT_3D ( 'NONE', #8557, #20653, #8819 ) ;
#34205 = ORIENTED_EDGE ( 'NONE', *, *, #11407, .T. ) ;
#34206 = ADVANCED_FACE ( 'NONE', ( #38335 ), #5794, .F. ) ;
#34207 = AXIS2_PLACEMENT_3D ( 'NONE', #2631, #23129, #50733 ) ;
#34208 = CARTESIAN_POINT ( 'NONE',  ( 0.5906848879318955525, 50.61712177749316055, -21.34592841102499250 ) ) ;
#34209 = EDGE_CURVE ( 'NONE', #11713, #27333, #18382, .T. ) ;
#34210 = AXIS2_PLACEMENT_3D ( 'NONE', #43900, #525, #12086 ) ;
#34211 = CARTESIAN_POINT ( 'NONE',  ( -330.4913330509368166, -182.0095552316576573, -7.608018572112656308 ) ) ;
#34213 = EDGE_LOOP ( 'NONE', ( #11021, #51656, #48320, #43524 ) ) ;
#34212 = DIRECTION ( 'NONE',  ( -0.000000000000000000, -1.000000000000000000, 0.000000000000000000 ) ) ;
#34214 = EDGE_LOOP ( 'NONE', ( #4770, #26167, #28200, #20958 ) ) ;
#34215 = ADVANCED_FACE ( 'NONE', ( #19593 ), #50445, .F. ) ;
#34216 = VERTEX_POINT ( 'NONE', #2598 ) ;
#34217 = PLANE ( 'NONE',  #40144 ) ;
#34218 = DIRECTION ( 'NONE',  ( 0.9027978299657477557, 0.000000000000000000, -0.4300652022765115712 ) ) ;
#34219 = DIRECTION ( 'NONE',  ( -0.000000000000000000, 1.000000000000000000, -0.000000000000000000 ) ) ;
#34220 = ORIENTED_EDGE ( 'NONE', *, *, #45601, .F. ) ;
#34221 = CARTESIAN_POINT ( 'NONE',  ( -161.6832731452239784, -175.3837268820161057, -53.00774697410100345 ) ) ;
#34222 = CARTESIAN_POINT ( 'NONE',  ( -180.0000000000000568, -123.5000000000000284, 15.24495751795539000 ) ) ;
#34223 = VECTOR ( 'NONE', #22988, 1000.000000000000000 ) ;
#34225 = ORIENTED_EDGE ( 'NONE', *, *, #51330, .T. ) ;
#34224 = DIRECTION ( 'NONE',  ( -0.000000000000000000, -0.8229838658936536877, 0.5680647467311596976 ) ) ;
#34226 = VECTOR ( 'NONE', #51760, 1000.000000000000000 ) ;
#34227 = EDGE_CURVE ( 'NONE', #26284, #25732, #40066, .T. ) ;
#34228 = CARTESIAN_POINT ( 'NONE',  ( -4.176930889631405464, -193.5000000000000000, 116.8859077982279615 ) ) ;
#34229 = ORIENTED_EDGE ( 'NONE', *, *, #43483, .F. ) ;
#34230 = CARTESIAN_POINT ( 'NONE',  ( -156.2577088867455473, -183.6283474603465606, -63.31490529818422885 ) ) ;
#34231 = VECTOR ( 'NONE', #29021, 1000.000000000000000 ) ;
#34232 = ORIENTED_EDGE ( 'NONE', *, *, #22387, .T. ) ;
#34233 = DIRECTION ( 'NONE',  ( -0.000000000000000000, 0.9709418174260553425, 0.2393156642875449158 ) ) ;
#34234 = CARTESIAN_POINT ( 'NONE',  ( 75.67769207106684348, -193.5000000000000000, 14.49428645563876650 ) ) ;
#34235 = LINE ( 'NONE', #15051, #48393 ) ;
#34236 = VECTOR ( 'NONE', #38718, 1000.000000000000000 ) ;
#34237 = ORIENTED_EDGE ( 'NONE', *, *, #28367, .T. ) ;
#34238 = CARTESIAN_POINT ( 'NONE',  ( -155.0851258170080769, -183.6283474603465606, 63.33473559879983128 ) ) ;
#34239 = PLANE ( 'NONE',  #1507 ) ;
#34240 = ORIENTED_EDGE ( 'NONE', *, *, #40350, .T. ) ;
#34241 = CARTESIAN_POINT ( 'NONE',  ( -113.5519059482138573, -193.5000000000000000, 105.5544085257715494 ) ) ;
#34242 = ORIENTED_EDGE ( 'NONE', *, *, #39785, .F. ) ;
#34243 = FACE_BOUND ( 'NONE', #35571, .T. ) ;
#34244 = LINE ( 'NONE', #6397, #16415 ) ;
#34245 = CIRCLE ( 'NONE', #51890, 125.0000000000000000 ) ;
#34246 = ORIENTED_EDGE ( 'NONE', *, *, #7819, .F. ) ;
#34247 = CARTESIAN_POINT ( 'NONE',  ( -339.1964088526558498, -64.50000000000000000, 0.4999999999999543698 ) ) ;
#34248 = VERTEX_POINT ( 'NONE', #14686 ) ;
#34249 = CARTESIAN_POINT ( 'NONE',  ( -60.00000000000000000, -63.50000000000000000, -60.00000000000000711 ) ) ;
#34250 = CARTESIAN_POINT ( 'NONE',  ( -336.3521761649654422, -78.25545813661345562, 37.90245108779119931 ) ) ;
#34251 = ORIENTED_EDGE ( 'NONE', *, *, #3057, .F. ) ;
#34252 = DIRECTION ( 'NONE',  ( 0.000000000000000000, 0.8854560256532110207, 0.4647231720437664526 ) ) ;
#34253 = ADVANCED_FACE ( 'NONE', ( #40853 ), #32461, .F. ) ;
#34254 = CARTESIAN_POINT ( 'NONE',  ( -330.4913330509368166, -180.9052250602807703, 13.63415328425337236 ) ) ;
#34255 = CARTESIAN_POINT ( 'NONE',  ( -46.06708674231131084, -183.6283474603465606, -124.9767260852756863 ) ) ;
#34256 = EDGE_CURVE ( 'NONE', #14713, #8894, #17444, .T. ) ;
#34257 = EDGE_LOOP ( 'NONE', ( #16594, #18586, #4896, #2605 ) ) ;
#34258 = FACE_OUTER_BOUND ( 'NONE', #47545, .T. ) ;
#34259 = EDGE_LOOP ( 'NONE', ( #10161, #2202, #31026, #14841 ) ) ;
#34260 = AXIS2_PLACEMENT_3D ( 'NONE', #46086, #10069, #48397 ) ;
#34261 = VECTOR ( 'NONE', #28784, 1000.000000000000114 ) ;
#34262 = AXIS2_PLACEMENT_3D ( 'NONE', #44165, #28115, #19991 ) ;
#34263 = DIRECTION ( 'NONE',  ( -0.000000000000000000, 1.000000000000000000, -0.000000000000000000 ) ) ;
#34264 = FACE_OUTER_BOUND ( 'NONE', #14554, .T. ) ;
#34266 = ORIENTED_EDGE ( 'NONE', *, *, #20939, .F. ) ;
#34265 = DIRECTION ( 'NONE',  ( 0.000000000000000000, -1.000000000000000000, 1.047444401652940007E-14 ) ) ;
#34267 = AXIS2_PLACEMENT_3D ( 'NONE', #1647, #33167, #41306 ) ;
#34268 = VERTEX_POINT ( 'NONE', #24319 ) ;
#34269 = CARTESIAN_POINT ( 'NONE',  ( -332.3517673607765914, -104.1045282520827300, -55.74477592174792306 ) ) ;
#34270 = EDGE_CURVE ( 'NONE', #39314, #28401, #27732, .T. ) ;
#34271 = EDGE_CURVE ( 'NONE', #38037, #30945, #43765, .T. ) ;
#34272 = DIRECTION ( 'NONE',  ( -0.6068001458185890984, 0.000000000000000000, -0.7948544414133565938 ) ) ;
#34273 = AXIS2_PLACEMENT_3D ( 'NONE', #18388, #23361, #39369 ) ;
#34274 = VERTEX_POINT ( 'NONE', #11707 ) ;
#34275 = EDGE_CURVE ( 'NONE', #36109, #265, #20908, .T. ) ;
#34276 = DIRECTION ( 'NONE',  ( 0.000000000000000000, 1.000000000000000000, 0.000000000000000000 ) ) ;
#34277 = VERTEX_POINT ( 'NONE', #39804 ) ;
#34278 = CARTESIAN_POINT ( 'NONE',  ( -330.4913330509368166, -109.8658467157464571, 57.40522506028071348 ) ) ;
#34279 = DIRECTION ( 'NONE',  ( -0.000000000000000000, 1.000000000000000000, -0.000000000000000000 ) ) ;
#34280 = ADVANCED_FACE ( 'NONE', ( #12732 ), #28758, .F. ) ;
#34281 = DIRECTION ( 'NONE',  ( 1.043714542225393381E-14, -0.1205366802553233113, -0.9927088740980539727 ) ) ;
#34282 = FACE_OUTER_BOUND ( 'NONE', #8591, .T. ) ;
#34283 = ORIENTED_EDGE ( 'NONE', *, *, #47873, .T. ) ;
#34284 = VERTEX_POINT ( 'NONE', #44026 ) ;
#34285 = ORIENTED_EDGE ( 'NONE', *, *, #32045, .F. ) ;
#34286 = VECTOR ( 'NONE', #44390, 1000.000000000000114 ) ;
#34287 = DIRECTION ( 'NONE',  ( -1.000000000000000000, 0.000000000000000000, 0.000000000000000000 ) ) ;
#34288 = LINE ( 'NONE', #38728, #41137 ) ;
#34289 = CARTESIAN_POINT ( 'NONE',  ( -160.0000000000000284, -123.5000000000000284, -41.63467731922663972 ) ) ;
#34290 = CARTESIAN_POINT ( 'NONE',  ( 45.24245851652179340, -183.6283474603465606, -81.19354792697733103 ) ) ;
#34291 = ORIENTED_EDGE ( 'NONE', *, *, #51644, .F. ) ;
#34292 = DIRECTION ( 'NONE',  ( -0.000000000000000000, 0.9709418174260553425, 0.2393156642875449158 ) ) ;
#34293 = ORIENTED_EDGE ( 'NONE', *, *, #15930, .F. ) ;
#34294 = ORIENTED_EDGE ( 'NONE', *, *, #22523, .F. ) ;
#34295 = LINE ( 'NONE', #10376, #12210 ) ;
#34297 = AXIS2_PLACEMENT_3D ( 'NONE', #205, #16250, #32262 ) ;
#34296 = FACE_OUTER_BOUND ( 'NONE', #3036, .T. ) ;
#34298 = CARTESIAN_POINT ( 'NONE',  ( 46.00000000000000711, -57.64213562373095101, -46.00000000000000000 ) ) ;
#34299 = ADVANCED_BREP_SHAPE_REPRESENTATION ( '', ( #35629, #31742 ), #22569 ) ;
#34300 = AXIS2_PLACEMENT_3D ( 'NONE', #35688, #51741, #7335 ) ;
#34301 = LINE ( 'NONE', #30348, #27894 ) ;
#34302 = DIRECTION ( 'NONE',  ( -0.000000000000000000, 1.000000000000000000, -0.000000000000000000 ) ) ;
#34303 = ORIENTED_EDGE ( 'NONE', *, *, #33665, .T. ) ;
#34304 = CARTESIAN_POINT ( 'NONE',  ( 51.05451324771860300, -193.5000000000000000, 75.61781872352698031 ) ) ;
#34305 = ORIENTED_EDGE ( 'NONE', *, *, #38644, .T. ) ;
#34306 = EDGE_CURVE ( 'NONE', #8881, #33712, #18259, .T. ) ;
#34307 = ORIENTED_EDGE ( 'NONE', *, *, #45261, .F. ) ;
#34308 = PLANE ( 'NONE',  #15370 ) ;
#34309 = AXIS2_PLACEMENT_3D ( 'NONE', #39316, #2295, #6755 ) ;
#34310 = CARTESIAN_POINT ( 'NONE',  ( -305.0000000000000568, -79.68838513426354098, -40.99441916720346057 ) ) ;
#34311 = VERTEX_POINT ( 'NONE', #15669 ) ;
#34312 = ADVANCED_FACE ( 'NONE', ( #16444 ), #16181, .T. ) ;
#34313 = PLANE ( 'NONE',  #25682 ) ;
#34314 = ADVANCED_FACE ( 'NONE', ( #47977 ), #24570, .T. ) ;
#34315 = DIRECTION ( 'NONE',  ( 0.000000000000000000, -0.000000000000000000, -1.000000000000000000 ) ) ;
#34316 = DIRECTION ( 'NONE',  ( 0.000000000000000000, 1.000000000000000000, 0.000000000000000000 ) ) ;
#34317 = EDGE_CURVE ( 'NONE', #25328, #51645, #48241, .T. ) ;
#34318 = DIRECTION ( 'NONE',  ( -0.000000000000000000, -0.1205366802553268363, -0.9927088740980534176 ) ) ;
#34319 = EDGE_CURVE ( 'NONE', #27371, #24196, #15750, .T. ) ;
#34320 = VECTOR ( 'NONE', #20932, 1000.000000000000000 ) ;
#34321 = CARTESIAN_POINT ( 'NONE',  ( 26.70958190211001337, -189.7472609257535510, -99.85818990449013199 ) ) ;
#34322 = EDGE_LOOP ( 'NONE', ( #13956, #45498, #7726, #26582 ) ) ;
#34323 = ADVANCED_FACE ( 'NONE', ( #40080 ), #16713, .T. ) ;
#34324 = CARTESIAN_POINT ( 'NONE',  ( -339.1964088526558498, -172.3400804610910200, 33.10432812419180948 ) ) ;
#34325 = ORIENTED_EDGE ( 'NONE', *, *, #22174, .F. ) ;
#34326 = ORIENTED_EDGE ( 'NONE', *, *, #2238, .F. ) ;
#34327 = CARTESIAN_POINT ( 'NONE',  ( 76.47090317495664635, -193.5000000000000000, -3.534122433557446374 ) ) ;
#34328 = EDGE_CURVE ( 'NONE', #44193, #37366, #35875, .T. ) ;
#34329 = EDGE_LOOP ( 'NONE', ( #14264, #32019, #48717, #42421 ) ) ;
#34330 = ADVANCED_FACE ( 'NONE', ( #44549 ), #47729, .F. ) ;
#34331 = DIRECTION ( 'NONE',  ( 0.000000000000000000, -1.000000000000000000, 0.000000000000000000 ) ) ;
#34332 = ADVANCED_FACE ( 'NONE', ( #44302 ), #388, .T. ) ;
#34333 = DIRECTION ( 'NONE',  ( 0.000000000000000000, 0.000000000000000000, 1.000000000000000000 ) ) ;
#34334 = DIRECTION ( 'NONE',  ( 0.000000000000000000, -6.383782391594650107E-14, -1.000000000000000000 ) ) ;
#34335 = ORIENTED_EDGE ( 'NONE', *, *, #21803, .F. ) ;
#34336 = DIRECTION ( 'NONE',  ( -0.000000000000000000, 1.000000000000000000, 0.000000000000000000 ) ) ;
#34337 = MECHANICAL_DESIGN_GEOMETRIC_PRESENTATION_REPRESENTATION (  '', ( #10041 ), #46957 ) ;
#34338 = EDGE_CURVE ( 'NONE', #25155, #14931, #42593, .T. ) ;
#34339 = FACE_OUTER_BOUND ( 'NONE', #38928, .T. ) ;
#34340 = LINE ( 'NONE', #49858, #19829 ) ;
#34341 = ORIENTED_EDGE ( 'NONE', *, *, #14614, .F. ) ;
#34342 = ORIENTED_EDGE ( 'NONE', *, *, #3741, .F. ) ;
#34343 = ADVANCED_FACE ( 'NONE', ( #1959 ), #9078, .F. ) ;
#34344 = VERTEX_POINT ( 'NONE', #45855 ) ;
#34345 = ADVANCED_FACE ( 'NONE', ( #16962 ), #50060, .T. ) ;
#34346 = LINE ( 'NONE', #31426, #15009 ) ;
#34347 = VECTOR ( 'NONE', #8855, 1000.000000000000000 ) ;
#34348 = LINE ( 'NONE', #30640, #37731 ) ;
#34349 = PRESENTATION_STYLE_ASSIGNMENT (( #17801 ) ) ;
#34350 = DIRECTION ( 'NONE',  ( -1.000000000000000000, 0.000000000000000000, 0.000000000000000000 ) ) ;
#34351 = LINE ( 'NONE', #30146, #33080 ) ;
#34352 = VERTEX_POINT ( 'NONE', #29804 ) ;
#34353 = ADVANCED_FACE ( 'NONE', ( #49282 ), #29296, .F. ) ;
#34354 = CIRCLE ( 'NONE', #31840, 125.0000000000000000 ) ;
#34355 = LINE ( 'NONE', #30650, #38311 ) ;
#34356 = ORIENTED_EDGE ( 'NONE', *, *, #43874, .T. ) ;
#34358 = ORIENTED_EDGE ( 'NONE', *, *, #28541, .T. ) ;
#34357 = DIRECTION ( 'NONE',  ( 1.000000000000000000, -0.000000000000000000, -0.000000000000000000 ) ) ;
#34359 = ORIENTED_EDGE ( 'NONE', *, *, #41431, .F. ) ;
#34360 = FACE_OUTER_BOUND ( 'NONE', #46304, .T. ) ;
#34361 = ORIENTED_EDGE ( 'NONE', *, *, #23749, .T. ) ;
#34362 = DIRECTION ( 'NONE',  ( -0.4300652022765304450, 0.000000000000000000, 0.9027978299657387629 ) ) ;
#34363 = ORIENTED_EDGE ( 'NONE', *, *, #2896, .T. ) ;
#34364 = CARTESIAN_POINT ( 'NONE',  ( -46.00000000000000711, 20.00000000000000000, 5.000000000000006217 ) ) ;
#34365 = DIRECTION ( 'NONE',  ( 0.000000000000000000, -1.000000000000000000, 0.000000000000000000 ) ) ;
#34366 = ORIENTED_EDGE ( 'NONE', *, *, #30117, .F. ) ;
#34367 = FACE_OUTER_BOUND ( 'NONE', #46770, .T. ) ;
#34368 = ORIENTED_EDGE ( 'NONE', *, *, #3903, .T. ) ;
#34369 = VERTEX_POINT ( 'NONE', #5135 ) ;
#34370 = LINE ( 'NONE', #43024, #10266 ) ;
#34371 = FACE_OUTER_BOUND ( 'NONE', #18003, .T. ) ;
#34372 = AXIS2_PLACEMENT_3D ( 'NONE', #49595, #13845, #1225 ) ;
#34373 = LINE ( 'NONE', #2325, #21968 ) ;
#34374 = DIRECTION ( 'NONE',  ( 0.000000000000000000, 0.000000000000000000, 1.000000000000000000 ) ) ;
#34375 = VERTEX_POINT ( 'NONE', #49802 ) ;
#34376 = FACE_OUTER_BOUND ( 'NONE', #50868, .T. ) ;
#34377 = CIRCLE ( 'NONE', #50226, 60.00000000000000000 ) ;
#34378 = DIRECTION ( 'NONE',  ( -1.000000000000000000, 0.000000000000000000, 0.000000000000000000 ) ) ;
#34379 = EDGE_CURVE ( 'NONE', #20132, #50151, #41123, .T. ) ;
#34380 = EDGE_CURVE ( 'NONE', #14469, #41991, #11568, .T. ) ;
#34381 = DIRECTION ( 'NONE',  ( 0.000000000000000000, 0.000000000000000000, 1.000000000000000000 ) ) ;
#34382 = LINE ( 'NONE', #10454, #4426 ) ;
#34383 = ORIENTED_EDGE ( 'NONE', *, *, #13267, .T. ) ;
#34384 = CARTESIAN_POINT ( 'NONE',  ( 72.95485052494851175, -193.5000000000000000, -29.64437826672757481 ) ) ;
#34385 = DIRECTION ( 'NONE',  ( -1.000000000000000000, 0.000000000000000000, 0.000000000000000000 ) ) ;
#34386 = EDGE_CURVE ( 'NONE', #1671, #14956, #33234, .T. ) ;
#34387 = EDGE_CURVE ( 'NONE', #33217, #14916, #5662, .T. ) ;
#34388 = DIRECTION ( 'NONE',  ( 0.000000000000000000, 0.000000000000000000, 1.000000000000000000 ) ) ;
#34389 = ORIENTED_EDGE ( 'NONE', *, *, #40074, .F. ) ;
#34390 = CARTESIAN_POINT ( 'NONE',  ( -339.1964088526558498, -79.66942718702553350, -39.49849221029258928 ) ) ;
#34391 = DIRECTION ( 'NONE',  ( 0.000000000000000000, 0.000000000000000000, 1.000000000000000000 ) ) ;
#34392 = ORIENTED_EDGE ( 'NONE', *, *, #46878, .T. ) ;
#34393 = CARTESIAN_POINT ( 'NONE',  ( 34.93559171950835918, -183.6283474603465606, -93.09664195018497423 ) ) ;
#34394 = ORIENTED_EDGE ( 'NONE', *, *, #12355, .F. ) ;
#34395 = VECTOR ( 'NONE', #5464, 1000.000000000000000 ) ;
#34396 = DIRECTION ( 'NONE',  ( 0.000000000000000000, 0.6631226582407964143, 0.7485107481710999711 ) ) ;
#34397 = EDGE_CURVE ( 'NONE', #20906, #33364, #5394, .T. ) ;
#34398 = CARTESIAN_POINT ( 'NONE',  ( -70.75782287548088334, -189.7472609257535510, 122.9986166548864901 ) ) ;
#34399 = PRODUCT_RELATED_PRODUCT_CATEGORY ( 'part', '', ( #41948 ) ) ;
#34400 = LINE ( 'NONE', #7062, #17042 ) ;
#34401 = CARTESIAN_POINT ( 'NONE',  ( -336.3521761649654422, -182.5000000000000568, 2.632288850093980503 ) ) ;
#34402 = DIRECTION ( 'NONE',  ( 0.000000000000000000, 1.000000000000000000, 0.000000000000000000 ) ) ;
#34403 = VERTEX_POINT ( 'NONE', #46124 ) ;
#34404 = EDGE_CURVE ( 'NONE', #44579, #27840, #21151, .T. ) ;
#34405 = FACE_OUTER_BOUND ( 'NONE', #44289, .T. ) ;
#34406 = VERTEX_POINT ( 'NONE', #10103 ) ;
#34407 = DIRECTION ( 'NONE',  ( -0.000000000000000000, 1.000000000000000000, -0.000000000000000000 ) ) ;
#34408 = VECTOR ( 'NONE', #44426, 1000.000000000000000 ) ;
#34409 = ORIENTED_EDGE ( 'NONE', *, *, #43576, .T. ) ;
#34410 = DIRECTION ( 'NONE',  ( 1.000000000000000000, -0.000000000000000000, -0.000000000000000000 ) ) ;
#34411 = LINE ( 'NONE', #50707, #5781 ) ;
#34412 = DIRECTION ( 'NONE',  ( -0.000000000000000000, -0.8854560256532062468, 0.4647231720437755564 ) ) ;
#34413 = VERTEX_POINT ( 'NONE', #25605 ) ;
#34416 = VERTEX_POINT ( 'NONE', #25111 ) ;
#34415 = PLANE ( 'NONE',  #13837 ) ;
#34414 = DIRECTION ( 'NONE',  ( 0.000000000000000000, 1.000000000000000000, -0.000000000000000000 ) ) ;
#34417 = DIRECTION ( 'NONE',  ( 0.8455960035018199594, 0.000000000000000000, 0.5338233779648003940 ) ) ;
#34418 = ORIENTED_EDGE ( 'NONE', *, *, #49191, .T. ) ;
#34419 = LINE ( 'NONE', #10247, #6286 ) ;
#34420 = ORIENTED_EDGE ( 'NONE', *, *, #34011, .T. ) ;
#34421 = CARTESIAN_POINT ( 'NONE',  ( -40.30502441601360886, -189.7472609257535510, 123.7303097900624920 ) ) ;
#34424 = VERTEX_POINT ( 'NONE', #1167 ) ;
#34423 = DIRECTION ( 'NONE',  ( -0.000000000000000000, 1.000000000000000000, 0.000000000000000000 ) ) ;
#34422 = CARTESIAN_POINT ( 'NONE',  ( -48.47912675150885065, -189.7472609257535510, 6.938893903907228378E-15 ) ) ;
#34425 = VERTEX_POINT ( 'NONE', #26119 ) ;
#34426 = VECTOR ( 'NONE', #39504, 1000.000000000000000 ) ;
#34427 = AXIS2_PLACEMENT_3D ( 'NONE', #31075, #43163, #15847 ) ;
#34428 = CARTESIAN_POINT ( 'NONE',  ( -68.21229068036657850, -193.5000000000000000, -123.4325817657429809 ) ) ;
#34429 = ORIENTED_EDGE ( 'NONE', *, *, #35608, .T. ) ;
#34430 = DIRECTION ( 'NONE',  ( 0.000000000000000000, 1.000000000000000000, 0.000000000000000000 ) ) ;
#34431 = CARTESIAN_POINT ( 'NONE',  ( -169.1033029113419559, -193.5000000000000000, 32.78426643622745473 ) ) ;
#34432 = ORIENTED_EDGE ( 'NONE', *, *, #4271, .F. ) ;
#34433 = DIRECTION ( 'NONE',  ( 0.02963332782254913048, 0.000000000000000000, 0.9995608365087946812 ) ) ;
#34434 = CARTESIAN_POINT ( 'NONE',  ( 74.77174840718836890, -183.6283474603465606, 20.83798868929603643 ) ) ;
#34435 = LINE ( 'NONE', #6596, #44209 ) ;
#34436 = DIRECTION ( 'NONE',  ( 0.000000000000000000, 0.8229838658936634577, 0.5680647467311457088 ) ) ;
#34437 = DIRECTION ( 'NONE',  ( -1.000000000000000000, 0.000000000000000000, -0.000000000000000000 ) ) ;
#34438 = VERTEX_POINT ( 'NONE', #12993 ) ;
#34439 = EDGE_CURVE ( 'NONE', #42496, #35050, #9849, .T. ) ;
#34440 = DIRECTION ( 'NONE',  ( -0.05924062789370006937, 0.000000000000000000, -0.9982437317643222396 ) ) ;
#34441 = LINE ( 'NONE', #2116, #44081 ) ;
#34442 = LINE ( 'NONE', #33666, #39695 ) ;
#34443 = ORIENTED_EDGE ( 'NONE', *, *, #4211, .T. ) ;
#34444 = AXIS2_PLACEMENT_3D ( 'NONE', #4943, #20698, #45153 ) ;
#34445 = LINE ( 'NONE', #51015, #34075 ) ;
#34446 = CARTESIAN_POINT ( 'NONE',  ( 30.00000000000000711, -43.50000000000000000, -30.00000000000000355 ) ) ;
#34447 = CARTESIAN_POINT ( 'NONE',  ( 30.67449672666758431, -193.5000000000000000, 95.45105364470144593 ) ) ;
#34448 = LINE ( 'NONE', #14491, #5657 ) ;
#34449 = EDGE_LOOP ( 'NONE', ( #8847, #5294, #35220, #20612 ) ) ;
#34450 = PLANE ( 'NONE',  #13701 ) ;
#34451 = PRODUCT_DEFINITION ( 'UNKNOWN', '', #32599, #25373 ) ;
#34452 = CARTESIAN_POINT ( 'NONE',  ( -339.1964088526558498, -116.8846903019852164, -58.63009191191289915 ) ) ;
#34453 = EDGE_CURVE ( 'NONE', #34970, #17341, #37434, .T. ) ;
#34454 = PLANE ( 'NONE',  #47230 ) ;
#34455 = LINE ( 'NONE', #30771, #33759 ) ;
#34456 = ORIENTED_EDGE ( 'NONE', *, *, #45162, .F. ) ;
#34457 = DIRECTION ( 'NONE',  ( 0.000000000000000000, 1.000000000000000000, 0.000000000000000000 ) ) ;
#34458 = AXIS2_PLACEMENT_3D ( 'NONE', #1051, #13152, #28640 ) ;
#34459 = AXIS2_PLACEMENT_3D ( 'NONE', #24482, #8715, #40764 ) ;
#34460 = CARTESIAN_POINT ( 'NONE',  ( -130.2106798473772926, -175.3837268820161057, 94.57776286494220130 ) ) ;
#34461 = ORIENTED_EDGE ( 'NONE', *, *, #46073, .T. ) ;
#34462 = ORIENTED_EDGE ( 'NONE', *, *, #11531, .T. ) ;
#34463 = EDGE_LOOP ( 'NONE', ( #13739, #33339, #18350, #21089 ) ) ;
#34464 = CARTESIAN_POINT ( 'NONE',  ( -332.3517673607765914, -64.61288906875131488, 4.498567634385603142 ) ) ;
#34465 = ADVANCED_FACE ( 'NONE', ( #17494 ), #25873, .F. ) ;
#34466 = CARTESIAN_POINT ( 'NONE',  ( -336.3521761649654422, -76.43926241122620979, -35.68215131113738181 ) ) ;
#34467 = FACE_OUTER_BOUND ( 'NONE', #51493, .T. ) ;
#34468 = VERTEX_POINT ( 'NONE', #42148 ) ;
#34469 = FACE_OUTER_BOUND ( 'NONE', #36894, .T. ) ;
#34470 = DIRECTION ( 'NONE',  ( -1.000000000000000000, -0.000000000000000000, -0.000000000000000000 ) ) ;
#34473 = ORIENTED_EDGE ( 'NONE', *, *, #29856, .T. ) ;
#34472 = CARTESIAN_POINT ( 'NONE',  ( -62.32061382540516092, -189.7472609257535510, 123.2250735253144285 ) ) ;
#34471 = LINE ( 'NONE', #26841, #45980 ) ;
#34474 = VECTOR ( 'NONE', #13791, 1000.000000000000000 ) ;
#34475 = CARTESIAN_POINT ( 'NONE',  ( -48.41988612361514299, -193.5000000000000000, -0.9982437317643144681 ) ) ;
#34476 = ORIENTED_EDGE ( 'NONE', *, *, #30958, .T. ) ;
#34477 = FACE_OUTER_BOUND ( 'NONE', #7595, .T. ) ;
#34478 = ORIENTED_EDGE ( 'NONE', *, *, #29822, .F. ) ;
#34479 = DIRECTION ( 'NONE',  ( 1.000000000000000000, -0.000000000000000000, -0.000000000000000000 ) ) ;
#34480 = CARTESIAN_POINT ( 'NONE',  ( -49.29161362951453640, -193.5000000000000000, 0.5829794791144718991 ) ) ;
#34481 = CARTESIAN_POINT ( 'NONE',  ( -44.48323084606168720, -177.1207230881787780, 124.9361149384469769 ) ) ;
#34482 = ADVANCED_FACE ( 'NONE', ( #6173 ), #37954, .F. ) ;
#34483 = ORIENTED_EDGE ( 'NONE', *, *, #2802, .T. ) ;
#34484 = FACE_OUTER_BOUND ( 'NONE', #18821, .T. ) ;
#34485 = PLANE ( 'NONE',  #35082 ) ;
#34486 = VERTEX_POINT ( 'NONE', #2215 ) ;
#34487 = CARTESIAN_POINT ( 'NONE',  ( 72.05536924052414349, -189.7472609257535510, 33.11246405730899056 ) ) ;
#34488 = VECTOR ( 'NONE', #570, 1000.000000000000000 ) ;
#34489 = CARTESIAN_POINT ( 'NONE',  ( -75.48985759771373694, -183.6283474603465606, -122.0467960216648748 ) ) ;
#34490 = ORIENTED_EDGE ( 'NONE', *, *, #32708, .T. ) ;
#34491 = EDGE_CURVE ( 'NONE', #26145, #4313, #9067, .T. ) ;
#34492 = FACE_BOUND ( 'NONE', #9532, .T. ) ;
#34493 = CARTESIAN_POINT ( 'NONE',  ( -339.1964088526558498, -167.9936954712156592, -38.74998146212110584 ) ) ;
#34494 = VECTOR ( 'NONE', #12063, 1000.000000000000000 ) ;
#34495 = VERTEX_POINT ( 'NONE', #6934 ) ;
#34496 = DIRECTION ( 'NONE',  ( -0.000000000000000000, 0.8854560256532093554, -0.4647231720437695057 ) ) ;
#34497 = ORIENTED_EDGE ( 'NONE', *, *, #46571, .T. ) ;
#34498 = EDGE_CURVE ( 'NONE', #15701, #35294, #39250, .T. ) ;
#34499 = DIRECTION ( 'NONE',  ( -0.1182731709213523247, 0.000000000000000000, -0.9929810960135185827 ) ) ;
#34500 = CARTESIAN_POINT ( 'NONE',  ( 30.00000000000000711, -43.50000000000000000, 0.000000000000000000 ) ) ;
#34501 = ORIENTED_EDGE ( 'NONE', *, *, #43355, .T. ) ;
#34502 = DIRECTION ( 'NONE',  ( 0.9646355819083576311, 0.000000000000000000, 0.2635871660690715101 ) ) ;
#34503 = DIRECTION ( 'NONE',  ( 0.000000000000000000, 0.000000000000000000, -1.000000000000000000 ) ) ;
#34504 = DIRECTION ( 'NONE',  ( -0.000000000000000000, 1.000000000000000000, -0.000000000000000000 ) ) ;
#34505 = ORIENTED_EDGE ( 'NONE', *, *, #31463, .T. ) ;
#34506 = DIRECTION ( 'NONE',  ( 0.000000000000000000, -1.000000000000000000, -0.000000000000000000 ) ) ;
#34507 = ORIENTED_EDGE ( 'NONE', *, *, #44228, .T. ) ;
#34508 = DIRECTION ( 'NONE',  ( 1.000000000000000000, 0.000000000000000000, -0.000000000000000000 ) ) ;
#34509 = EDGE_CURVE ( 'NONE', #4643, #8311, #42414, .T. ) ;
#34510 = DIRECTION ( 'NONE',  ( -0.000000000000000000, 1.000000000000000000, -0.000000000000000000 ) ) ;
#34512 = VERTEX_POINT ( 'NONE', #38973 ) ;
#34511 = LINE ( 'NONE', #10346, #2693 ) ;
#34513 = VERTEX_POINT ( 'NONE', #18258 ) ;
#34514 = DIRECTION ( 'NONE',  ( -0.000000000000000000, 1.000000000000000000, -0.000000000000000000 ) ) ;
#34515 = DIRECTION ( 'NONE',  ( 0.4566292373937018145, 0.000000000000000000, 0.8896570909947529859 ) ) ;
#34516 = ORIENTED_EDGE ( 'NONE', *, *, #45270, .T. ) ;
#34517 = DIRECTION ( 'NONE',  ( -0.000000000000000000, 1.000000000000000000, -0.000000000000000000 ) ) ;
#34518 = VERTEX_POINT ( 'NONE', #14571 ) ;
#34519 = LINE ( 'NONE', #51110, #40939 ) ;
#34520 = CARTESIAN_POINT ( 'NONE',  ( -171.0948786228703113, -175.3837268820161057, -18.47640724094507192 ) ) ;
#34521 = VECTOR ( 'NONE', #3805, 999.9999999999998863 ) ;
#34522 = CARTESIAN_POINT ( 'NONE',  ( -339.1964088526558498, -116.7644047441736035, -59.62073260661671981 ) ) ;
#34523 = CARTESIAN_POINT ( 'NONE',  ( -336.3521761649654422, -177.7325358280884586, 23.38292116578760726 ) ) ;
#34524 = VECTOR ( 'NONE', #49318, 1000.000000000000000 ) ;
#34525 = EDGE_LOOP ( 'NONE', ( #47242, #19309, #42714, #49154 ) ) ;
#34526 = EDGE_LOOP ( 'NONE', ( #45816, #46691, #42442, #3812 ) ) ;
#34528 = VERTEX_POINT ( 'NONE', #22966 ) ;
#34527 = AXIS2_PLACEMENT_3D ( 'NONE', #13048, #24123, #40131 ) ;
#34529 = LINE ( 'NONE', #46130, #37540 ) ;
#34530 = FACE_OUTER_BOUND ( 'NONE', #10311, .T. ) ;
#34531 = FACE_OUTER_BOUND ( 'NONE', #48201, .T. ) ;
#34532 = DIRECTION ( 'NONE',  ( -0.6749830015182196608, 0.000000000000000000, 0.7378332790417189146 ) ) ;
#34533 = ORIENTED_EDGE ( 'NONE', *, *, #51573, .T. ) ;
#34534 = EDGE_CURVE ( 'NONE', #1446, #30190, #22708, .T. ) ;
#34535 = EDGE_CURVE ( 'NONE', #19679, #3624, #10619, .T. ) ;
#34536 = LINE ( 'NONE', #30591, #50053 ) ;
#34537 = VECTOR ( 'NONE', #34818, 1000.000000000000000 ) ;
#34538 = ORIENTED_EDGE ( 'NONE', *, *, #31655, .F. ) ;
#34539 = ORIENTED_EDGE ( 'NONE', *, *, #37420, .F. ) ;
#34540 = DIRECTION ( 'NONE',  ( -1.000000000000000000, 0.000000000000000000, -0.000000000000000000 ) ) ;
#34541 = CIRCLE ( 'NONE', #17790, 125.0000000000000000 ) ;
#34542 = CARTESIAN_POINT ( 'NONE',  ( 75.48400724637755843, -183.6283474603465606, -16.06677968424457958 ) ) ;
#34543 = LINE ( 'NONE', #49825, #40081 ) ;
#34544 = DIRECTION ( 'NONE',  ( 0.000000000000000000, 0.000000000000000000, 1.000000000000000000 ) ) ;
#34545 = CARTESIAN_POINT ( 'NONE',  ( -131.8938452225253855, -183.6283474603465606, 93.09664195018558530 ) ) ;
#34546 = ORIENTED_EDGE ( 'NONE', *, *, #45212, .F. ) ;
#34547 = EDGE_CURVE ( 'NONE', #17157, #15990, #18763, .T. ) ;
#34548 = CARTESIAN_POINT ( 'NONE',  ( 20.66186849114819069, -175.3837268820161057, -104.1370384486464928 ) ) ;
#34549 = EDGE_CURVE ( 'NONE', #42116, #19264, #19293, .T. ) ;
#34550 = EDGE_LOOP ( 'NONE', ( #17553, #50901, #13038, #6237 ) ) ;
#34551 = CARTESIAN_POINT ( 'NONE',  ( -19.18792875895802652, -189.7472609257535510, -120.4907712303050715 ) ) ;
#34552 = EDGE_CURVE ( 'NONE', #36214, #46127, #22501, .T. ) ;
#34553 = DIRECTION ( 'NONE',  ( -1.000000000000000000, 0.000000000000000000, 0.000000000000000000 ) ) ;
#34554 = ORIENTED_EDGE ( 'NONE', *, *, #36766, .F. ) ;
#34555 = CIRCLE ( 'NONE', #42103, 125.0000000000000000 ) ;
#34556 = ADVANCED_FACE ( 'NONE', ( #31096 ), #34772, .T. ) ;
#34557 = DIRECTION ( 'NONE',  ( -0.000000000000000000, 1.000000000000000000, 0.000000000000000000 ) ) ;
#34558 = CARTESIAN_POINT ( 'NONE',  ( -155.9155026329808607, -177.1207230881787780, -61.91627321685029983 ) ) ;
#34559 = DIRECTION ( 'NONE',  ( 0.000000000000000000, -1.000000000000000000, 0.000000000000000000 ) ) ;
#34560 = VECTOR ( 'NONE', #38950, 1000.000000000000000 ) ;
#34561 = DIRECTION ( 'NONE',  ( 0.000000000000000000, 0.000000000000000000, -1.000000000000000000 ) ) ;
#34562 = VECTOR ( 'NONE', #12657, 999.9999999999998863 ) ;
#34563 = DIRECTION ( 'NONE',  ( 1.043714542225393223E-14, 0.9709418174260493473, -0.2393156642875685913 ) ) ;
#34564 = ORIENTED_EDGE ( 'NONE', *, *, #36192, .F. ) ;
#34565 = DIRECTION ( 'NONE',  ( 0.000000000000000000, 1.000000000000000000, 0.000000000000000000 ) ) ;
#34566 = EDGE_LOOP ( 'NONE', ( #18408, #20070, #39265, #51648 ) ) ;
#34567 = ORIENTED_EDGE ( 'NONE', *, *, #31161, .F. ) ;
#34568 = CARTESIAN_POINT ( 'NONE',  ( -48.47912675150885065, -175.3837268820161057, 6.938893903907228378E-15 ) ) ;
#34569 = VERTEX_POINT ( 'NONE', #23232 ) ;
#34570 = VECTOR ( 'NONE', #5057, 1000.000000000000000 ) ;
#34571 = DIRECTION ( 'NONE',  ( 1.000000000000000000, -0.000000000000000000, 0.000000000000000000 ) ) ;
#34572 = CIRCLE ( 'NONE', #9425, 125.0000000000000000 ) ;
#34573 = AXIS2_PLACEMENT_3D ( 'NONE', #1710, #13538, #46133 ) ;
#34574 = ORIENTED_EDGE ( 'NONE', *, *, #29331, .T. ) ;
#34575 = CARTESIAN_POINT ( 'NONE',  ( -123.6678354051270077, -189.7472609257535510, 99.85818990449067201 ) ) ;
#34576 = CARTESIAN_POINT ( 'NONE',  ( -332.3517673607765914, -73.21199843436539823, 32.72792230702598459 ) ) ;
#34577 = VERTEX_POINT ( 'NONE', #50832 ) ;
#34578 = FACE_OUTER_BOUND ( 'NONE', #50504, .T. ) ;
#34579 = LINE ( 'NONE', #47461, #898 ) ;
#34580 = DIRECTION ( 'NONE',  ( -0.000000000000000000, 1.000000000000000000, 0.000000000000000000 ) ) ;
#34581 = ORIENTED_EDGE ( 'NONE', *, *, #23081, .T. ) ;
#34582 = VERTEX_POINT ( 'NONE', #38477 ) ;
#34583 = EDGE_LOOP ( 'NONE', ( #41518, #37258, #21563, #28281 ) ) ;
#34584 = DIRECTION ( 'NONE',  ( 0.000000000000000000, -0.8229838658936613482, -0.5680647467311485954 ) ) ;
#34585 = LINE ( 'NONE', #34842, #28483 ) ;
#34586 = FACE_OUTER_BOUND ( 'NONE', #3779, .T. ) ;
#34587 = CARTESIAN_POINT ( 'NONE',  ( -47.55243714407701816, -183.6283474603465606, -0.3758275821142288420 ) ) ;
#34588 = CARTESIAN_POINT ( 'NONE',  ( -336.3521761649654422, -140.1754235130667610, -56.65561927338005432 ) ) ;
#34589 = VECTOR ( 'NONE', #30170, 1000.000000000000227 ) ;
#34590 = ORIENTED_EDGE ( 'NONE', *, *, #41611, .T. ) ;
#34591 = EDGE_CURVE ( 'NONE', #34528, #5079, #9889, .T. ) ;
#34592 = EDGE_CURVE ( 'NONE', #32588, #16076, #18296, .T. ) ;
#34593 = EDGE_CURVE ( 'NONE', #10828, #45319, #2481, .T. ) ;
#34594 = EDGE_CURVE ( 'NONE', #23726, #34940, #48539, .T. ) ;
#34595 = VECTOR ( 'NONE', #24690, 1000.000000000000114 ) ;
#34596 = CARTESIAN_POINT ( 'NONE',  ( -336.3521761649654422, -73.44864141332200802, 31.34948880313848107 ) ) ;
#34597 = EDGE_LOOP ( 'NONE', ( #24865, #8483, #47103, #44280 ) ) ;
#34599 = ORIENTED_EDGE ( 'NONE', *, *, #12917, .F. ) ;
#34598 = DIRECTION ( 'NONE',  ( 0.000000000000000000, 0.000000000000000000, 1.000000000000000000 ) ) ;
#34600 = VERTEX_POINT ( 'NONE', #34520 ) ;
#34601 = EDGE_CURVE ( 'NONE', #41076, #7058, #47669, .T. ) ;
#34602 = CARTESIAN_POINT ( 'NONE',  ( -336.3521761649654422, -135.0638248728647852, 57.91551518289418254 ) ) ;
#34603 = ADVANCED_FACE ( 'NONE', ( #10875, #27150 ), #33421, .T. ) ;
#34604 = EDGE_LOOP ( 'NONE', ( #27717, #16909, #8891, #45868 ) ) ;
#34605 = DIRECTION ( 'NONE',  ( 0.000000000000000000, 0.000000000000000000, -1.000000000000000000 ) ) ;
#34606 = DIRECTION ( 'NONE',  ( -1.000000000000000000, -0.000000000000000000, -0.000000000000000000 ) ) ;
#34607 = CARTESIAN_POINT ( 'NONE',  ( 41.40822382563629134, -193.5000000000000000, 85.41934182508082074 ) ) ;
#34608 = ORIENTED_EDGE ( 'NONE', *, *, #49412, .T. ) ;
#34609 = EDGE_CURVE ( 'NONE', #3937, #5817, #40106, .T. ) ;
#34610 = LINE ( 'NONE', #26467, #16639 ) ;
#34611 = VERTEX_POINT ( 'NONE', #43459 ) ;
#34612 = AXIS2_PLACEMENT_3D ( 'NONE', #51525, #22891, #31539 ) ;
#34613 = AXIS2_PLACEMENT_3D ( 'NONE', #37136, #4308, #49245 ) ;
#34614 = EDGE_CURVE ( 'NONE', #27304, #22201, #14093, .T. ) ;
#34615 = ORIENTED_EDGE ( 'NONE', *, *, #32883, .F. ) ;
#34616 = CARTESIAN_POINT ( 'NONE',  ( -55.05561436132772002, -189.7472609257535510, 124.8268793598474105 ) ) ;
#34617 = CIRCLE ( 'NONE', #18690, 9.999999999999994671 ) ;
#34619 = AXIS2_PLACEMENT_3D ( 'NONE', #5161, #49308, #4904 ) ;
#34618 = CARTESIAN_POINT ( 'NONE',  ( -108.5723883981723930, -193.5000000000000000, 109.6074810615846360 ) ) ;
#34620 = ADVANCED_FACE ( 'NONE', ( #12142 ), #48435, .T. ) ;
#34621 = DIRECTION ( 'NONE',  ( -0.000000000000000000, -1.000000000000000000, 0.000000000000000000 ) ) ;
#34622 = ORIENTED_EDGE ( 'NONE', *, *, #16805, .T. ) ;
#34623 = DIRECTION ( 'NONE',  ( 1.000000000000000000, 0.000000000000000000, -0.000000000000000000 ) ) ;
#34624 = DIRECTION ( 'NONE',  ( -0.05924062789372142729, 0.000000000000000000, 0.9982437317643209074 ) ) ;
#34625 = ADVANCED_FACE ( 'NONE', ( #39736 ), #16115, .F. ) ;
#34626 = PLANE ( 'NONE',  #46475 ) ;
#34627 = CARTESIAN_POINT ( 'NONE',  ( -336.3521761649654422, -100.1170788342122080, 54.23253582808833073 ) ) ;
#34628 = EDGE_LOOP ( 'NONE', ( #45529, #12421, #23802, #37811 ) ) ;
#34629 = DIRECTION ( 'NONE',  ( 0.000000000000000000, 0.000000000000000000, 1.000000000000000000 ) ) ;
#34630 = PLANE ( 'NONE',  #2228 ) ;
#34631 = DIRECTION ( 'NONE',  ( 0.9473263538541899509, 0.000000000000000000, 0.3202698538628415692 ) ) ;
#34632 = ORIENTED_EDGE ( 'NONE', *, *, #16997, .T. ) ;
#34633 = CARTESIAN_POINT ( 'NONE',  ( -330.4913330509368166, -180.9052250602809693, -13.63415328425256945 ) ) ;
#34634 = AXIS2_PLACEMENT_3D ( 'NONE', #3343, #40114, #20146 ) ;
#34635 = CYLINDRICAL_SURFACE ( 'NONE', #25276, 9.999999999999994671 ) ;
#34636 = EDGE_LOOP ( 'NONE', ( #48502, #14920, #26508, #15272 ) ) ;
#34637 = DIRECTION ( 'NONE',  ( 0.000000000000000000, 0.000000000000000000, 1.000000000000000000 ) ) ;
#34638 = ORIENTED_EDGE ( 'NONE', *, *, #34047, .T. ) ;
#34639 = EDGE_CURVE ( 'NONE', #42167, #50918, #4031, .T. ) ;
#34640 = AXIS2_PLACEMENT_3D ( 'NONE', #25223, #48888, #37298 ) ;
#34641 = PLANE ( 'NONE',  #22599 ) ;
#34642 = CARTESIAN_POINT ( 'NONE',  ( -164.2512865680372727, -175.3837268820161057, -47.13604789772047354 ) ) ;
#34643 = DIRECTION ( 'NONE',  ( 0.000000000000000000, 1.000000000000000000, -0.000000000000000000 ) ) ;
#34644 = DIRECTION ( 'NONE',  ( 0.000000000000000000, 1.000000000000000000, -0.000000000000000000 ) ) ;
#34646 = CIRCLE ( 'NONE', #10351, 125.0000000000000000 ) ;
#34645 = DIRECTION ( 'NONE',  ( -0.8455960035018199594, 0.000000000000000000, -0.5338233779648003940 ) ) ;
#34647 = VECTOR ( 'NONE', #22050, 999.9999999999998863 ) ;
#34648 = ORIENTED_EDGE ( 'NONE', *, *, #17181, .F. ) ;
#34649 = DIRECTION ( 'NONE',  ( 0.000000000000000000, -6.245004513516505540E-15, -1.000000000000000000 ) ) ;
#34650 = ORIENTED_EDGE ( 'NONE', *, *, #41670, .T. ) ;
#34651 = EDGE_CURVE ( 'NONE', #3375, #34970, #19523, .T. ) ;
#34652 = CARTESIAN_POINT ( 'NONE',  ( 47.28479244271900939, -175.3837268820161057, -78.77358243914883928 ) ) ;
#34653 = CIRCLE ( 'NONE', #31315, 125.0000000000000000 ) ;
#34654 = ORIENTED_EDGE ( 'NONE', *, *, #19407, .T. ) ;
#34655 = DIRECTION ( 'NONE',  ( -0.000000000000000000, 1.000000000000000000, -0.000000000000000000 ) ) ;
#34656 = EDGE_CURVE ( 'NONE', #29379, #8048, #39496, .T. ) ;
#34657 = EDGE_CURVE ( 'NONE', #6242, #20061, #45167, .T. ) ;
#34658 = EDGE_CURVE ( 'NONE', #23290, #42327, #28691, .T. ) ;
#34659 = AXIS2_PLACEMENT_3D ( 'NONE', #24311, #15660, #47721 ) ;
#34660 = ADVANCED_FACE ( 'NONE', ( #12414 ), #11650, .T. ) ;
#34661 = DIRECTION ( 'NONE',  ( -0.000000000000000000, 1.000000000000000000, -0.000000000000000000 ) ) ;
#34662 = CARTESIAN_POINT ( 'NONE',  ( -332.3517673607765914, -169.4076645216271402, -37.15394033962039089 ) ) ;
#34663 = VERTEX_POINT ( 'NONE', #36075 ) ;
#34665 = ORIENTED_EDGE ( 'NONE', *, *, #33800, .T. ) ;
#34664 = DIRECTION ( 'NONE',  ( 0.000000000000000000, 0.000000000000000000, 1.000000000000000000 ) ) ;
#34666 = FACE_OUTER_BOUND ( 'NONE', #42997, .T. ) ;
#34667 = ORIENTED_EDGE ( 'NONE', *, *, #21032, .T. ) ;
#34668 = LINE ( 'NONE', #6825, #27231 ) ;
#34669 = VECTOR ( 'NONE', #47055, 999.9999999999998863 ) ;
#34670 = ORIENTED_EDGE ( 'NONE', *, *, #14747, .F. ) ;
#34671 = LINE ( 'NONE', #38363, #51077 ) ;
#34674 = EDGE_LOOP ( 'NONE', ( #13632, #27652, #49701, #15200 ) ) ;
#34673 = PLANE ( 'NONE',  #22452 ) ;
#34672 = LINE ( 'NONE', #27041, #29138 ) ;
#34675 = ORIENTED_EDGE ( 'NONE', *, *, #35903, .F. ) ;
#34676 = AXIS2_PLACEMENT_3D ( 'NONE', #1696, #17735, #16955 ) ;
#34677 = FACE_OUTER_BOUND ( 'NONE', #17797, .T. ) ;
#34678 = ORIENTED_EDGE ( 'NONE', *, *, #21985, .T. ) ;
#34679 = CARTESIAN_POINT ( 'NONE',  ( -159.0901268547125653, -183.6283474603465606, 58.22548115875957109 ) ) ;
#34680 = DIRECTION ( 'NONE',  ( 0.000000000000000000, -0.9350162426854107256, 0.3546048870425463906 ) ) ;
#34681 = EDGE_CURVE ( 'NONE', #23911, #21654, #27676, .T. ) ;
#34682 = ORIENTED_EDGE ( 'NONE', *, *, #6024, .T. ) ;
#34683 = CARTESIAN_POINT ( 'NONE',  ( -76.79768193946077304, -193.5000000000000000, 120.7230919990160771 ) ) ;
#34684 = DIRECTION ( 'NONE',  ( 0.000000000000000000, 0.000000000000000000, 1.000000000000000000 ) ) ;
#34685 = PLANE ( 'NONE',  #23256 ) ;
#34686 = DIRECTION ( 'NONE',  ( 1.000000000000000000, -2.086444717177606589E-17, -8.465038975556385201E-17 ) ) ;
#34687 = CARTESIAN_POINT ( 'NONE',  ( 49.10711742958949344, -175.3837268820161057, 78.11481899503480975 ) ) ;
#34688 = ADVANCED_FACE ( 'NONE', ( #28440 ), #3751, .T. ) ;
#34689 = ORIENTED_EDGE ( 'NONE', *, *, #10937, .F. ) ;
#34690 = VECTOR ( 'NONE', #5874, 1000.000000000000114 ) ;
#34691 = CARTESIAN_POINT ( 'NONE',  ( -151.9915035862630646, -177.1207230881787780, 70.07273251429430161 ) ) ;
#34692 = DIRECTION ( 'NONE',  ( 0.000000000000000000, 0.000000000000000000, 1.000000000000000000 ) ) ;
#34693 = ADVANCED_FACE ( 'NONE', ( #23730 ), #24258, .F. ) ;
#34694 = CARTESIAN_POINT ( 'NONE',  ( -48.47912675150885065, -177.1207230881787780, 6.938893903907228378E-15 ) ) ;
#34695 = VERTEX_POINT ( 'NONE', #20297 ) ;
#34696 = AXIS2_PLACEMENT_3D ( 'NONE', #40107, #47757, #3859 ) ;
#34697 = LINE ( 'NONE', #3414, #26526 ) ;
#34698 = DIRECTION ( 'NONE',  ( -0.000000000000000000, 1.000000000000000000, -0.000000000000000000 ) ) ;
#34699 = CARTESIAN_POINT ( 'NONE',  ( 5.542374969221969039, -183.6283474603465606, 112.7238987608088223 ) ) ;
#34700 = CARTESIAN_POINT ( 'NONE',  ( 44.58442300236217903, -193.5000000000000000, -81.94739446021067408 ) ) ;
#34701 = ORIENTED_EDGE ( 'NONE', *, *, #35601, .F. ) ;
#34702 = EDGE_CURVE ( 'NONE', #19264, #7764, #40006, .T. ) ;
#34703 = LINE ( 'NONE', #26817, #2735 ) ;
#34704 = LINE ( 'NONE', #26050, #37913 ) ;
#34705 = LINE ( 'NONE', #49979, #30436 ) ;
#34706 = LINE ( 'NONE', #19454, #23697 ) ;
#34707 = VECTOR ( 'NONE', #6270, 1000.000000000000000 ) ;
#34708 = VERTEX_POINT ( 'NONE', #36330 ) ;
#34709 = LINE ( 'NONE', #37171, #39420 ) ;
#34710 = CIRCLE ( 'NONE', #16266, 125.0000000000000000 ) ;
#34711 = CARTESIAN_POINT ( 'NONE',  ( -336.3521761649654422, -182.5000000000000568, 2.632288850093980503 ) ) ;
#34712 = ORIENTED_EDGE ( 'NONE', *, *, #12235, .F. ) ;
#34713 = EDGE_LOOP ( 'NONE', ( #5229, #51715, #31881, #47257 ) ) ;
#34714 = ORIENTED_EDGE ( 'NONE', *, *, #45658, .T. ) ;
#34715 = CARTESIAN_POINT ( 'NONE',  ( 11.10560377650620723, -193.5000000000000000, -108.7464374498168951 ) ) ;
#34716 = EDGE_CURVE ( 'NONE', #41529, #37529, #51594, .T. ) ;
#34717 = ADVANCED_FACE ( 'NONE', ( #15600 ), #43958, .T. ) ;
#34718 = FACE_OUTER_BOUND ( 'NONE', #22216, .T. ) ;
#34719 = CARTESIAN_POINT ( 'NONE',  ( -49.13194886969938580, -193.5000000000000000, 0.7575112421616214675 ) ) ;
#34721 = EDGE_LOOP ( 'NONE', ( #51403, #21495, #45510, #2148 ) ) ;
#34720 = AXIS2_PLACEMENT_3D ( 'NONE', #4679, #26834, #3631 ) ;
#34722 = LINE ( 'NONE', #26585, #798 ) ;
#34723 = CARTESIAN_POINT ( 'NONE',  ( -336.3521761649654422, -170.5607375887735770, 35.68215131113770155 ) ) ;
#34726 = EDGE_LOOP ( 'NONE', ( #31671, #51789, #20488, #8724 ) ) ;
#34725 = CARTESIAN_POINT ( 'NONE',  ( -56.65322908700500193, -189.7472609257535510, -123.7303097900624351 ) ) ;
#34724 = DIRECTION ( 'NONE',  ( 0.000000000000000000, 0.000000000000000000, -1.000000000000000000 ) ) ;
#34727 = CARTESIAN_POINT ( 'NONE',  ( -336.3521761649654422, -68.38646289696045244, -23.71704087764494062 ) ) ;
#34728 = ORIENTED_EDGE ( 'NONE', *, *, #14442, .F. ) ;
#34729 = PLANE ( 'NONE',  #49915 ) ;
#34730 = ORIENTED_EDGE ( 'NONE', *, *, #3949, .T. ) ;
#34731 = CARTESIAN_POINT ( 'NONE',  ( -339.1964088526558498, -101.7569374291128526, -55.92172413327835301 ) ) ;
#34732 = DIRECTION ( 'NONE',  ( -0.000000000000000000, 1.000000000000000000, -0.000000000000000000 ) ) ;
#34733 = DIRECTION ( 'NONE',  ( 0.000000000000000000, 0.000000000000000000, -1.000000000000000000 ) ) ;
#34734 = VERTEX_POINT ( 'NONE', #36594 ) ;
#34735 = VERTEX_POINT ( 'NONE', #4541 ) ;
#34736 = DIRECTION ( 'NONE',  ( 0.000000000000000000, -1.000000000000000000, 0.000000000000000000 ) ) ;
#34737 = DIRECTION ( 'NONE',  ( -0.9151456172430181280, 0.000000000000000000, -0.4031234292879730674 ) ) ;
#34738 = EDGE_LOOP ( 'NONE', ( #35632, #51825, #23208, #40477 ) ) ;
#34739 = ADVANCED_FACE ( 'NONE', ( #16643 ), #32653, .T. ) ;
#34740 = CARTESIAN_POINT ( 'NONE',  ( -12.76653800058364574, -193.5000000000000000, -119.7898618611244927 ) ) ;
#34741 = VECTOR ( 'NONE', #1209, 999.9999999999998863 ) ;
#34742 = CARTESIAN_POINT ( 'NONE',  ( 0.000000000000000000, -178.6659583184396354, -20.92168833550928042 ) ) ;
#34743 = VECTOR ( 'NONE', #44122, 1000.000000000000000 ) ;
#34744 = EDGE_LOOP ( 'NONE', ( #22647, #27510, #15657, #23384 ) ) ;
#34745 = CARTESIAN_POINT ( 'NONE',  ( -305.0000000000000568, -123.5000000000000284, 0.000000000000000000 ) ) ;
#34747 = VECTOR ( 'NONE', #41676, 1000.000000000000114 ) ;
#34746 = DIRECTION ( 'NONE',  ( -0.000000000000000000, 1.000000000000000000, -0.000000000000000000 ) ) ;
#34748 = EDGE_CURVE ( 'NONE', #10180, #6855, #29200, .T. ) ;
#34749 = ORIENTED_EDGE ( 'NONE', *, *, #31389, .F. ) ;
#34750 = CARTESIAN_POINT ( 'NONE',  ( -167.6453766917639427, -183.6283474603465606, 37.74128873232410086 ) ) ;
#34751 = VERTEX_POINT ( 'NONE', #45288 ) ;
#34752 = CARTESIAN_POINT ( 'NONE',  ( -157.5429198988176438, -189.7472609257535510, 61.07445476073480961 ) ) ;
#34753 = DIRECTION ( 'NONE',  ( -0.000000000000000000, 0.3546048870425331789, -0.9350162426854158326 ) ) ;
#34754 = VERTEX_POINT ( 'NONE', #13212 ) ;
#34755 = FACE_OUTER_BOUND ( 'NONE', #11557, .T. ) ;
#34756 = DIRECTION ( 'NONE',  ( -1.000000000000000000, -0.000000000000000000, 0.000000000000000000 ) ) ;
#34757 = LINE ( 'NONE', #6668, #15663 ) ;
#34758 = CIRCLE ( 'NONE', #37314, 60.00000000000000000 ) ;
#34759 = ORIENTED_EDGE ( 'NONE', *, *, #5448, .T. ) ;
#34760 = CARTESIAN_POINT ( 'NONE',  ( 141.7825277784304205, -213.5000000000000000, 41.45482488023466772 ) ) ;
#34761 = CYLINDRICAL_SURFACE ( 'NONE', #47969, 125.0000000000000000 ) ;
#34762 = CARTESIAN_POINT ( 'NONE',  ( -173.2419626162308646, -183.6283474603465606, 7.696413904698412800 ) ) ;
#34764 = ORIENTED_EDGE ( 'NONE', *, *, #7972, .F. ) ;
#34763 = DIRECTION ( 'NONE',  ( 0.000000000000000000, 0.000000000000000000, 1.000000000000000000 ) ) ;
#34765 = ORIENTED_EDGE ( 'NONE', *, *, #3295, .T. ) ;
#34766 = LINE ( 'NONE', #38197, #24929 ) ;
#34767 = DIRECTION ( 'NONE',  ( 0.9960498426152165630, 0.000000000000000000, 0.08879589532293852283 ) ) ;
#34768 = ORIENTED_EDGE ( 'NONE', *, *, #8602, .F. ) ;
#34769 = DIRECTION ( 'NONE',  ( -0.000000000000000000, 1.000000000000000000, -0.000000000000000000 ) ) ;
#34770 = ORIENTED_EDGE ( 'NONE', *, *, #37525, .F. ) ;
#34771 = DIRECTION ( 'NONE',  ( -0.000000000000000000, 1.000000000000000000, -0.000000000000000000 ) ) ;
#34772 = PLANE ( 'NONE',  #4871 ) ;
#34773 = VECTOR ( 'NONE', #8690, 1000.000000000000114 ) ;
#34774 = VECTOR ( 'NONE', #39482, 1000.000000000000114 ) ;
#34775 = ADVANCED_FACE ( 'NONE', ( #37643 ), #37110, .T. ) ;
#34776 = CARTESIAN_POINT ( 'NONE',  ( -173.4724443937511751, -193.5000000000000000, 1.292495564989516454 ) ) ;
#34777 = CARTESIAN_POINT ( 'NONE',  ( -339.1964088526558498, -64.86990808808717190, -6.615309698015097162 ) ) ;
#34778 = EDGE_LOOP ( 'NONE', ( #20394, #39941, #24197, #49671 ) ) ;
#34779 = EDGE_LOOP ( 'NONE', ( #47629, #50385, #533, #9015 ) ) ;
#34780 = CIRCLE ( 'NONE', #42329, 125.0000000000000000 ) ;
#34781 = ORIENTED_EDGE ( 'NONE', *, *, #15904, .F. ) ;
#34782 = DIRECTION ( 'NONE',  ( -0.000000000000000000, -0.7485107481711046340, -0.6631226582407911962 ) ) ;
#34783 = CARTESIAN_POINT ( 'NONE',  ( -115.4536696835168641, -177.1207230881787780, -105.5434062319793185 ) ) ;
#34784 = EDGE_CURVE ( 'NONE', #17312, #39795, #14963, .T. ) ;
#34785 = CARTESIAN_POINT ( 'NONE',  ( -46.06708674231131084, -183.6283474603465606, -124.9767260852756863 ) ) ;
#34786 = DIRECTION ( 'NONE',  ( 1.000000000000000000, 0.000000000000000000, 0.000000000000000000 ) ) ;
#34787 = ORIENTED_EDGE ( 'NONE', *, *, #47620, .T. ) ;
#34788 = AXIS2_PLACEMENT_3D ( 'NONE', #19305, #47680, #31367 ) ;
#34789 = CARTESIAN_POINT ( 'NONE',  ( 1.734723475976807094E-15, 20.00000000000000000, 46.00000000000000711 ) ) ;
#34790 = DIRECTION ( 'NONE',  ( -0.9266896074318317078, 0.000000000000000000, -0.3758275821142421647 ) ) ;
#34791 = VERTEX_POINT ( 'NONE', #9523 ) ;
#34792 = VERTEX_POINT ( 'NONE', #33451 ) ;
#34793 = LINE ( 'NONE', #46922, #18940 ) ;
#34794 = CARTESIAN_POINT ( 'NONE',  ( -16.10442403432825387, -183.6283474603465606, -119.6996507684850428 ) ) ;
#34795 = LINE ( 'NONE', #7217, #45158 ) ;
#34796 = EDGE_CURVE ( 'NONE', #9382, #24476, #32533, .T. ) ;
#34797 = CARTESIAN_POINT ( 'NONE',  ( -180.0000000000000568, -123.5000000000000284, 6.938893903907228378E-15 ) ) ;
#34798 = DIRECTION ( 'NONE',  ( -0.000000000000000000, 1.000000000000000000, -0.000000000000000000 ) ) ;
#34799 = DIRECTION ( 'NONE',  ( 0.000000000000000000, 0.8660254037844379305, 0.5000000000000011102 ) ) ;
#34800 = ORIENTED_EDGE ( 'NONE', *, *, #10006, .T. ) ;
#34801 = DIRECTION ( 'NONE',  ( -0.000000000000000000, 0.7485107481711089639, 0.6631226582407863113 ) ) ;
#34802 = ORIENTED_EDGE ( 'NONE', *, *, #49157, .T. ) ;
#34803 = DIRECTION ( 'NONE',  ( -0.000000000000000000, 1.000000000000000000, -0.000000000000000000 ) ) ;
#34804 = VECTOR ( 'NONE', #48725, 1000.000000000000000 ) ;
#34805 = LINE ( 'NONE', #17770, #15259 ) ;
#34806 = ORIENTED_EDGE ( 'NONE', *, *, #21477, .F. ) ;
#34807 = VECTOR ( 'NONE', #11669, 1000.000000000000000 ) ;
#34808 = AXIS2_PLACEMENT_3D ( 'NONE', #23335, #35395, #27763 ) ;
#34809 = FACE_OUTER_BOUND ( 'NONE', #8213, .T. ) ;
#34810 = CYLINDRICAL_SURFACE ( 'NONE', #13795, 4.999999999999997335 ) ;
#34811 = DIRECTION ( 'NONE',  ( 0.000000000000000000, -1.000000000000000000, 0.000000000000000000 ) ) ;
#34812 = FACE_BOUND ( 'NONE', #44129, .T. ) ;
#34813 = VECTOR ( 'NONE', #31210, 1000.000000000000000 ) ;
#34814 = LINE ( 'NONE', #25915, #39542 ) ;
#34815 = VERTEX_POINT ( 'NONE', #25046 ) ;
#34816 = PRESENTATION_LAYER_ASSIGNMENT (  '', '', ( #2078 ) ) ;
#34817 = CARTESIAN_POINT ( 'NONE',  ( -339.1964088526558498, -67.22367097967892846, 20.80804632820117916 ) ) ;
#34819 = VERTEX_POINT ( 'NONE', #41053 ) ;
#34818 = DIRECTION ( 'NONE',  ( -0.000000000000000000, 1.000000000000000000, -0.000000000000000000 ) ) ;
#34820 = VECTOR ( 'NONE', #47457, 1000.000000000000000 ) ;
#34821 = EDGE_CURVE ( 'NONE', #2545, #22186, #17930, .T. ) ;
#34822 = ORIENTED_EDGE ( 'NONE', *, *, #38400, .T. ) ;
#34823 = AXIS2_PLACEMENT_3D ( 'NONE', #12365, #16852, #12884 ) ;
#34824 = ORIENTED_EDGE ( 'NONE', *, *, #41683, .T. ) ;
#34825 = EDGE_CURVE ( 'NONE', #194, #35836, #3167, .T. ) ;
#34826 = CIRCLE ( 'NONE', #47454, 125.0000000000000000 ) ;
#34827 = CARTESIAN_POINT ( 'NONE',  ( -164.2529447963538871, -183.6283474603465606, 44.41421852208711840 ) ) ;
#34828 = EDGE_LOOP ( 'NONE', ( #48146, #6357, #28379, #26648 ) ) ;
#34829 = DIRECTION ( 'NONE',  ( 0.000000000000000000, -0.9709418174260502354, 0.2393156642875652051 ) ) ;
#34830 = CARTESIAN_POINT ( 'NONE',  ( -59.81005805956448995, -177.1207230881787780, -123.4817304940906126 ) ) ;
#34831 = ORIENTED_EDGE ( 'NONE', *, *, #8351, .T. ) ;
#34832 = CARTESIAN_POINT ( 'NONE',  ( 27.50603775690333563, -193.5000000000000000, -99.25348746834811209 ) ) ;
#34833 = ADVANCED_FACE ( 'NONE', ( #13469 ), #1106, .T. ) ;
#34834 = DIRECTION ( 'NONE',  ( 1.000000000000000000, 0.000000000000000000, 0.000000000000000000 ) ) ;
#34835 = CARTESIAN_POINT ( 'NONE',  ( -305.0000000000000568, -75.06648993880729392, -35.41461708323759439 ) ) ;
#34836 = ORIENTED_EDGE ( 'NONE', *, *, #25980, .T. ) ;
#34837 = ORIENTED_EDGE ( 'NONE', *, *, #46564, .T. ) ;
#34838 = EDGE_CURVE ( 'NONE', #993, #51627, #5783, .T. ) ;
#34839 = ADVANCED_FACE ( 'NONE', ( #33937 ), #17154, .T. ) ;
#34840 = ORIENTED_EDGE ( 'NONE', *, *, #33000, .T. ) ;
#34841 = LINE ( 'NONE', #10419, #12467 ) ;
#34842 = CARTESIAN_POINT ( 'NONE',  ( -122.3978016498073345, -193.5000000000000000, -100.8019320314827070 ) ) ;
#34843 = EDGE_CURVE ( 'NONE', #19400, #21155, #49216, .T. ) ;
#34844 = VECTOR ( 'NONE', #38892, 1000.000000000000000 ) ;
#34845 = DIRECTION ( 'NONE',  ( -0.000000000000000000, 1.000000000000000000, -0.000000000000000000 ) ) ;
#34846 = VECTOR ( 'NONE', #13234, 1000.000000000000000 ) ;
#34847 = DIRECTION ( 'NONE',  ( 1.000000000000000000, 6.525800561034990492E-17, 5.781354811211851654E-17 ) ) ;
#34848 = LINE ( 'NONE', #47225, #26397 ) ;
#34849 = ORIENTED_EDGE ( 'NONE', *, *, #4819, .F. ) ;
#34850 = VECTOR ( 'NONE', #15844, 1000.000000000000000 ) ;
#34851 = AXIS2_PLACEMENT_3D ( 'NONE', #48023, #43813, #23843 ) ;
#34852 = CARTESIAN_POINT ( 'NONE',  ( -12.76653800058363863, -175.3837268820161057, -119.7898618611245070 ) ) ;
#34853 = ORIENTED_EDGE ( 'NONE', *, *, #17232, .F. ) ;
#34855 = ORIENTED_EDGE ( 'NONE', *, *, #23490, .F. ) ;
#34854 = DIRECTION ( 'NONE',  ( 0.000000000000000000, 1.000000000000000000, -0.000000000000000000 ) ) ;
#34856 = ORIENTED_EDGE ( 'NONE', *, *, #19254, .F. ) ;
#34857 = CARTESIAN_POINT ( 'NONE',  ( -48.47912675150885065, -177.1207230881787780, 6.938893903907228378E-15 ) ) ;
#34858 = VECTOR ( 'NONE', #34357, 1000.000000000000000 ) ;
#34859 = DIRECTION ( 'NONE',  ( 0.000000000000000000, 0.000000000000000000, 1.000000000000000000 ) ) ;
#34860 = VECTOR ( 'NONE', #9623, 1000.000000000000000 ) ;
#34861 = DIRECTION ( 'NONE',  ( 0.000000000000000000, 0.000000000000000000, 1.000000000000000000 ) ) ;
#34862 = LINE ( 'NONE', #50923, #44377 ) ;
#34863 = VERTEX_POINT ( 'NONE', #1374 ) ;
#34864 = DIRECTION ( 'NONE',  ( -0.9564009842765264224, 0.000000000000000000, 0.2920567706369628924 ) ) ;
#34865 = VECTOR ( 'NONE', #37003, 1000.000000000000114 ) ;
#34866 = ORIENTED_EDGE ( 'NONE', *, *, #17495, .T. ) ;
#34867 = VECTOR ( 'NONE', #50587, 999.9999999999998863 ) ;
#34868 = ORIENTED_EDGE ( 'NONE', *, *, #32735, .F. ) ;
#34869 = CARTESIAN_POINT ( 'NONE',  ( 65.79610465833508215, -177.1207230881787780, -50.65739320401928580 ) ) ;
#34870 = DIRECTION ( 'NONE',  ( -0.000000000000000000, 1.000000000000000000, -0.000000000000000000 ) ) ;
#34871 = DIRECTION ( 'NONE',  ( 0.000000000000000000, -0.000000000000000000, -1.000000000000000000 ) ) ;
#34872 = VERTEX_POINT ( 'NONE', #17431 ) ;
#34873 = CARTESIAN_POINT ( 'NONE',  ( -339.1964088526558498, -150.4759391377552618, 52.47426709956155122 ) ) ;
#34874 = CARTESIAN_POINT ( 'NONE',  ( 15.23368049493606335, -189.7472609257535510, -107.5438431188757136 ) ) ;
#34875 = FACE_OUTER_BOUND ( 'NONE', #46094, .T. ) ;
#34876 = FACE_OUTER_BOUND ( 'NONE', #39468, .T. ) ;
#34877 = ORIENTED_EDGE ( 'NONE', *, *, #38966, .T. ) ;
#34878 = DIRECTION ( 'NONE',  ( 0.000000000000000000, -1.000000000000000000, 0.000000000000000000 ) ) ;
#34879 = CARTESIAN_POINT ( 'NONE',  ( -48.47912675150885065, -187.5000000000000284, -14.99999999999999289 ) ) ;
#34880 = CARTESIAN_POINT ( 'NONE',  ( -339.1964088526558498, -178.4886558749184076, -21.38919645685194837 ) ) ;
#34881 = ORIENTED_EDGE ( 'NONE', *, *, #37816, .F. ) ;
#34882 = VECTOR ( 'NONE', #22100, 1000.000000000000114 ) ;
#34883 = DIRECTION ( 'NONE',  ( -0.000000000000000000, -0.9927088740980548609, -0.1205366802553164696 ) ) ;
#34884 = VECTOR ( 'NONE', #25776, 1000.000000000000000 ) ;
#34885 = VECTOR ( 'NONE', #6897, 1000.000000000000000 ) ;
#34886 = DIRECTION ( 'NONE',  ( -0.000000000000000000, 1.000000000000000000, -0.000000000000000000 ) ) ;
#34887 = EDGE_CURVE ( 'NONE', #7641, #31987, #9784, .T. ) ;
#34888 = ORIENTED_EDGE ( 'NONE', *, *, #47907, .T. ) ;
#34889 = EDGE_CURVE ( 'NONE', #21667, #20982, #31749, .T. ) ;
#34890 = CARTESIAN_POINT ( 'NONE',  ( 69.88207517204676833, -189.7472609257535510, 40.19484891390058579 ) ) ;
#34891 = ORIENTED_EDGE ( 'NONE', *, *, #7951, .T. ) ;
#34892 = DIRECTION ( 'NONE',  ( -0.4827922027307427477, 0.000000000000000000, -0.8757349421956379665 ) ) ;
#34893 = FACE_BOUND ( 'NONE', #50472, .T. ) ;
#34894 = AXIS2_PLACEMENT_3D ( 'NONE', #36036, #31569, #15295 ) ;
#34895 = CARTESIAN_POINT ( 'NONE',  ( 70.49476099643868565, -193.5000000000000000, 34.94873081740416154 ) ) ;
#34896 = EDGE_CURVE ( 'NONE', #32022, #44223, #40784, .T. ) ;
#34897 = CIRCLE ( 'NONE', #29047, 125.0000000000000000 ) ;
#34898 = ADVANCED_FACE ( 'NONE', ( #12929 ), #13721, .T. ) ;
#34899 = AXIS2_PLACEMENT_3D ( 'NONE', #21991, #30913, #14903 ) ;
#34900 = DIRECTION ( 'NONE',  ( 0.000000000000000000, -0.000000000000000000, 1.000000000000000000 ) ) ;
#34901 = ORIENTED_EDGE ( 'NONE', *, *, #11935, .F. ) ;
#34902 = EDGE_CURVE ( 'NONE', #15667, #26081, #25812, .T. ) ;
#34903 = ORIENTED_EDGE ( 'NONE', *, *, #38703, .F. ) ;
#34904 = AXIS2_PLACEMENT_3D ( 'NONE', #50335, #8882, #49097 ) ;
#34905 = FACE_OUTER_BOUND ( 'NONE', #9223, .T. ) ;
#34906 = EDGE_CURVE ( 'NONE', #30515, #14242, #14768, .T. ) ;
#34907 = ORIENTED_EDGE ( 'NONE', *, *, #20807, .F. ) ;
#34908 = CARTESIAN_POINT ( 'NONE',  ( 73.87536152799695799, -189.7472609257535510, -25.58083653558412252 ) ) ;
#34909 = ADVANCED_FACE ( 'NONE', ( #30782 ), #14249, .F. ) ;
#34910 = LINE ( 'NONE', #3125, #49440 ) ;
#34911 = CARTESIAN_POINT ( 'NONE',  ( -118.1688136093591908, -175.3837268820161057, -103.7706487676296661 ) ) ;
#34912 = ORIENTED_EDGE ( 'NONE', *, *, #48234, .F. ) ;
#34915 = EDGE_LOOP ( 'NONE', ( #38074, #29072, #46444, #10693 ) ) ;
#34914 = CARTESIAN_POINT ( 'NONE',  ( 30.50828161901820224, -193.5000000000000000, 96.88131563365348597 ) ) ;
#34913 = DIRECTION ( 'NONE',  ( -0.9785564922995017012, 0.000000000000000000, -0.2059786187411094538 ) ) ;
#34916 = AXIS2_PLACEMENT_3D ( 'NONE', #40624, #28804, #12775 ) ;
#34917 = VECTOR ( 'NONE', #43799, 1000.000000000000000 ) ;
#34918 = DIRECTION ( 'NONE',  ( -0.000000000000000000, 1.000000000000000000, -0.000000000000000000 ) ) ;
#34919 = AXIS2_PLACEMENT_3D ( 'NONE', #16924, #5886, #33976 ) ;
#34920 = VERTEX_POINT ( 'NONE', #6110 ) ;
#34921 = CARTESIAN_POINT ( 'NONE',  ( -490.0000000000001137, -78.50000000000002842, 0.000000000000000000 ) ) ;
#34922 = ORIENTED_EDGE ( 'NONE', *, *, #10032, .F. ) ;
#34923 = CIRCLE ( 'NONE', #3046, 15.00000000000000000 ) ;
#34924 = PLANE ( 'NONE',  #36798 ) ;
#34925 = VERTEX_POINT ( 'NONE', #6360 ) ;
#34928 = ORIENTED_EDGE ( 'NONE', *, *, #27835, .T. ) ;
#34927 = DIRECTION ( 'NONE',  ( 0.8610436117673585521, 0.000000000000000000, -0.5085311186492154079 ) ) ;
#34926 = CARTESIAN_POINT ( 'NONE',  ( -165.5546359831674295, -177.1207230881787780, 43.79868877201493405 ) ) ;
#34929 = VERTEX_POINT ( 'NONE', #10812 ) ;
#34930 = CARTESIAN_POINT ( 'NONE',  ( 46.00000000000000711, 35.00000000000000000, -46.00000000000000000 ) ) ;
#34931 = ORIENTED_EDGE ( 'NONE', *, *, #52009, .T. ) ;
#34932 = CARTESIAN_POINT ( 'NONE',  ( -49.44376233341721161, -177.1207230881787780, 0.2635871660690650709 ) ) ;
#34933 = CIRCLE ( 'NONE', #48512, 125.0000000000000000 ) ;
#34934 = ORIENTED_EDGE ( 'NONE', *, *, #20231, .T. ) ;
#34935 = DIRECTION ( 'NONE',  ( 0.1768902751225592818, 0.000000000000000000, 0.9842305779475992722 ) ) ;
#34936 = FACE_OUTER_BOUND ( 'NONE', #37019, .T. ) ;
#34937 = DIRECTION ( 'NONE',  ( -0.1182731709213730997, 0.000000000000000000, 0.9929810960135161402 ) ) ;
#34938 = VECTOR ( 'NONE', #44783, 1000.000000000000000 ) ;
#34939 = LINE ( 'NONE', #38108, #4746 ) ;
#34940 = VERTEX_POINT ( 'NONE', #18188 ) ;
#34941 =( NAMED_UNIT ( * ) SI_UNIT ( $, .STERADIAN. ) SOLID_ANGLE_UNIT ( ) );
#34942 = CIRCLE ( 'NONE', #6427, 10.00000000000000178 ) ;
#34943 = LINE ( 'NONE', #26286, #17069 ) ;
#34944 = LINE ( 'NONE', #18164, #28160 ) ;
#34945 = AXIS2_PLACEMENT_3D ( 'NONE', #42108, #45303, #5613 ) ;
#34946 = EDGE_CURVE ( 'NONE', #20567, #45186, #43122, .T. ) ;
#34947 = DIRECTION ( 'NONE',  ( -0.000000000000000000, 0.000000000000000000, -1.000000000000000000 ) ) ;
#34948 = EDGE_LOOP ( 'NONE', ( #2396, #30468, #25909, #46996 ) ) ;
#34949 = LINE ( 'NONE', #27324, #19770 ) ;
#34951 = CIRCLE ( 'NONE', #19024, 125.0000000000000000 ) ;
#34950 = FACE_OUTER_BOUND ( 'NONE', #28235, .T. ) ;
#34952 = DIRECTION ( 'NONE',  ( -0.000000000000000000, -1.000000000000000000, -0.000000000000000000 ) ) ;
#34953 = ADVANCED_FACE ( 'NONE', ( #38916 ), #34217, .T. ) ;
#34954 = CARTESIAN_POINT ( 'NONE',  ( -332.3517673607765914, -174.9833430614318388, 28.86398714850502856 ) ) ;
#34955 = EDGE_CURVE ( 'NONE', #39674, #8221, #22900, .T. ) ;
#34956 = DIRECTION ( 'NONE',  ( -0.000000000000000000, 1.000000000000000000, -0.000000000000000000 ) ) ;
#34957 = EDGE_CURVE ( 'NONE', #32738, #10210, #2140, .T. ) ;
#34958 = EDGE_CURVE ( 'NONE', #44807, #39299, #51916, .T. ) ;
#34959 = ORIENTED_EDGE ( 'NONE', *, *, #45496, .F. ) ;
#34960 = EDGE_CURVE ( 'NONE', #2310, #37251, #35233, .T. ) ;
#34961 = AXIS2_PLACEMENT_3D ( 'NONE', #48911, #25246, #12887 ) ;
#34962 = DIRECTION ( 'NONE',  ( 0.000000000000000000, 0.000000000000000000, -1.000000000000000000 ) ) ;
#34963 = VECTOR ( 'NONE', #33491, 1000.000000000000114 ) ;
#34964 = CARTESIAN_POINT ( 'NONE',  ( -339.1964088526558498, -84.00150778970767362, -43.83057281297470098 ) ) ;
#34965 = EDGE_CURVE ( 'NONE', #27624, #30532, #46566, .T. ) ;
#34966 = LINE ( 'NONE', #38396, #2648 ) ;
#34967 = DIRECTION ( 'NONE',  ( 0.3758275821142422202, 0.000000000000000000, -0.9266896074318318188 ) ) ;
#34968 = FACE_OUTER_BOUND ( 'NONE', #3835, .T. ) ;
#34969 = CIRCLE ( 'NONE', #4787, 60.00000000000000000 ) ;
#34970 = VERTEX_POINT ( 'NONE', #39183 ) ;
#34971 = EDGE_CURVE ( 'NONE', #6765, #27048, #50767, .T. ) ;
#34972 = CARTESIAN_POINT ( 'NONE',  ( -167.1668396246903114, -193.5000000000000000, -35.90758392117659525 ) ) ;
#34973 = ADVANCED_FACE ( 'NONE', ( #22129 ), #30268, .F. ) ;
#34974 = DIRECTION ( 'NONE',  ( 0.000000000000000000, 0.000000000000000000, 1.000000000000000000 ) ) ;
#34975 = ORIENTED_EDGE ( 'NONE', *, *, #8083, .T. ) ;
#34976 = VECTOR ( 'NONE', #42372, 999.9999999999998863 ) ;
#34977 = EDGE_LOOP ( 'NONE', ( #48554, #9094, #14004, #40002 ) ) ;
#34978 = EDGE_CURVE ( 'NONE', #7704, #44807, #46313, .T. ) ;
#34979 = VECTOR ( 'NONE', #12320, 1000.000000000000114 ) ;
#34980 = ORIENTED_EDGE ( 'NONE', *, *, #428, .T. ) ;
#34981 = LINE ( 'NONE', #34464, #25047 ) ;
#34982 = AXIS2_PLACEMENT_3D ( 'NONE', #46584, #19240, #18976 ) ;
#34983 = AXIS2_PLACEMENT_3D ( 'NONE', #51320, #31854, #15572 ) ;
#34984 = EDGE_CURVE ( 'NONE', #1807, #50561, #42346, .T. ) ;
#34986 = AXIS2_PLACEMENT_3D ( 'NONE', #41125, #16965, #4606 ) ;
#34985 = LINE ( 'NONE', #3194, #16929 ) ;
#34987 = ORIENTED_EDGE ( 'NONE', *, *, #19525, .F. ) ;
#34988 = ADVANCED_FACE ( 'NONE', ( #22382 ), #38409, .F. ) ;
#34989 = VECTOR ( 'NONE', #9228, 1000.000000000000000 ) ;
#34990 = CARTESIAN_POINT ( 'NONE',  ( -60.80616967713025645, -183.6283474603465606, -123.3865623328508150 ) ) ;
#34991 = FACE_OUTER_BOUND ( 'NONE', #213, .T. ) ;
#34994 = ORIENTED_EDGE ( 'NONE', *, *, #51362, .F. ) ;
#34993 = FACE_OUTER_BOUND ( 'NONE', #19359, .T. ) ;
#34992 = PLANE ( 'NONE',  #51856 ) ;
#34995 = CARTESIAN_POINT ( 'NONE',  ( -67.22356632362125595, -177.1207230881787780, -123.5865930638409793 ) ) ;
#34996 = ORIENTED_EDGE ( 'NONE', *, *, #44320, .T. ) ;
#34997 = CARTESIAN_POINT ( 'NONE',  ( -4.525132525065792777, -193.5000000000000000, 115.9484881370938325 ) ) ;
#34998 = EDGE_LOOP ( 'NONE', ( #38440, #16703, #34759, #9881 ) ) ;
#34999 = LINE ( 'NONE', #2937, #40866 ) ;
#35000 = CARTESIAN_POINT ( 'NONE',  ( -48.47912675150885065, -183.6283474603465606, -0.9999999999999931166 ) ) ;
#35001 = FACE_OUTER_BOUND ( 'NONE', #5324, .T. ) ;
#35002 = EDGE_CURVE ( 'NONE', #45545, #4141, #34981, .T. ) ;
#35003 = VERTEX_POINT ( 'NONE', #38660 ) ;
#35004 = EDGE_CURVE ( 'NONE', #27368, #18178, #42092, .T. ) ;
#35005 = VECTOR ( 'NONE', #24995, 1000.000000000000000 ) ;
#35006 = ORIENTED_EDGE ( 'NONE', *, *, #3471, .F. ) ;
#35007 = DIRECTION ( 'NONE',  ( 0.000000000000000000, -1.000000000000000000, -0.000000000000000000 ) ) ;
#35008 = AXIS2_PLACEMENT_3D ( 'NONE', #15016, #11292, #50495 ) ;
#35009 = LINE ( 'NONE', #30036, #687 ) ;
#35010 = ORIENTED_EDGE ( 'NONE', *, *, #19774, .F. ) ;
#35011 = LINE ( 'NONE', #51068, #35798 ) ;
#35012 = CIRCLE ( 'NONE', #14017, 125.0000000000000000 ) ;
#35013 = DIRECTION ( 'NONE',  ( 0.000000000000000000, 0.000000000000000000, -1.000000000000000000 ) ) ;
#35014 = ORIENTED_EDGE ( 'NONE', *, *, #34889, .F. ) ;
#35015 = FACE_BOUND ( 'NONE', #31351, .T. ) ;
#35016 = DIRECTION ( 'NONE',  ( 1.043714542225393539E-14, -0.6631226582407911962, 0.7485107481711046340 ) ) ;
#35017 = VERTEX_POINT ( 'NONE', #47081 ) ;
#35018 = LINE ( 'NONE', #23458, #36679 ) ;
#35019 = ORIENTED_EDGE ( 'NONE', *, *, #37052, .T. ) ;
#35020 = AXIS2_PLACEMENT_3D ( 'NONE', #42690, #14066, #42935 ) ;
#35021 = PLANE ( 'NONE',  #3798 ) ;
#35022 = CIRCLE ( 'NONE', #8161, 125.0000000000000000 ) ;
#35023 = DIRECTION ( 'NONE',  ( 0.000000000000000000, 1.000000000000000000, -0.000000000000000000 ) ) ;
#35024 = VERTEX_POINT ( 'NONE', #11059 ) ;
#35025 = AXIS2_PLACEMENT_3D ( 'NONE', #7541, #23562, #23820 ) ;
#35026 = ADVANCED_FACE ( 'NONE', ( #32068 ), #51536, .F. ) ;
#35027 = DIRECTION ( 'NONE',  ( 0.000000000000000000, 0.000000000000000000, 1.000000000000000000 ) ) ;
#35028 = CARTESIAN_POINT ( 'NONE',  ( -490.0000000000001137, -168.5000000000000284, 0.000000000000000000 ) ) ;
#35029 = LINE ( 'NONE', #50810, #47592 ) ;
#35030 = EDGE_CURVE ( 'NONE', #13288, #29108, #3690, .T. ) ;
#35031 = AXIS2_PLACEMENT_3D ( 'NONE', #44713, #32623, #48667 ) ;
#35032 = EDGE_CURVE ( 'NONE', #21876, #20693, #15535, .T. ) ;
#35033 = EDGE_LOOP ( 'NONE', ( #49007, #10892, #34866, #37603 ) ) ;
#35035 = CIRCLE ( 'NONE', #12358, 125.0000000000000000 ) ;
#35034 = LINE ( 'NONE', #39985, #14531 ) ;
#35036 = EDGE_CURVE ( 'NONE', #36520, #3787, #32317, .T. ) ;
#35037 = DIRECTION ( 'NONE',  ( 0.000000000000000000, 0.000000000000000000, -1.000000000000000000 ) ) ;
#35038 = LINE ( 'NONE', #15085, #10473 ) ;
#35040 = ORIENTED_EDGE ( 'NONE', *, *, #18610, .F. ) ;
#35039 = DIRECTION ( 'NONE',  ( 0.000000000000000000, -0.9709418174260502354, 0.2393156642875652051 ) ) ;
#35041 = EDGE_LOOP ( 'NONE', ( #27867, #49348, #19457, #37927 ) ) ;
#35042 = LINE ( 'NONE', #51102, #16531 ) ;
#35043 = CARTESIAN_POINT ( 'NONE',  ( -124.9871112439422092, -193.5000000000000000, -98.85104101073275729 ) ) ;
#35044 = ORIENTED_EDGE ( 'NONE', *, *, #5314, .F. ) ;
#35045 = AXIS2_PLACEMENT_3D ( 'NONE', #45366, #21704, #50083 ) ;
#35046 = CIRCLE ( 'NONE', #48497, 60.00000000000000000 ) ;
#35047 = ORIENTED_EDGE ( 'NONE', *, *, #19285, .F. ) ;
#35048 = DIRECTION ( 'NONE',  ( 0.000000000000000000, 1.000000000000000000, 0.000000000000000000 ) ) ;
#35049 = PRODUCT_RELATED_PRODUCT_CATEGORY ( 'part', '', ( #802 ) ) ;
#35050 = VERTEX_POINT ( 'NONE', #44158 ) ;
#35051 = DIRECTION ( 'NONE',  ( -0.000000000000000000, 0.1205366802553199113, -0.9927088740980544168 ) ) ;
#35052 = DIRECTION ( 'NONE',  ( -0.000000000000000000, -1.000000000000000000, 0.000000000000000000 ) ) ;
#35053 = CIRCLE ( 'NONE', #13225, 125.0000000000000000 ) ;
#35054 = CARTESIAN_POINT ( 'NONE',  ( -94.25732089370191602, -193.5000000000000000, 116.3157639405754935 ) ) ;
#35055 = CARTESIAN_POINT ( 'NONE',  ( -339.1964088526558498, -84.00150778970699150, 43.83057281297409702 ) ) ;
#35056 = EDGE_LOOP ( 'NONE', ( #34205, #41105, #15008, #17049 ) ) ;
#35057 = ORIENTED_EDGE ( 'NONE', *, *, #19669, .F. ) ;
#35058 = EDGE_CURVE ( 'NONE', #30216, #50878, #15821, .T. ) ;
#35059 = ORIENTED_EDGE ( 'NONE', *, *, #12911, .T. ) ;
#35060 = DIRECTION ( 'NONE',  ( -0.5085311186492273983, 0.000000000000000000, 0.8610436117673514467 ) ) ;
#35061 = CARTESIAN_POINT ( 'NONE',  ( -168.0489871616337325, -193.5000000000000000, -32.84887689123904408 ) ) ;
#35062 = CIRCLE ( 'NONE', #28330, 20.00000000000001776 ) ;
#35063 = LINE ( 'NONE', #47407, #30780 ) ;
#35064 = VECTOR ( 'NONE', #41867, 1000.000000000000000 ) ;
#35065 = DIRECTION ( 'NONE',  ( 0.000000000000000000, 0.000000000000000000, 1.000000000000000000 ) ) ;
#35066 = CARTESIAN_POINT ( 'NONE',  ( 46.00000000000000000, 0.000000000000000000, 0.000000000000000000 ) ) ;
#35067 = ORIENTED_EDGE ( 'NONE', *, *, #16665, .T. ) ;
#35068 = DIRECTION ( 'NONE',  ( 0.000000000000000000, 1.000000000000000000, 0.000000000000000000 ) ) ;
#35069 = CARTESIAN_POINT ( 'NONE',  ( -142.9772358822569629, -183.6283474603465606, 81.82363577055970438 ) ) ;
#35070 = AXIS2_PLACEMENT_3D ( 'NONE', #5549, #41520, #10766 ) ;
#35071 = ORIENTED_EDGE ( 'NONE', *, *, #23669, .F. ) ;
#35072 = ORIENTED_EDGE ( 'NONE', *, *, #47444, .F. ) ;
#35073 = DIRECTION ( 'NONE',  ( -0.9374196611341254481, 0.000000000000000000, 0.3482016354343867026 ) ) ;
#35074 = DIRECTION ( 'NONE',  ( 0.000000000000000000, 0.000000000000000000, -1.000000000000000000 ) ) ;
#35075 = FACE_OUTER_BOUND ( 'NONE', #32602, .T. ) ;
#35076 = LINE ( 'NONE', #51899, #16172 ) ;
#35077 = DIRECTION ( 'NONE',  ( 0.000000000000000000, -1.000000000000000000, -0.000000000000000000 ) ) ;
#35078 = ORIENTED_EDGE ( 'NONE', *, *, #23200, .F. ) ;
#35079 = DIRECTION ( 'NONE',  ( 0.000000000000000000, -0.000000000000000000, 1.000000000000000000 ) ) ;
#35080 = ORIENTED_EDGE ( 'NONE', *, *, #7610, .F. ) ;
#35081 = DIRECTION ( 'NONE',  ( 0.000000000000000000, 0.000000000000000000, 1.000000000000000000 ) ) ;
#35082 = AXIS2_PLACEMENT_3D ( 'NONE', #22670, #34737, #50790 ) ;
#35083 = CIRCLE ( 'NONE', #4899, 125.0000000000000000 ) ;
#35084 = DIRECTION ( 'NONE',  ( -0.000000000000000000, 1.000000000000000000, 0.000000000000000000 ) ) ;
#35085 = ORIENTED_EDGE ( 'NONE', *, *, #42692, .T. ) ;
#35086 = AXIS2_PLACEMENT_3D ( 'NONE', #14058, #25355, #914 ) ;
#35087 = CARTESIAN_POINT ( 'NONE',  ( -339.1964088526558498, -84.75001853787875916, -44.49369547121548862 ) ) ;
#35088 = DIRECTION ( 'NONE',  ( 0.000000000000000000, -1.000000000000000000, 0.000000000000000000 ) ) ;
#35089 = DIRECTION ( 'NONE',  ( 0.000000000000000000, -0.000000000000000000, -1.000000000000000000 ) ) ;
#35090 = EDGE_CURVE ( 'NONE', #36830, #29101, #8163, .T. ) ;
#35091 = PLANE ( 'NONE',  #11479 ) ;
#35092 = DIRECTION ( 'NONE',  ( 0.000000000000000000, -1.000000000000000000, -0.000000000000000000 ) ) ;
#35093 = ORIENTED_EDGE ( 'NONE', *, *, #3831, .T. ) ;
#35094 = DIRECTION ( 'NONE',  ( 1.000000000000000000, -1.050884489711724171E-17, -8.654812430365567976E-17 ) ) ;
#35096 = ORIENTED_EDGE ( 'NONE', *, *, #31877, .T. ) ;
#35095 = DIRECTION ( 'NONE',  ( -0.6068001458186002006, 0.000000000000000000, 0.7948544414133481562 ) ) ;
#35097 = VERTEX_POINT ( 'NONE', #16306 ) ;
#35098 = CARTESIAN_POINT ( 'NONE',  ( -85.77912150413021664, -189.7472609257535510, -119.3051146910911768 ) ) ;
#35099 = ORIENTED_EDGE ( 'NONE', *, *, #43846, .T. ) ;
#35100 = AXIS2_PLACEMENT_3D ( 'NONE', #16534, #20198, #28338 ) ;
#35101 = CARTESIAN_POINT ( 'NONE',  ( 43.86477233319988756, -193.5000000000000000, -84.24728067915975771 ) ) ;
#35102 = ORIENTED_EDGE ( 'NONE', *, *, #268, .T. ) ;
#35103 = DIRECTION ( 'NONE',  ( 0.000000000000000000, -0.2393156642875652051, -0.9709418174260502354 ) ) ;
#35104 = DIRECTION ( 'NONE',  ( -0.000000000000000000, 1.000000000000000000, -0.000000000000000000 ) ) ;
#35105 = ADVANCED_FACE ( 'NONE', ( #39430 ), #44432, .T. ) ;
#35106 = ORIENTED_EDGE ( 'NONE', *, *, #48491, .T. ) ;
#35107 = FACE_OUTER_BOUND ( 'NONE', #46352, .T. ) ;
#35108 = DIRECTION ( 'NONE',  ( 0.000000000000000000, 1.000000000000000000, 0.000000000000000000 ) ) ;
#35109 = CARTESIAN_POINT ( 'NONE',  ( 48.69345348225014902, -193.5000000000000000, -78.62880929222872339 ) ) ;
#35110 = ORIENTED_EDGE ( 'NONE', *, *, #9405, .F. ) ;
#35111 = VERTEX_POINT ( 'NONE', #3433 ) ;
#35112 = ORIENTED_EDGE ( 'NONE', *, *, #51093, .F. ) ;
#35113 = PLANE ( 'NONE',  #44371 ) ;
#35114 = CARTESIAN_POINT ( 'NONE',  ( -336.3521761649654422, -160.6539403396202772, 45.90766452162722544 ) ) ;
#35115 = VECTOR ( 'NONE', #29767, 1000.000000000000000 ) ;
#35116 = VECTOR ( 'NONE', #17808, 1000.000000000000000 ) ;
#35117 = ADVANCED_FACE ( 'NONE', ( #23920 ), #23662, .F. ) ;
#35118 = LINE ( 'NONE', #51176, #42743 ) ;
#35119 = PLANE ( 'NONE',  #21163 ) ;
#35120 = DIRECTION ( 'NONE',  ( 0.000000000000000000, 0.000000000000000000, -1.000000000000000000 ) ) ;
#35121 = VERTEX_POINT ( 'NONE', #266 ) ;
#35122 = VECTOR ( 'NONE', #22648, 1000.000000000000000 ) ;
#35123 = EDGE_CURVE ( 'NONE', #24837, #43547, #27347, .T. ) ;
#35124 = DIRECTION ( 'NONE',  ( -0.000000000000000000, 1.000000000000000000, -0.000000000000000000 ) ) ;
#35125 = ORIENTED_EDGE ( 'NONE', *, *, #13149, .T. ) ;
#35127 = ORIENTED_EDGE ( 'NONE', *, *, #38154, .T. ) ;
#35126 = DIRECTION ( 'NONE',  ( 0.000000000000000000, 1.000000000000000000, 0.000000000000000000 ) ) ;
#35128 = VECTOR ( 'NONE', #20433, 1000.000000000000000 ) ;
#35129 = ORIENTED_EDGE ( 'NONE', *, *, #14388, .T. ) ;
#35130 = CARTESIAN_POINT ( 'NONE',  ( -48.47912675150885065, -189.7472609257535510, 6.938893903907228378E-15 ) ) ;
#35131 = FACE_OUTER_BOUND ( 'NONE', #7578, .T. ) ;
#35132 = CARTESIAN_POINT ( 'NONE',  ( -70.42295845586433245, -193.5000000000000000, -123.0587999703024877 ) ) ;
#35133 = DIRECTION ( 'NONE',  ( -0.000000000000000000, 1.000000000000000000, -0.000000000000000000 ) ) ;
#35134 = ORIENTED_EDGE ( 'NONE', *, *, #32859, .T. ) ;
#35135 = CARTESIAN_POINT ( 'NONE',  ( -30.31202594373734627, -177.1207230881787780, -123.6727797384705809 ) ) ;
#35136 = ORIENTED_EDGE ( 'NONE', *, *, #38531, .F. ) ;
#35137 = CIRCLE ( 'NONE', #41861, 14.00000000000001066 ) ;
#35138 = EDGE_CURVE ( 'NONE', #10684, #34133, #51806, .T. ) ;
#35139 = ORIENTED_EDGE ( 'NONE', *, *, #25886, .T. ) ;
#35140 = PLANE ( 'NONE',  #191 ) ;
#35141 = DIRECTION ( 'NONE',  ( -0.000000000000000000, 1.000000000000000000, -0.000000000000000000 ) ) ;
#35142 = ORIENTED_EDGE ( 'NONE', *, *, #33964, .T. ) ;
#35143 = DIRECTION ( 'NONE',  ( 0.000000000000000000, 0.000000000000000000, -1.000000000000000000 ) ) ;
#35144 = CARTESIAN_POINT ( 'NONE',  ( -101.0675409952199999, -183.6283474603465606, 113.3995532942341100 ) ) ;
#35145 = DIRECTION ( 'NONE',  ( -0.000000000000000000, 1.000000000000000000, -0.000000000000000000 ) ) ;
#35146 = CARTESIAN_POINT ( 'NONE',  ( -168.9345475356665531, -183.6283474603465606, 29.43839964798724296 ) ) ;
#35147 = ADVANCED_FACE ( 'NONE', ( #47604 ), #4222, .T. ) ;
#35148 = ORIENTED_EDGE ( 'NONE', *, *, #29455, .F. ) ;
#35149 = LINE ( 'NONE', #51984, #23798 ) ;
#35150 = DIRECTION ( 'NONE',  ( 0.000000000000000000, -0.9350162426854121689, 0.3546048870425426158 ) ) ;
#35151 = EDGE_CURVE ( 'NONE', #15345, #25387, #27615, .T. ) ;
#35152 = LINE ( 'NONE', #18616, #28224 ) ;
#35153 = ORIENTED_EDGE ( 'NONE', *, *, #24704, .T. ) ;
#35154 = AXIS2_PLACEMENT_3D ( 'NONE', #7921, #39708, #51839 ) ;
#35155 = EDGE_CURVE ( 'NONE', #37521, #27989, #43644, .T. ) ;
#35156 = VECTOR ( 'NONE', #5520, 1000.000000000000000 ) ;
#35157 = AXIS2_PLACEMENT_3D ( 'NONE', #31228, #43322, #39371 ) ;
#35158 = PLANE ( 'NONE',  #26950 ) ;
#35159 = EDGE_LOOP ( 'NONE', ( #812, #35665, #51696, #17887 ) ) ;
#35160 = DIRECTION ( 'NONE',  ( 0.000000000000000000, 0.6631226582407885317, -0.7485107481711069655 ) ) ;
#35161 = ORIENTED_EDGE ( 'NONE', *, *, #12722, .T. ) ;
#35162 = VECTOR ( 'NONE', #16153, 1000.000000000000000 ) ;
#35163 = FACE_OUTER_BOUND ( 'NONE', #36478, .T. ) ;
#35164 = FACE_BOUND ( 'NONE', #31531, .T. ) ;
#35166 = ORIENTED_EDGE ( 'NONE', *, *, #1457, .F. ) ;
#35165 = LINE ( 'NONE', #51219, #25432 ) ;
#35167 = ADVANCED_FACE ( 'NONE', ( #27860 ), #4484, .T. ) ;
#35168 = DIRECTION ( 'NONE',  ( 0.000000000000000000, 0.2393156642875582940, 0.9709418174260519008 ) ) ;
#35169 = ORIENTED_EDGE ( 'NONE', *, *, #5440, .F. ) ;
#35170 = CIRCLE ( 'NONE', #3297, 125.0000000000000000 ) ;
#35171 = ORIENTED_EDGE ( 'NONE', *, *, #45388, .T. ) ;
#35172 = DIRECTION ( 'NONE',  ( 1.000000000000000000, 0.000000000000000000, 0.000000000000000000 ) ) ;
#35173 = ORIENTED_EDGE ( 'NONE', *, *, #25595, .T. ) ;
#35174 = CARTESIAN_POINT ( 'NONE',  ( -330.4913330509368166, -64.99044476834235695, 7.608018572112246858 ) ) ;
#35175 = EDGE_CURVE ( 'NONE', #38308, #10671, #3249, .T. ) ;
#35176 = CARTESIAN_POINT ( 'NONE',  ( -123.6678354051270077, -189.7472609257535510, 99.85818990449067201 ) ) ;
#35177 = DIRECTION ( 'NONE',  ( 0.5586467658036476935, 0.000000000000000000, 0.8294056854502049880 ) ) ;
#35178 = ORIENTED_EDGE ( 'NONE', *, *, #23167, .T. ) ;
#35181 = EDGE_LOOP ( 'NONE', ( #23440, #34608, #49104, #9726 ) ) ;
#35180 = CARTESIAN_POINT ( 'NONE',  ( -48.47912675150885065, -189.7472609257535510, 6.938893903907228378E-15 ) ) ;
#35179 = DIRECTION ( 'NONE',  ( 0.2920567706369694982, 0.000000000000000000, 0.9564009842765243130 ) ) ;
#35182 = VECTOR ( 'NONE', #16496, 1000.000000000000000 ) ;
#35183 = LINE ( 'NONE', #30985, #15603 ) ;
#35184 = ORIENTED_EDGE ( 'NONE', *, *, #30150, .T. ) ;
#35185 = CARTESIAN_POINT ( 'NONE',  ( -305.0000000000000568, -67.99860710409808462, -22.79463504017392950 ) ) ;
#35186 = AXIS2_PLACEMENT_3D ( 'NONE', #398, #26068, #12228 ) ;
#35187 = VERTEX_POINT ( 'NONE', #31291 ) ;
#35188 = EDGE_CURVE ( 'NONE', #14029, #2008, #15, .T. ) ;
#35189 = EDGE_CURVE ( 'NONE', #49231, #49368, #11311, .T. ) ;
#35190 = DIRECTION ( 'NONE',  ( -1.000000000000000000, 0.000000000000000000, -0.000000000000000000 ) ) ;
#35191 = ORIENTED_EDGE ( 'NONE', *, *, #40145, .T. ) ;
#35193 = LINE ( 'NONE', #15494, #19113 ) ;
#35192 = DIRECTION ( 'NONE',  ( 0.5829794791144762289, 0.000000000000000000, -0.8124868780056783146 ) ) ;
#35194 = EDGE_LOOP ( 'NONE', ( #50724, #39895, #18513, #32831 ) ) ;
#35195 = CARTESIAN_POINT ( 'NONE',  ( -163.6979789053106629, -175.3837268820161057, -45.83253885719557985 ) ) ;
#35196 = ORIENTED_EDGE ( 'NONE', *, *, #19015, .T. ) ;
#35197 = CARTESIAN_POINT ( 'NONE',  ( -49.35486169370449971, -189.7472609257535510, 0.4827922027307437469 ) ) ;
#35198 = CARTESIAN_POINT ( 'NONE',  ( -332.3517673607765914, -120.8677111499054320, 59.00000000000000000 ) ) ;
#35199 = ORIENTED_EDGE ( 'NONE', *, *, #7832, .T. ) ;
#35200 = DIRECTION ( 'NONE',  ( 0.000000000000000000, 0.8229838658936536877, -0.5680647467311596976 ) ) ;
#35201 = LINE ( 'NONE', #3152, #29173 ) ;
#35202 = DIRECTION ( 'NONE',  ( -1.000000000000000000, -0.000000000000000000, 0.000000000000000000 ) ) ;
#35203 = FACE_OUTER_BOUND ( 'NONE', #44485, .T. ) ;
#35204 = ORIENTED_EDGE ( 'NONE', *, *, #5580, .F. ) ;
#35205 = DIRECTION ( 'NONE',  ( 0.6570486972603404308, -3.548008715945507234E-17, 0.7538481341944740510 ) ) ;
#35206 = EDGE_CURVE ( 'NONE', #24408, #49251, #17518, .T. ) ;
#35207 = LINE ( 'NONE', #19436, #48110 ) ;
#35208 = CARTESIAN_POINT ( 'NONE',  ( 54.46899307705341187, -177.1207230881787780, -70.89911581792812001 ) ) ;
#35209 = ADVANCED_FACE ( 'NONE', ( #1583 ), #17625, .F. ) ;
#35210 = VECTOR ( 'NONE', #36673, 1000.000000000000114 ) ;
#35211 = CARTESIAN_POINT ( 'NONE',  ( -48.47912675150885065, -177.1207230881787780, 6.938893903907228378E-15 ) ) ;
#35212 = ORIENTED_EDGE ( 'NONE', *, *, #50939, .T. ) ;
#35213 = ADVANCED_FACE ( 'NONE', ( #12614 ), #37831, .F. ) ;
#35214 = LINE ( 'NONE', #11287, #49171 ) ;
#35215 = LINE ( 'NONE', #36434, #7634 ) ;
#35216 = EDGE_CURVE ( 'NONE', #35836, #3435, #45227, .T. ) ;
#35217 = CARTESIAN_POINT ( 'NONE',  ( -121.5885020763900997, -177.1207230881787780, -101.3904297239420913 ) ) ;
#35219 = ORIENTED_EDGE ( 'NONE', *, *, #15003, .F. ) ;
#35218 = DIRECTION ( 'NONE',  ( 0.6965510290629932655, 0.000000000000000000, 0.7175072570443347120 ) ) ;
#35220 = ORIENTED_EDGE ( 'NONE', *, *, #14413, .F. ) ;
#35221 = ADVANCED_FACE ( 'NONE', ( #9464 ), #45728, .F. ) ;
#35222 = DIRECTION ( 'NONE',  ( -0.000000000000000000, -0.2393156642875482742, 0.9709418174260544543 ) ) ;
#35223 = DIRECTION ( 'NONE',  ( -0.5085311186492273983, 0.000000000000000000, 0.8610436117673514467 ) ) ;
#35224 = VECTOR ( 'NONE', #13269, 1000.000000000000000 ) ;
#35225 = DIRECTION ( 'NONE',  ( 1.000000000000000000, -0.000000000000000000, -0.000000000000000000 ) ) ;
#35226 = DIRECTION ( 'NONE',  ( -1.000000000000000000, -0.000000000000000000, 0.000000000000000000 ) ) ;
#35227 = CARTESIAN_POINT ( 'NONE',  ( 20.66186849114819069, -189.7472609257535510, -104.1370384486465070 ) ) ;
#35228 = ORIENTED_EDGE ( 'NONE', *, *, #21925, .T. ) ;
#35229 = CARTESIAN_POINT ( 'NONE',  ( 1.988269209400828741, 57.70862950595167007, -16.62469262932894409 ) ) ;
#35230 = ORIENTED_EDGE ( 'NONE', *, *, #8282, .T. ) ;
#35231 = ORIENTED_EDGE ( 'NONE', *, *, #9138, .T. ) ;
#35232 = EDGE_LOOP ( 'NONE', ( #21923, #39929, #637, #35598 ) ) ;
#35233 = LINE ( 'NONE', #38137, #30925 ) ;
#35234 = DIRECTION ( 'NONE',  ( -0.000000000000000000, 0.8854560256532157947, 0.4647231720437573488 ) ) ;
#35235 = EDGE_LOOP ( 'NONE', ( #6774, #19518, #29855, #19224 ) ) ;
#35236 = VECTOR ( 'NONE', #26393, 1000.000000000000227 ) ;
#35237 = AXIS2_PLACEMENT_3D ( 'NONE', #7176, #26877, #30312 ) ;
#35238 = DIRECTION ( 'NONE',  ( 0.000000000000000000, 1.000000000000000000, 0.000000000000000000 ) ) ;
#35239 = DIRECTION ( 'NONE',  ( 0.000000000000000000, 1.000000000000000000, 0.000000000000000000 ) ) ;
#35242 = ORIENTED_EDGE ( 'NONE', *, *, #16190, .T. ) ;
#35241 = FACE_OUTER_BOUND ( 'NONE', #11054, .T. ) ;
#35240 = DIRECTION ( 'NONE',  ( 0.000000000000000000, 0.000000000000000000, 1.000000000000000000 ) ) ;
#35243 = DIRECTION ( 'NONE',  ( 0.000000000000000000, -1.000000000000000000, 0.000000000000000000 ) ) ;
#35244 = ORIENTED_EDGE ( 'NONE', *, *, #33678, .T. ) ;
#35245 = DIRECTION ( 'NONE',  ( -0.000000000000000000, 1.000000000000000000, -0.000000000000000000 ) ) ;
#35246 = ORIENTED_EDGE ( 'NONE', *, *, #23345, .T. ) ;
#35247 = EDGE_CURVE ( 'NONE', #47918, #24476, #16582, .T. ) ;
#35248 = EDGE_CURVE ( 'NONE', #21906, #25767, #51099, .T. ) ;
#35249 = EDGE_CURVE ( 'NONE', #37592, #26366, #32610, .T. ) ;
#35250 = LINE ( 'NONE', #15291, #32473 ) ;
#35251 = CARTESIAN_POINT ( 'NONE',  ( -85.14888725715769624, -175.3837268820161057, 119.5003291395398577 ) ) ;
#35253 = DIRECTION ( 'NONE',  ( 0.000000000000000000, 1.000000000000000000, 0.000000000000000000 ) ) ;
#35252 = DIRECTION ( 'NONE',  ( 0.9266896074318291543, 0.000000000000000000, 0.3758275821142488260 ) ) ;
#35254 = VERTEX_POINT ( 'NONE', #21558 ) ;
#35255 = EDGE_CURVE ( 'NONE', #15087, #49860, #25232, .T. ) ;
#35256 = DIRECTION ( 'NONE',  ( 1.000000000000000000, 0.000000000000000000, 0.000000000000000000 ) ) ;
#35257 = ORIENTED_EDGE ( 'NONE', *, *, #44635, .F. ) ;
#35258 = LINE ( 'NONE', #22925, #18103 ) ;
#35260 = CIRCLE ( 'NONE', #6769, 125.0000000000000000 ) ;
#35259 = PLANE ( 'NONE',  #19146 ) ;
#35261 = VERTEX_POINT ( 'NONE', #37312 ) ;
#35262 = EDGE_CURVE ( 'NONE', #17251, #21890, #23355, .T. ) ;
#35263 = DIRECTION ( 'NONE',  ( 0.2920567706369833760, 0.000000000000000000, -0.9564009842765202052 ) ) ;
#35264 = DIRECTION ( 'NONE',  ( -0.000000000000000000, 1.000000000000000000, -0.000000000000000000 ) ) ;
#35265 = ORIENTED_EDGE ( 'NONE', *, *, #681, .F. ) ;
#35266 = FACE_BOUND ( 'NONE', #1475, .T. ) ;
#35267 = EDGE_CURVE ( 'NONE', #22193, #40543, #12876, .T. ) ;
#35268 = DIRECTION ( 'NONE',  ( -0.000000000000000000, 1.000000000000000000, -0.000000000000000000 ) ) ;
#35269 = EDGE_CURVE ( 'NONE', #51645, #26457, #9139, .T. ) ;
#35270 = ORIENTED_EDGE ( 'NONE', *, *, #39866, .T. ) ;
#35271 = LINE ( 'NONE', #47891, #14866 ) ;
#35272 = ORIENTED_EDGE ( 'NONE', *, *, #202, .T. ) ;
#35273 = EDGE_CURVE ( 'NONE', #15315, #21423, #49670, .T. ) ;
#35274 = LINE ( 'NONE', #46871, #17281 ) ;
#35275 = DIRECTION ( 'NONE',  ( 0.05924062789372142729, 0.000000000000000000, -0.9982437317643209074 ) ) ;
#35276 = ORIENTED_EDGE ( 'NONE', *, *, #38428, .F. ) ;
#35277 = ADVANCED_FACE ( 'NONE', ( #17103 ), #4745, .F. ) ;
#35278 = FACE_OUTER_BOUND ( 'NONE', #43018, .T. ) ;
#35279 = DIRECTION ( 'NONE',  ( -0.8455960035018199594, 0.000000000000000000, -0.5338233779648003940 ) ) ;
#35280 = CARTESIAN_POINT ( 'NONE',  ( 36.10886851198521441, -177.1207230881787780, 92.03190238880813467 ) ) ;
#35281 = ADVANCED_FACE ( 'NONE', ( #33109 ), #17367, .F. ) ;
#35282 = CIRCLE ( 'NONE', #9302, 60.00000000000000000 ) ;
#35283 = CIRCLE ( 'NONE', #43690, 125.0000000000000000 ) ;
#35284 = CARTESIAN_POINT ( 'NONE',  ( -336.3521761649654422, -154.8494888031386836, 50.05135858667791382 ) ) ;
#35285 = CARTESIAN_POINT ( 'NONE',  ( -336.3521761649654422, -123.5000000000000284, 0.000000000000000000 ) ) ;
#35286 = DIRECTION ( 'NONE',  ( 0.000000000000000000, 0.000000000000000000, -1.000000000000000000 ) ) ;
#35288 = VERTEX_POINT ( 'NONE', #41505 ) ;
#35287 = CARTESIAN_POINT ( 'NONE',  ( -336.3521761649654422, -123.5000000000000284, 0.000000000000000000 ) ) ;
#35289 = EDGE_LOOP ( 'NONE', ( #22403, #23783, #51041, #43628 ) ) ;
#35290 = FACE_OUTER_BOUND ( 'NONE', #39725, .T. ) ;
#35291 = EDGE_CURVE ( 'NONE', #46556, #26846, #5802, .T. ) ;
#35292 = DIRECTION ( 'NONE',  ( -0.8896570909947530970, 0.000000000000000000, 0.4566292373937018700 ) ) ;
#35293 = EDGE_LOOP ( 'NONE', ( #38522, #14321, #27680, #32724 ) ) ;
#35294 = VERTEX_POINT ( 'NONE', #48645 ) ;
#35295 = AXIS2_PLACEMENT_3D ( 'NONE', #33875, #9453, #42020 ) ;
#35296 = FACE_OUTER_BOUND ( 'NONE', #43266, .T. ) ;
#35297 = ORIENTED_EDGE ( 'NONE', *, *, #44663, .F. ) ;
#35298 = DIRECTION ( 'NONE',  ( -0.000000000000000000, 1.000000000000000000, -0.000000000000000000 ) ) ;
#35299 = CARTESIAN_POINT ( 'NONE',  ( -49.35486169370449971, -175.3837268820161057, 0.4827922027307437469 ) ) ;
#35300 = CARTESIAN_POINT ( 'NONE',  ( -133.0671220150036334, -177.1207230881787780, -92.03190238880748097 ) ) ;
#35301 = LINE ( 'NONE', #4034, #33353 ) ;
#35302 = ORIENTED_EDGE ( 'NONE', *, *, #15654, .F. ) ;
#35303 = ORIENTED_EDGE ( 'NONE', *, *, #385, .F. ) ;
#35304 = ORIENTED_EDGE ( 'NONE', *, *, #38493, .F. ) ;
#35305 = EDGE_CURVE ( 'NONE', #22071, #22595, #38604, .T. ) ;
#35306 = CARTESIAN_POINT ( 'NONE',  ( -132.6364218684650211, -183.6283474603465606, 92.42591454022807795 ) ) ;
#35307 = DIRECTION ( 'NONE',  ( 0.000000000000000000, -0.3546048870425331789, 0.9350162426854158326 ) ) ;
#35308 = CYLINDRICAL_SURFACE ( 'NONE', #16545, 125.0000000000000000 ) ;
#35309 = CARTESIAN_POINT ( 'NONE',  ( 16.00000000000000000, 20.00000000000000355, 1.959434878635766315E-15 ) ) ;
#35310 = DIRECTION ( 'NONE',  ( 0.000000000000000000, 0.000000000000000000, 1.000000000000000000 ) ) ;
#35311 = EDGE_LOOP ( 'NONE', ( #44267, #29532, #51072, #42287 ) ) ;
#35312 = AXIS2_PLACEMENT_3D ( 'NONE', #23143, #11567, #19441 ) ;
#35313 = EDGE_CURVE ( 'NONE', #8712, #194, #50202, .T. ) ;
#35314 = UNCERTAINTY_MEASURE_WITH_UNIT (LENGTH_MEASURE( 1.000000000000000082E-05 ), #5277, 'distance_accuracy_value', 'NONE');
#35315 = EDGE_CURVE ( 'NONE', #5249, #15815, #2606, .T. ) ;
#35316 = CARTESIAN_POINT ( 'NONE',  ( -180.0000000000000568, -123.5000000000000284, 15.24495751795539711 ) ) ;
#35317 = CYLINDRICAL_SURFACE ( 'NONE', #507, 125.0000000000000000 ) ;
#35318 = EDGE_CURVE ( 'NONE', #15872, #22804, #14196, .T. ) ;
#35319 = AXIS2_PLACEMENT_3D ( 'NONE', #36003, #23899, #16035 ) ;
#35320 = EDGE_CURVE ( 'NONE', #51319, #18264, #22315, .T. ) ;
#35321 = ORIENTED_EDGE ( 'NONE', *, *, #13150, .F. ) ;
#35322 = ORIENTED_EDGE ( 'NONE', *, *, #14951, .T. ) ;
#35323 = DIRECTION ( 'NONE',  ( -0.000000000000000000, 1.000000000000000000, -0.000000000000000000 ) ) ;
#35324 = DIRECTION ( 'NONE',  ( 0.000000000000000000, 1.000000000000000000, 0.000000000000000000 ) ) ;
#35325 = ORIENTED_EDGE ( 'NONE', *, *, #31332, .T. ) ;
#35326 = PLANE ( 'NONE',  #4752 ) ;
#35327 = PLANE ( 'NONE',  #11948 ) ;
#35328 = CARTESIAN_POINT ( 'NONE',  ( -330.4913330509368166, -175.5095439275173419, 27.86139516340933042 ) ) ;
#35329 = ORIENTED_EDGE ( 'NONE', *, *, #33062, .T. ) ;
#35330 = DIRECTION ( 'NONE',  ( 0.08879589532292483933, 0.000000000000000000, 0.9960498426152178952 ) ) ;
#35331 = ORIENTED_EDGE ( 'NONE', *, *, #16805, .F. ) ;
#35332 = CARTESIAN_POINT ( 'NONE',  ( -330.4913330509368166, -171.7720157143599238, 33.92731199008539278 ) ) ;
#35333 = CIRCLE ( 'NONE', #26929, 125.0000000000000000 ) ;
#35334 = ADVANCED_FACE ( 'NONE', ( #18642 ), #30975, .T. ) ;
#35335 = CARTESIAN_POINT ( 'NONE',  ( -330.4913330509368166, -123.5000000000000284, 0.000000000000000000 ) ) ;
#35336 = ORIENTED_EDGE ( 'NONE', *, *, #31537, .F. ) ;
#35337 = EDGE_CURVE ( 'NONE', #32161, #49023, #50261, .T. ) ;
#35338 = DIRECTION ( 'NONE',  ( 0.000000000000000000, -0.9927088740980527515, 0.1205366802553337890 ) ) ;
#35339 = DIRECTION ( 'NONE',  ( 0.000000000000000000, 1.000000000000000000, 0.000000000000000000 ) ) ;
#35340 = DIRECTION ( 'NONE',  ( 0.000000000000000000, 1.000000000000000000, 0.000000000000000000 ) ) ;
#35341 = DIRECTION ( 'NONE',  ( -0.000000000000000000, 1.000000000000000000, 0.000000000000000000 ) ) ;
#35342 = ADVANCED_FACE ( 'NONE', ( #29946 ), #47020, .T. ) ;
#35343 = FACE_OUTER_BOUND ( 'NONE', #21557, .T. ) ;
#35344 = EDGE_LOOP ( 'NONE', ( #50618, #21640, #936, #46336 ) ) ;
#35345 = EDGE_LOOP ( 'NONE', ( #46075, #49002, #49669, #20869 ) ) ;
#35346 = DIRECTION ( 'NONE',  ( 0.000000000000000000, 0.9709418174260553425, 0.2393156642875449158 ) ) ;
#35348 = VERTEX_POINT ( 'NONE', #30710 ) ;
#35347 = DIRECTION ( 'NONE',  ( 1.000000000000000000, 0.000000000000000000, -0.000000000000000000 ) ) ;
#35349 = AXIS2_PLACEMENT_3D ( 'NONE', #12779, #4923, #8842 ) ;
#35350 = ORIENTED_EDGE ( 'NONE', *, *, #39691, .F. ) ;
#35351 = CARTESIAN_POINT ( 'NONE',  ( -339.1964088526558498, -178.8432607619606358, 20.45418021416736565 ) ) ;
#35352 = AXIS2_PLACEMENT_3D ( 'NONE', #2199, #14297, #42134 ) ;
#35353 = DIRECTION ( 'NONE',  ( -0.000000000000000000, 1.000000000000000000, -0.000000000000000000 ) ) ;
#35354 = ORIENTED_EDGE ( 'NONE', *, *, #31996, .F. ) ;
#35355 = DIRECTION ( 'NONE',  ( -0.000000000000000000, 1.000000000000000000, -0.000000000000000000 ) ) ;
#35356 = PLANE ( 'NONE',  #44648 ) ;
#35357 = VERTEX_POINT ( 'NONE', #18391 ) ;
#35358 = CYLINDRICAL_SURFACE ( 'NONE', #40072, 125.0000000000000000 ) ;
#35359 = LINE ( 'NONE', #14627, #21920 ) ;
#35360 = LINE ( 'NONE', #15672, #45067 ) ;
#35361 = VERTEX_POINT ( 'NONE', #50453 ) ;
#35362 = VECTOR ( 'NONE', #9443, 1000.000000000000114 ) ;
#35363 = ORIENTED_EDGE ( 'NONE', *, *, #34019, .F. ) ;
#35364 = ORIENTED_EDGE ( 'NONE', *, *, #10893, .F. ) ;
#35365 = LINE ( 'NONE', #38273, #40151 ) ;
#35366 = LINE ( 'NONE', #7528, #37760 ) ;
#35367 = AXIS2_PLACEMENT_3D ( 'NONE', #23731, #27927, #47670 ) ;
#35368 = DIRECTION ( 'NONE',  ( 0.000000000000000000, 0.4647231720437695057, 0.8854560256532093554 ) ) ;
#35369 = DIRECTION ( 'NONE',  ( 0.5338233779647948429, 0.000000000000000000, -0.8455960035018234011 ) ) ;
#35370 = CARTESIAN_POINT ( 'NONE',  ( -330.4913330509368166, -123.0000000000002700, -59.00000000000002132 ) ) ;
#35371 = ORIENTED_EDGE ( 'NONE', *, *, #43007, .F. ) ;
#35372 = ADVANCED_FACE ( 'NONE', ( #6043 ), #7070, .T. ) ;
#35373 = ADVANCED_FACE ( 'NONE', ( #46004 ), #42806, .T. ) ;
#35374 = LINE ( 'NONE', #47475, #1441 ) ;
#35375 = ORIENTED_EDGE ( 'NONE', *, *, #18496, .T. ) ;
#35377 = ORIENTED_EDGE ( 'NONE', *, *, #35269, .F. ) ;
#35376 = DIRECTION ( 'NONE',  ( -0.000000000000000000, 0.9709418174260553425, 0.2393156642875449158 ) ) ;
#35378 = ORIENTED_EDGE ( 'NONE', *, *, #10777, .F. ) ;
#35379 = DIRECTION ( 'NONE',  ( 0.000000000000000000, -0.9709418174260544543, -0.2393156642875482465 ) ) ;
#35380 = CARTESIAN_POINT ( 'NONE',  ( -53.47502265695602119, -193.5000000000000000, -124.9001241957025883 ) ) ;
#35381 = CIRCLE ( 'NONE', #27796, 4.999999999999997335 ) ;
#35382 = FACE_OUTER_BOUND ( 'NONE', #48912, .T. ) ;
#35383 = DIRECTION ( 'NONE',  ( 0.000000000000000000, 1.000000000000000000, 0.000000000000000000 ) ) ;
#35384 = ORIENTED_EDGE ( 'NONE', *, *, #48329, .F. ) ;
#35385 = DIRECTION ( 'NONE',  ( 0.2920567706369628924, 0.000000000000000000, 0.9564009842765264224 ) ) ;
#35386 = AXIS2_PLACEMENT_3D ( 'NONE', #26686, #18540, #49835 ) ;
#35387 = ORIENTED_EDGE ( 'NONE', *, *, #30675, .T. ) ;
#35388 = AXIS2_PLACEMENT_3D ( 'NONE', #47901, #7692, #23216 ) ;
#35389 = ORIENTED_EDGE ( 'NONE', *, *, #20563, .T. ) ;
#35390 = DIRECTION ( 'NONE',  ( 0.000000000000000000, 0.000000000000000000, 1.000000000000000000 ) ) ;
#35391 = CYLINDRICAL_SURFACE ( 'NONE', #4622, 125.0000000000000000 ) ;
#35392 = EDGE_CURVE ( 'NONE', #4433, #10455, #9993, .T. ) ;
#35393 = CARTESIAN_POINT ( 'NONE',  ( 67.04262753014327814, -175.3837268820161057, -47.74645837849745078 ) ) ;
#35394 = CARTESIAN_POINT ( 'NONE',  ( -169.0136227435421006, -189.7472609257535510, -33.11246405730813080 ) ) ;
#35395 = DIRECTION ( 'NONE',  ( 0.000000000000000000, -1.000000000000000000, 0.000000000000000000 ) ) ;
#35396 = DIRECTION ( 'NONE',  ( 0.000000000000000000, 1.000000000000000000, 0.000000000000000000 ) ) ;
#35397 = CARTESIAN_POINT ( 'NONE',  ( -154.0877180371535928, -175.3837268820161057, -66.87170886601928999 ) ) ;
#35398 = ORIENTED_EDGE ( 'NONE', *, *, #18619, .F. ) ;
#35399 = LINE ( 'NONE', #48555, #20451 ) ;
#35400 = CARTESIAN_POINT ( 'NONE',  ( -168.1141659785444915, -177.1207230881787780, -36.22785377503944204 ) ) ;
#35401 = VECTOR ( 'NONE', #35803, 1000.000000000000000 ) ;
#35402 = EDGE_CURVE ( 'NONE', #2850, #34268, #6813, .T. ) ;
#35403 = DIRECTION ( 'NONE',  ( 0.5315839928299667116, 0.000000000000000000, -0.8470055835512242393 ) ) ;
#35404 = ORIENTED_EDGE ( 'NONE', *, *, #10035, .F. ) ;
#35405 = CIRCLE ( 'NONE', #15271, 125.0000000000000000 ) ;
#35406 = CIRCLE ( 'NONE', #16101, 125.0000000000000000 ) ;
#35407 = DIRECTION ( 'NONE',  ( 0.000000000000000000, 0.9927088740980534176, -0.1205366802553268502 ) ) ;
#35408 = CARTESIAN_POINT ( 'NONE',  ( -336.3521761649654422, -182.3871109312487420, -4.498567634386014369 ) ) ;
#35409 = EDGE_LOOP ( 'NONE', ( #20117, #13117, #46844, #30999 ) ) ;
#35410 = CARTESIAN_POINT ( 'NONE',  ( -332.3517673607765914, -65.58448481710581746, 11.56382487286456140 ) ) ;
#35411 = EDGE_CURVE ( 'NONE', #6696, #44669, #8309, .T. ) ;
#35412 = ORIENTED_EDGE ( 'NONE', *, *, #36933, .T. ) ;
#35413 = CARTESIAN_POINT ( 'NONE',  ( -169.6464974000608379, -189.7472609257535510, 26.35287080855539088 ) ) ;
#35414 = FACE_BOUND ( 'NONE', #14648, .T. ) ;
#35416 = EDGE_LOOP ( 'NONE', ( #36046, #31416, #41904, #51527 ) ) ;
#35415 = CARTESIAN_POINT ( 'NONE',  ( -180.0000000000000568, -115.7896721143442278, 60.00000000000000711 ) ) ;
#35417 = VECTOR ( 'NONE', #45248, 1000.000000000000000 ) ;
#35418 = DIRECTION ( 'NONE',  ( -0.000000000000000000, 1.000000000000000000, -0.000000000000000000 ) ) ;
#35419 = ORIENTED_EDGE ( 'NONE', *, *, #49043, .T. ) ;
#35420 = AXIS2_PLACEMENT_3D ( 'NONE', #42534, #6555, #22581 ) ;
#35421 = ADVANCED_FACE ( 'NONE', ( #33881 ), #10483, .F. ) ;
#35422 = ORIENTED_EDGE ( 'NONE', *, *, #36528, .T. ) ;
#35423 = DIRECTION ( 'NONE',  ( -1.000000000000000000, 0.000000000000000000, 0.000000000000000000 ) ) ;
#35424 = VERTEX_POINT ( 'NONE', #34908 ) ;
#35425 = DIRECTION ( 'NONE',  ( 0.000000000000000000, 1.000000000000000000, 0.000000000000000000 ) ) ;
#35426 = EDGE_CURVE ( 'NONE', #21993, #12738, #14970, .T. ) ;
#35427 = VECTOR ( 'NONE', #6614, 1000.000000000000114 ) ;
#35428 = VECTOR ( 'NONE', #10645, 1000.000000000000000 ) ;
#35429 = SURFACE_SIDE_STYLE ('',( #48047 ) ) ;
#35430 = LINE ( 'NONE', #31766, #18893 ) ;
#35431 = ORIENTED_EDGE ( 'NONE', *, *, #32595, .T. ) ;
#35434 = EDGE_LOOP ( 'NONE', ( #20528, #23537, #19878, #44257 ) ) ;
#35433 = SURFACE_STYLE_USAGE ( .BOTH. , #19411 ) ;
#35432 = CARTESIAN_POINT ( 'NONE',  ( -332.3517673607765914, -159.1821513111375452, -47.06073758877369073 ) ) ;
#35435 = AXIS2_PLACEMENT_3D ( 'NONE', #16755, #4139, #36707 ) ;
#35436 = EDGE_CURVE ( 'NONE', #33838, #13263, #18125, .T. ) ;
#35437 = LINE ( 'NONE', #43338, #3820 ) ;
#35438 = EDGE_LOOP ( 'NONE', ( #34240, #31377, #42062, #31585 ) ) ;
#35439 = DIRECTION ( 'NONE',  ( -0.9646355819083594074, 0.000000000000000000, 0.2635871660690647933 ) ) ;
#35440 = DIRECTION ( 'NONE',  ( -0.000000000000000000, 1.000000000000000000, -0.000000000000000000 ) ) ;
#35441 = ORIENTED_EDGE ( 'NONE', *, *, #29149, .F. ) ;
#35443 = CARTESIAN_POINT ( 'NONE',  ( 41.40822382563629134, -177.1207230881787780, 85.41934182508082074 ) ) ;
#35442 = DIRECTION ( 'NONE',  ( -0.2920567706369764371, 0.000000000000000000, 0.9564009842765223146 ) ) ;
#35444 = ORIENTED_EDGE ( 'NONE', *, *, #3178, .T. ) ;
#35445 = DIRECTION ( 'NONE',  ( -0.000000000000000000, 0.000000000000000000, -1.000000000000000000 ) ) ;
#35446 = ORIENTED_EDGE ( 'NONE', *, *, #29337, .F. ) ;
#35447 = CARTESIAN_POINT ( 'NONE',  ( -305.0000000000000568, -153.6873197461136442, -51.85292399224849191 ) ) ;
#35448 = CARTESIAN_POINT ( 'NONE',  ( -160.0000000000000284, -123.5000000000000284, -41.63467731922663972 ) ) ;
#35449 = EDGE_CURVE ( 'NONE', #3470, #47114, #46252, .T. ) ;
#35450 = LINE ( 'NONE', #11275, #30544 ) ;
#35451 = CARTESIAN_POINT ( 'NONE',  ( 60.51025563957495734, -189.7472609257535510, 59.13814366165117065 ) ) ;
#35452 = CARTESIAN_POINT ( 'NONE',  ( -168.1141659785444915, -177.1207230881787780, -36.22785377503943494 ) ) ;
#35453 = AXIS2_PLACEMENT_3D ( 'NONE', #9681, #36765, #32813 ) ;
#35454 = CARTESIAN_POINT ( 'NONE',  ( 60.00000000000001421, -63.50000000000000000, -60.00000000000000711 ) ) ;
#35455 = VERTEX_POINT ( 'NONE', #39110 ) ;
#35456 = DIRECTION ( 'NONE',  ( 0.000000000000000000, 0.000000000000000000, 1.000000000000000000 ) ) ;
#35457 = DIRECTION ( 'NONE',  ( 0.000000000000000000, -1.000000000000000000, -0.000000000000000000 ) ) ;
#35458 = PLANE ( 'NONE',  #12227 ) ;
#35459 = AXIS2_PLACEMENT_3D ( 'NONE', #41554, #21609, #37630 ) ;
#35460 = LINE ( 'NONE', #22874, #43057 ) ;
#35461 = ORIENTED_EDGE ( 'NONE', *, *, #8818, .F. ) ;
#35462 = PLANE ( 'NONE',  #29038 ) ;
#35463 = CARTESIAN_POINT ( 'NONE',  ( -31.30262293407085039, -183.6283474603465606, -123.8142468240611294 ) ) ;
#35464 = DIRECTION ( 'NONE',  ( 0.000000000000000000, -0.000000000000000000, -1.000000000000000000 ) ) ;
#35466 = ORIENTED_EDGE ( 'NONE', *, *, #50823, .F. ) ;
#35465 = CARTESIAN_POINT ( 'NONE',  ( -336.3521761649654422, -180.3949349376675855, 15.70448169564087770 ) ) ;
#35467 = ORIENTED_EDGE ( 'NONE', *, *, #48807, .T. ) ;
#35468 = ORIENTED_EDGE ( 'NONE', *, *, #40065, .T. ) ;
#35469 = CIRCLE ( 'NONE', #15386, 125.0000000000000000 ) ;
#35470 = CIRCLE ( 'NONE', #17050, 125.0000000000000000 ) ;
#35471 = DIRECTION ( 'NONE',  ( -0.000000000000000000, -1.000000000000000000, 0.000000000000000000 ) ) ;
#35472 = AXIS2_PLACEMENT_3D ( 'NONE', #10599, #33991, #2709 ) ;
#35473 = DIRECTION ( 'NONE',  ( -0.000000000000000000, 1.000000000000000000, -0.000000000000000000 ) ) ;
#35474 = DIRECTION ( 'NONE',  ( 0.000000000000000000, 1.000000000000000000, -0.000000000000000000 ) ) ;
#35475 = LINE ( 'NONE', #15527, #30412 ) ;
#35476 = ORIENTED_EDGE ( 'NONE', *, *, #31346, .F. ) ;
#35477 = ADVANCED_FACE ( 'NONE', ( #23365 ), #35960, .F. ) ;
#35478 = EDGE_CURVE ( 'NONE', #20971, #38288, #20040, .T. ) ;
#35479 = CLOSED_SHELL ( 'NONE', ( #15689, #35221, #18203, #29512, #3744, #28033, #15563, #29087, #5016, #8709, #44605, #5370, #44233, #17948, #7200, #27724 ) ) ;
#35480 = CARTESIAN_POINT ( 'NONE',  ( 2.731537303769431269, 57.27118962484799169, -16.80650863900784131 ) ) ;
#35481 = ORIENTED_EDGE ( 'NONE', *, *, #31432, .T. ) ;
#35482 = ORIENTED_EDGE ( 'NONE', *, *, #649, .F. ) ;
#35483 = EDGE_LOOP ( 'NONE', ( #24886, #18896, #12303, #30303 ) ) ;
#35484 = DIRECTION ( 'NONE',  ( 0.000000000000000000, -0.000000000000000000, -1.000000000000000000 ) ) ;
#35485 = AXIS2_PLACEMENT_3D ( 'NONE', #35856, #7742, #22998 ) ;
#35486 = EDGE_CURVE ( 'NONE', #25387, #12506, #31793, .T. ) ;
#35487 = CARTESIAN_POINT ( 'NONE',  ( 30.00000000000000711, 0.000000000000000000, 30.00000000000000355 ) ) ;
#35488 = ORIENTED_EDGE ( 'NONE', *, *, #50692, .F. ) ;
#35489 = EDGE_CURVE ( 'NONE', #30271, #36384, #3904, .T. ) ;
#35490 = VECTOR ( 'NONE', #7700, 1000.000000000000000 ) ;
#35491 = DIRECTION ( 'NONE',  ( 0.000000000000000000, 0.000000000000000000, 1.000000000000000000 ) ) ;
#35492 = CARTESIAN_POINT ( 'NONE',  ( -339.1964088526558498, -182.5000000000000568, 0.5000000000000457412 ) ) ;
#35495 = EDGE_LOOP ( 'NONE', ( #21119, #17745 ) ) ;
#35494 = LINE ( 'NONE', #47089, #34200 ) ;
#35493 = FACE_OUTER_BOUND ( 'NONE', #3522, .T. ) ;
#35496 = ADVANCED_FACE ( 'NONE', ( #31487 ), #39615, .T. ) ;
#35497 = ADVANCED_FACE ( 'NONE', ( #47539 ), #8362, .T. ) ;
#35498 = LINE ( 'NONE', #51052, #51659 ) ;
#35499 = EDGE_LOOP ( 'NONE', ( #47246, #19653 ) ) ;
#35500 = DIRECTION ( 'NONE',  ( -0.6528221181905119463, 0.000000000000000000, -0.7575112421616284619 ) ) ;
#35501 = VERTEX_POINT ( 'NONE', #19160 ) ;
#35502 = CARTESIAN_POINT ( 'NONE',  ( -330.4913330509368166, -108.8949048983204904, 57.16590939599316812 ) ) ;
#35503 = DIRECTION ( 'NONE',  ( 0.000000000000000000, -0.000000000000000000, 1.000000000000000000 ) ) ;
#35505 = CYLINDRICAL_SURFACE ( 'NONE', #25680, 124.9999999999999858 ) ;
#35504 = CARTESIAN_POINT ( 'NONE',  ( -21.64528618042744412, -177.1207230881787780, 121.0625654437174887 ) ) ;
#35506 = AXIS2_PLACEMENT_3D ( 'NONE', #1021, #32822, #13115 ) ;
#35507 = VECTOR ( 'NONE', #34071, 1000.000000000000000 ) ;
#35508 = ORIENTED_EDGE ( 'NONE', *, *, #14171, .T. ) ;
#35509 = CARTESIAN_POINT ( 'NONE',  ( -171.4559849729830603, -193.5000000000000000, 22.39848972532369942 ) ) ;
#35510 = VECTOR ( 'NONE', #23966, 1000.000000000000227 ) ;
#35511 = FACE_OUTER_BOUND ( 'NONE', #28049, .T. ) ;
#35512 = ORIENTED_EDGE ( 'NONE', *, *, #16380, .F. ) ;
#35513 = CARTESIAN_POINT ( 'NONE',  ( -47.74129347246713451, -183.6283474603465606, 0.6749830015182212151 ) ) ;
#35514 = PLANE ( 'NONE',  #28166 ) ;
#35515 = ORIENTED_EDGE ( 'NONE', *, *, #38659, .F. ) ;
#35516 = DIRECTION ( 'NONE',  ( 0.000000000000000000, 0.000000000000000000, -1.000000000000000000 ) ) ;
#35517 = VECTOR ( 'NONE', #14616, 1000.000000000000341 ) ;
#35518 = PLANE ( 'NONE',  #35712 ) ;
#35519 = EDGE_LOOP ( 'NONE', ( #11962, #24444, #29551, #33628 ) ) ;
#35520 = FACE_OUTER_BOUND ( 'NONE', #38766, .T. ) ;
#35521 = ORIENTED_EDGE ( 'NONE', *, *, #39344, .T. ) ;
#35522 = DIRECTION ( 'NONE',  ( 0.000000000000000000, -0.9709418174260502354, 0.2393156642875652051 ) ) ;
#35523 = DIRECTION ( 'NONE',  ( 0.000000000000000000, 0.000000000000000000, 1.000000000000000000 ) ) ;
#35524 = VECTOR ( 'NONE', #1861, 1000.000000000000000 ) ;
#35525 = LINE ( 'NONE', #23710, #27738 ) ;
#35526 = DIRECTION ( 'NONE',  ( -0.000000000000000000, -1.000000000000000000, -0.000000000000000000 ) ) ;
#35527 = CARTESIAN_POINT ( 'NONE',  ( 54.46899307705341187, -183.6283474603465606, -70.89911581792813422 ) ) ;
#35528 = AXIS2_PLACEMENT_3D ( 'NONE', #45700, #10199, #9689 ) ;
#35529 = CARTESIAN_POINT ( 'NONE',  ( 75.60865171534658202, -177.1207230881787780, -15.07392567185468124 ) ) ;
#35530 = DIRECTION ( 'NONE',  ( 0.000000000000000000, 0.000000000000000000, 1.000000000000000000 ) ) ;
#35531 = CARTESIAN_POINT ( 'NONE',  ( -48.30901192927175458, -175.3837268820161057, -123.9998842437354227 ) ) ;
#35533 = ORIENTED_EDGE ( 'NONE', *, *, #1245, .F. ) ;
#35532 = DIRECTION ( 'NONE',  ( -0.000000000000000000, 1.000000000000000000, -0.000000000000000000 ) ) ;
#35534 = ADVANCED_FACE ( 'NONE', ( #28050 ), #36201, .T. ) ;
#35535 = VERTEX_POINT ( 'NONE', #11517 ) ;
#35536 = EDGE_CURVE ( 'NONE', #47044, #41906, #7582, .T. ) ;
#35537 = ADVANCED_FACE ( 'NONE', ( #11771 ), #31757, .F. ) ;
#35538 = CARTESIAN_POINT ( 'NONE',  ( -339.1964088526558498, -109.8658467157464571, 57.40522506028071348 ) ) ;
#35539 = AXIS2_PLACEMENT_3D ( 'NONE', #33257, #8814, #49036 ) ;
#35540 = EDGE_CURVE ( 'NONE', #39811, #5648, #4113, .T. ) ;
#35541 = DIRECTION ( 'NONE',  ( 1.000000000000000000, -0.000000000000000000, 0.000000000000000000 ) ) ;
#35542 = ORIENTED_EDGE ( 'NONE', *, *, #22003, .F. ) ;
#35543 = CIRCLE ( 'NONE', #1113, 60.00000000000000000 ) ;
#35544 = ORIENTED_EDGE ( 'NONE', *, *, #6854, .T. ) ;
#35545 = DIRECTION ( 'NONE',  ( -0.9473263538541923934, 0.000000000000000000, 0.3202698538628350744 ) ) ;
#35546 = ORIENTED_EDGE ( 'NONE', *, *, #51006, .T. ) ;
#35547 = DIRECTION ( 'NONE',  ( 0.000000000000000000, 0.000000000000000000, 1.000000000000000000 ) ) ;
#35548 = DIRECTION ( 'NONE',  ( 0.000000000000000000, -0.9709418174260535661, -0.2393156642875516327 ) ) ;
#35549 = ADVANCED_FACE ( 'NONE', ( #47797 ), #43585, .F. ) ;
#35550 = EDGE_CURVE ( 'NONE', #36303, #29857, #51479, .T. ) ;
#35551 = CARTESIAN_POINT ( 'NONE',  ( -48.13092511607445800, -189.7472609257535510, 0.9374196611341301111 ) ) ;
#35552 = DIRECTION ( 'NONE',  ( -0.000000000000000000, 1.000000000000000000, -0.000000000000000000 ) ) ;
#35553 = EDGE_LOOP ( 'NONE', ( #28439, #18121, #29342, #29652 ) ) ;
#35554 = VERTEX_POINT ( 'NONE', #32001 ) ;
#35555 = EDGE_CURVE ( 'NONE', #32165, #1159, #33488, .T. ) ;
#35556 = EDGE_LOOP ( 'NONE', ( #42637, #10941, #2623, #41941 ) ) ;
#35557 = CARTESIAN_POINT ( 'NONE',  ( 30.05499637021958392, -193.5000000000000000, -97.24912084693205827 ) ) ;
#35558 = CARTESIAN_POINT ( 'NONE',  ( 40.30419662299490113, -193.5000000000000000, -87.99159897727903967 ) ) ;
#35559 = DIRECTION ( 'NONE',  ( 0.000000000000000000, 0.000000000000000000, 1.000000000000000000 ) ) ;
#35560 = EDGE_CURVE ( 'NONE', #14995, #3996, #37681, .T. ) ;
#35561 = CARTESIAN_POINT ( 'NONE',  ( -336.3521761649654422, -180.3949349376675855, 15.70448169564087770 ) ) ;
#35562 = CARTESIAN_POINT ( 'NONE',  ( 9.518239912201957864, -213.5000000000000000, -110.7307791902283043 ) ) ;
#35563 = CIRCLE ( 'NONE', #49847, 4.999999999999997335 ) ;
#35564 = VERTEX_POINT ( 'NONE', #4168 ) ;
#35565 = CARTESIAN_POINT ( 'NONE',  ( 76.48781641346532467, -189.7472609257535510, 2.874563619424060246 ) ) ;
#35566 = ADVANCED_FACE ( 'NONE', ( #32257 ), #12290, .F. ) ;
#35567 = CARTESIAN_POINT ( 'NONE',  ( -21.46839590530488096, -183.6283474603465606, 122.0467960216650880 ) ) ;
#35568 = DIRECTION ( 'NONE',  ( 0.000000000000000000, 0.000000000000000000, 1.000000000000000000 ) ) ;
#35569 = VECTOR ( 'NONE', #29585, 1000.000000000000000 ) ;
#35570 = ORIENTED_EDGE ( 'NONE', *, *, #24401, .F. ) ;
#35571 = EDGE_LOOP ( 'NONE', ( #17954, #29286, #32845, #45733 ) ) ;
#35572 = VERTEX_POINT ( 'NONE', #984 ) ;
#35573 = LINE ( 'NONE', #21764, #13860 ) ;
#35574 = DIRECTION ( 'NONE',  ( -0.9785564922995032555, 0.000000000000000000, -0.2059786187411021818 ) ) ;
#35575 = VERTEX_POINT ( 'NONE', #37509 ) ;
#35576 = CARTESIAN_POINT ( 'NONE',  ( -330.4913330509368166, -95.63860483659122735, -52.00954392751761191 ) ) ;
#35577 = DIRECTION ( 'NONE',  ( -0.8455960035018311727, 0.000000000000000000, 0.5338233779647826305 ) ) ;
#35578 = CARTESIAN_POINT ( 'NONE',  ( -332.3517673607765914, -105.0395444947681369, -56.09938080879045685 ) ) ;
#35579 = ORIENTED_EDGE ( 'NONE', *, *, #3170, .F. ) ;
#35580 = CARTESIAN_POINT ( 'NONE',  ( -336.3521761649654422, -154.8494888031386836, 50.05135858667791382 ) ) ;
#35581 = AXIS2_PLACEMENT_3D ( 'NONE', #34719, #32259, #35690 ) ;
#35582 = EDGE_CURVE ( 'NONE', #22595, #16314, #44617, .T. ) ;
#35583 = ORIENTED_EDGE ( 'NONE', *, *, #22659, .T. ) ;
#35584 = DIRECTION ( 'NONE',  ( 0.000000000000000000, 0.000000000000000000, 1.000000000000000000 ) ) ;
#35585 = LINE ( 'NONE', #11929, #16118 ) ;
#35586 = ORIENTED_EDGE ( 'NONE', *, *, #32069, .T. ) ;
#35587 = LINE ( 'NONE', #31390, #32384 ) ;
#35588 = CARTESIAN_POINT ( 'NONE',  ( -330.4913330509368166, -178.8432607619609200, -20.45418021416661247 ) ) ;
#35589 = CARTESIAN_POINT ( 'NONE',  ( -48.47912675150885065, -177.1207230881787780, 6.938893903907228378E-15 ) ) ;
#35590 = LINE ( 'NONE', #46939, #39164 ) ;
#35591 = ORIENTED_EDGE ( 'NONE', *, *, #44040, .T. ) ;
#35592 = LINE ( 'NONE', #28233, #13561 ) ;
#35593 = EDGE_LOOP ( 'NONE', ( #42809, #39049, #23041, #49561 ) ) ;
#35594 = EDGE_CURVE ( 'NONE', #37599, #21393, #36992, .T. ) ;
#35595 = EDGE_LOOP ( 'NONE', ( #25836, #10101, #19729, #21829 ) ) ;
#35596 = FACE_OUTER_BOUND ( 'NONE', #49574, .T. ) ;
#35598 = ORIENTED_EDGE ( 'NONE', *, *, #27543, .T. ) ;
#35597 = DIRECTION ( 'NONE',  ( 0.000000000000000000, 0.000000000000000000, 1.000000000000000000 ) ) ;
#35599 = VECTOR ( 'NONE', #42102, 1000.000000000000000 ) ;
#35600 = AXIS2_PLACEMENT_3D ( 'NONE', #13624, #17066, #20734 ) ;
#35601 = EDGE_CURVE ( 'NONE', #50590, #8376, #17291, .T. ) ;
#35602 = EDGE_CURVE ( 'NONE', #47240, #1324, #12558, .T. ) ;
#35603 = EDGE_LOOP ( 'NONE', ( #34483, #1385, #38952, #51601 ) ) ;
#35604 = ADVANCED_FACE ( 'NONE', ( #13071 ), #40929, .T. ) ;
#35605 = FACE_OUTER_BOUND ( 'NONE', #8403, .T. ) ;
#35606 = EDGE_CURVE ( 'NONE', #653, #41184, #16783, .T. ) ;
#35607 = CIRCLE ( 'NONE', #12948, 125.0000000000000000 ) ;
#35608 = EDGE_CURVE ( 'NONE', #19641, #35121, #21737, .T. ) ;
#35609 = FACE_OUTER_BOUND ( 'NONE', #9550, .T. ) ;
#35610 = EDGE_LOOP ( 'NONE', ( #3783, #40601, #36973, #49205 ) ) ;
#35611 = CARTESIAN_POINT ( 'NONE',  ( -336.3521761649654422, -81.08339623743702873, -41.09453333279329712 ) ) ;
#35612 = EDGE_CURVE ( 'NONE', #3976, #24651, #4676, .T. ) ;
#35613 = PLANE ( 'NONE',  #40459 ) ;
#35614 = ORIENTED_EDGE ( 'NONE', *, *, #3441, .F. ) ;
#35615 = CARTESIAN_POINT ( 'NONE',  ( -260.0000000000000000, -113.5000000000000142, -60.00000000000001421 ) ) ;
#35616 = DIRECTION ( 'NONE',  ( -0.2348860457809707758, 0.000000000000000000, -0.9720229140804138579 ) ) ;
#35617 = EDGE_CURVE ( 'NONE', #49368, #25876, #17038, .T. ) ;
#35619 = VECTOR ( 'NONE', #6184, 1000.000000000000227 ) ;
#35618 = PLANE ( 'NONE',  #17694 ) ;
#35620 = DIRECTION ( 'NONE',  ( -0.000000000000000000, 1.000000000000000000, 0.000000000000000000 ) ) ;
#35621 = ORIENTED_EDGE ( 'NONE', *, *, #16377, .F. ) ;
#35622 = ORIENTED_EDGE ( 'NONE', *, *, #22257, .F. ) ;
#35623 = ADVANCED_FACE ( 'NONE', ( #5208 ), #32530, .T. ) ;
#35624 = ORIENTED_EDGE ( 'NONE', *, *, #4843, .T. ) ;
#35625 = CARTESIAN_POINT ( 'NONE',  ( -133.0671220150036334, -193.5000000000000000, -92.03190238880748097 ) ) ;
#35626 = CARTESIAN_POINT ( 'NONE',  ( 13.86276369408137477, -175.3837268820161057, -107.1890582354654526 ) ) ;
#35627 = EDGE_CURVE ( 'NONE', #46556, #975, #36739, .T. ) ;
#35628 = PLANE ( 'NONE',  #19270 ) ;
#35629 = MANIFOLD_SOLID_BREP ( 'Chamfer1', #11139 ) ;
#35630 = DIRECTION ( 'NONE',  ( -0.000000000000000000, 0.4647231720437664526, -0.8854560256532110207 ) ) ;
#35631 = DIRECTION ( 'NONE',  ( -0.000000000000000000, 1.000000000000000000, -0.000000000000000000 ) ) ;
#35632 = ORIENTED_EDGE ( 'NONE', *, *, #14268, .T. ) ;
#35633 = EDGE_CURVE ( 'NONE', #9665, #8060, #31822, .T. ) ;
#35634 = EDGE_CURVE ( 'NONE', #25060, #36281, #29359, .T. ) ;
#35635 = DIRECTION ( 'NONE',  ( 0.000000000000000000, 0.000000000000000000, 1.000000000000000000 ) ) ;
#35636 = ORIENTED_EDGE ( 'NONE', *, *, #41082, .T. ) ;
#35638 = EDGE_LOOP ( 'NONE', ( #30566, #22955, #40258, #18803 ) ) ;
#35637 = DIRECTION ( 'NONE',  ( 0.5829794791144762289, 0.000000000000000000, -0.8124868780056783146 ) ) ;
#35639 = ORIENTED_EDGE ( 'NONE', *, *, #4076, .F. ) ;
#35640 = FACE_OUTER_BOUND ( 'NONE', #33181, .T. ) ;
#35641 = CARTESIAN_POINT ( 'NONE',  ( -160.0000000000000284, -123.5000000000000284, 41.63467731922665394 ) ) ;
#35642 = CIRCLE ( 'NONE', #12981, 125.0000000000000000 ) ;
#35643 = AXIS2_PLACEMENT_3D ( 'NONE', #28081, #43611, #39396 ) ;
#35644 = PLANE ( 'NONE',  #5343 ) ;
#35645 = CARTESIAN_POINT ( 'NONE',  ( 65.52619748798558419, -183.6283474603465606, 48.77484799213969069 ) ) ;
#35646 = ORIENTED_EDGE ( 'NONE', *, *, #23696, .F. ) ;
#35647 = CARTESIAN_POINT ( 'NONE',  ( 55.91309001144629320, -183.6283474603465606, 68.75510947788671956 ) ) ;
#35648 = ORIENTED_EDGE ( 'NONE', *, *, #44833, .F. ) ;
#35649 = AXIS2_PLACEMENT_3D ( 'NONE', #48416, #3731, #16350 ) ;
#35650 = ADVANCED_FACE ( 'NONE', ( #10690 ), #9654, .F. ) ;
#35651 = ORIENTED_EDGE ( 'NONE', *, *, #31788, .T. ) ;
#35652 = CARTESIAN_POINT ( 'NONE',  ( -60.00000000000000000, 20.00000000000000000, -60.00000000000000711 ) ) ;
#35653 = PLANE ( 'NONE',  #407 ) ;
#35654 = CARTESIAN_POINT ( 'NONE',  ( -38.66762320617017679, -193.5000000000000000, -124.6143426664033740 ) ) ;
#35655 = FACE_OUTER_BOUND ( 'NONE', #11712, .T. ) ;
#35656 = CIRCLE ( 'NONE', #48274, 125.0000000000000000 ) ;
#35657 = DIRECTION ( 'NONE',  ( 0.000000000000000000, 0.000000000000000000, 1.000000000000000000 ) ) ;
#35658 = DIRECTION ( 'NONE',  ( 0.000000000000000000, 0.000000000000000000, 1.000000000000000000 ) ) ;
#35659 = CARTESIAN_POINT ( 'NONE',  ( -180.0000000000000568, -115.7896721143442278, -60.00000000000000711 ) ) ;
#35660 = ORIENTED_EDGE ( 'NONE', *, *, #7394, .F. ) ;
#35661 = AXIS2_PLACEMENT_3D ( 'NONE', #11136, #7206, #51883 ) ;
#35662 = CARTESIAN_POINT ( 'NONE',  ( -339.1964088526558498, -176.8578783931341150, -27.43969411971490047 ) ) ;
#35663 = LINE ( 'NONE', #48281, #50070 ) ;
#35664 = DIRECTION ( 'NONE',  ( -0.000000000000000000, 0.000000000000000000, -1.000000000000000000 ) ) ;
#35665 = ORIENTED_EDGE ( 'NONE', *, *, #7325, .F. ) ;
#35666 = DIRECTION ( 'NONE',  ( 0.000000000000000000, 1.000000000000000000, 0.000000000000000000 ) ) ;
#35667 = DIRECTION ( 'NONE',  ( 0.000000000000000000, 0.000000000000000000, 1.000000000000000000 ) ) ;
#35668 = EDGE_CURVE ( 'NONE', #24027, #20203, #42481, .T. ) ;
#35669 = ORIENTED_EDGE ( 'NONE', *, *, #16274, .T. ) ;
#35670 = EDGE_CURVE ( 'NONE', #16559, #8474, #18058, .T. ) ;
#35671 = DIRECTION ( 'NONE',  ( -0.8757349421956310831, 0.000000000000000000, -0.4827922027307550712 ) ) ;
#35672 = ORIENTED_EDGE ( 'NONE', *, *, #30340, .T. ) ;
#35673 = LINE ( 'NONE', #30694, #4978 ) ;
#35674 = AXIS2_PLACEMENT_3D ( 'NONE', #47889, #19496, #20021 ) ;
#35675 = FACE_BOUND ( 'NONE', #7050, .T. ) ;
#35677 = ORIENTED_EDGE ( 'NONE', *, *, #11468, .T. ) ;
#35676 = DIRECTION ( 'NONE',  ( 0.5586467658036535777, 0.000000000000000000, -0.8294056854502011022 ) ) ;
#35678 = AXIS2_PLACEMENT_3D ( 'NONE', #14861, #30874, #10899 ) ;
#35679 = AXIS2_PLACEMENT_3D ( 'NONE', #31726, #23832, #8067 ) ;
#35680 = CARTESIAN_POINT ( 'NONE',  ( -48.47912675150885065, -188.5000000000000284, 15.00000000000000711 ) ) ;
#35681 = ORIENTED_EDGE ( 'NONE', *, *, #20192, .T. ) ;
#35682 = AXIS2_PLACEMENT_3D ( 'NONE', #15724, #3880, #7812 ) ;
#35683 = ORIENTED_EDGE ( 'NONE', *, *, #24403, .T. ) ;
#35684 = DIRECTION ( 'NONE',  ( -0.000000000000000000, 1.000000000000000000, -0.000000000000000000 ) ) ;
#35685 = EDGE_LOOP ( 'NONE', ( #41804, #7198, #20861, #393 ) ) ;
#35687 = ADVANCED_FACE ( 'NONE', ( #34586 ), #25681, .T. ) ;
#35686 = CIRCLE ( 'NONE', #3809, 125.0000000000000000 ) ;
#35688 = CARTESIAN_POINT ( 'NONE',  ( -171.4559849729830603, -177.1207230881787780, 22.39848972532369942 ) ) ;
#35689 = CIRCLE ( 'NONE', #46594, 9.000000000000001776 ) ;
#35690 = DIRECTION ( 'NONE',  ( 0.000000000000000000, 0.000000000000000000, 1.000000000000000000 ) ) ;
#35691 = AXIS2_PLACEMENT_3D ( 'NONE', #16593, #32606, #33117 ) ;
#35692 = EDGE_CURVE ( 'NONE', #22760, #16305, #38788, .T. ) ;
#35693 = VECTOR ( 'NONE', #1770, 1000.000000000000000 ) ;
#35694 = DIRECTION ( 'NONE',  ( -0.000000000000000000, 0.5680647467311656929, 0.8229838658936495799 ) ) ;
#35695 = DIRECTION ( 'NONE',  ( -0.000000000000000000, 0.1205366802553199113, -0.9927088740980544168 ) ) ;
#35696 = VERTEX_POINT ( 'NONE', #2794 ) ;
#35698 = ORIENTED_EDGE ( 'NONE', *, *, #48821, .T. ) ;
#35697 = LINE ( 'NONE', #51746, #30870 ) ;
#35699 = ORIENTED_EDGE ( 'NONE', *, *, #28544, .F. ) ;
#35700 = LINE ( 'NONE', #30719, #49148 ) ;
#35701 = ORIENTED_EDGE ( 'NONE', *, *, #31001, .T. ) ;
#35702 = CARTESIAN_POINT ( 'NONE',  ( -7.223120065443615623, -183.6283474603465606, 117.9955164924470523 ) ) ;
#35703 = VERTEX_POINT ( 'NONE', #6758 ) ;
#35704 = LINE ( 'NONE', #3390, #33470 ) ;
#35705 = ORIENTED_EDGE ( 'NONE', *, *, #19539, .T. ) ;
#35707 = DIRECTION ( 'NONE',  ( 1.000000000000000000, 0.000000000000000000, 0.000000000000000000 ) ) ;
#35706 = DIRECTION ( 'NONE',  ( -0.000000000000000000, 1.000000000000000000, 0.000000000000000000 ) ) ;
#35708 = ORIENTED_EDGE ( 'NONE', *, *, #25963, .F. ) ;
#35709 = CARTESIAN_POINT ( 'NONE',  ( -149.9407190013152160, -193.5000000000000000, -73.01058346660458653 ) ) ;
#35710 = EDGE_LOOP ( 'NONE', ( #35014, #32426, #13357, #17922 ) ) ;
#35711 = DIRECTION ( 'NONE',  ( 0.000000000000000000, 0.000000000000000000, 1.000000000000000000 ) ) ;
#35712 = AXIS2_PLACEMENT_3D ( 'NONE', #11862, #44460, #28149 ) ;
#35713 = FACE_OUTER_BOUND ( 'NONE', #17749, .T. ) ;
#35714 = CARTESIAN_POINT ( 'NONE',  ( -48.13092511607445090, -183.6283474603465606, -0.9374196611341135688 ) ) ;
#35715 = DIRECTION ( 'NONE',  ( 0.000000000000000000, 0.1205366802553164696, -0.9927088740980548609 ) ) ;
#35716 = LINE ( 'NONE', #48610, #7308 ) ;
#35717 = CIRCLE ( 'NONE', #4666, 60.00000000000000000 ) ;
#35718 = DIRECTION ( 'NONE',  ( 0.000000000000000000, 1.000000000000000000, 0.000000000000000000 ) ) ;
#35719 = VECTOR ( 'NONE', #45765, 1000.000000000000114 ) ;
#35720 = EDGE_LOOP ( 'NONE', ( #28814, #28823, #28613, #5400 ) ) ;
#35721 = DIRECTION ( 'NONE',  ( 1.000000000000000000, 0.000000000000000000, 0.000000000000000000 ) ) ;
#35722 = FACE_OUTER_BOUND ( 'NONE', #2661, .T. ) ;
#35723 = DIRECTION ( 'NONE',  ( -0.000000000000000000, -1.000000000000000000, -0.000000000000000000 ) ) ;
#35724 = LINE ( 'NONE', #18931, #32133 ) ;
#35725 = ORIENTED_EDGE ( 'NONE', *, *, #48478, .T. ) ;
#35726 = APPLICATION_CONTEXT ( 'automotive_design' ) ;
#35727 = DIRECTION ( 'NONE',  ( 0.000000000000000000, 0.000000000000000000, 1.000000000000000000 ) ) ;
#35728 = VECTOR ( 'NONE', #11607, 1000.000000000000000 ) ;
#35729 = VECTOR ( 'NONE', #14692, 1000.000000000000000 ) ;
#35730 = DIRECTION ( 'NONE',  ( 0.6528221181905280446, 0.000000000000000000, -0.7575112421616145841 ) ) ;
#35732 = ORIENTED_EDGE ( 'NONE', *, *, #11193, .F. ) ;
#35731 = CARTESIAN_POINT ( 'NONE',  ( -1.079983486989452192E-15, 45.00000000000000000, 0.000000000000000000 ) ) ;
#35733 = ADVANCED_FACE ( 'NONE', ( #13859 ), #25938, .T. ) ;
#35734 = ORIENTED_EDGE ( 'NONE', *, *, #19919, .T. ) ;
#35735 = AXIS2_PLACEMENT_3D ( 'NONE', #4964, #12032, #5223 ) ;
#35736 = ORIENTED_EDGE ( 'NONE', *, *, #34439, .T. ) ;
#35737 = CIRCLE ( 'NONE', #45848, 10.00000000000000000 ) ;
#35738 = DIRECTION ( 'NONE',  ( 0.000000000000000000, 0.000000000000000000, 1.000000000000000000 ) ) ;
#35739 = CARTESIAN_POINT ( 'NONE',  ( -305.0000000000000568, -97.07224986041923387, -53.86626052140510978 ) ) ;
#35740 = DIRECTION ( 'NONE',  ( 1.000000000000000000, -0.000000000000000000, -0.000000000000000000 ) ) ;
#35741 = DIRECTION ( 'NONE',  ( 0.000000000000000000, 0.000000000000000000, -1.000000000000000000 ) ) ;
#35742 = ORIENTED_EDGE ( 'NONE', *, *, #40974, .F. ) ;
#35743 = CARTESIAN_POINT ( 'NONE',  ( 4.431967298689001744, 53.65124805090443516, -18.86592383872149981 ) ) ;
#35744 = VERTEX_POINT ( 'NONE', #46188 ) ;
#35745 = ORIENTED_EDGE ( 'NONE', *, *, #24571, .T. ) ;
#35746 = VECTOR ( 'NONE', #9686, 1000.000000000000000 ) ;
#35747 = EDGE_LOOP ( 'NONE', ( #17037, #3285, #37994, #25231 ) ) ;
#35748 = EDGE_CURVE ( 'NONE', #1934, #25631, #5978, .T. ) ;
#35749 = DIRECTION ( 'NONE',  ( 0.8455960035018272869, 0.000000000000000000, -0.5338233779647886257 ) ) ;
#35750 = VECTOR ( 'NONE', #20798, 1000.000000000000114 ) ;
#35751 = AXIS2_PLACEMENT_3D ( 'NONE', #15303, #6393, #39457 ) ;
#35752 = ORIENTED_EDGE ( 'NONE', *, *, #12417, .F. ) ;
#35753 = FILL_AREA_STYLE_COLOUR ( '', #6592 ) ;
#35754 = CARTESIAN_POINT ( 'NONE',  ( 50.88012955800437709, -177.1207230881787780, 74.18852968774250201 ) ) ;
#35757 = ORIENTED_EDGE ( 'NONE', *, *, #41383, .F. ) ;
#35756 = CARTESIAN_POINT ( 'NONE',  ( -48.47912675150885065, -177.1207230881787780, 6.938893903907228378E-15 ) ) ;
#35755 = DIRECTION ( 'NONE',  ( 0.000000000000000000, 0.000000000000000000, -1.000000000000000000 ) ) ;
#35758 = CIRCLE ( 'NONE', #50906, 125.0000000000000000 ) ;
#35759 = AXIS2_PLACEMENT_3D ( 'NONE', #20091, #28226, #48217 ) ;
#35760 = CARTESIAN_POINT ( 'NONE',  ( -305.0000000000000568, -123.5000000000000284, -60.00000000000000000 ) ) ;
#35762 = ORIENTED_EDGE ( 'NONE', *, *, #26907, .F. ) ;
#35761 = AXIS2_PLACEMENT_3D ( 'NONE', #9748, #41273, #22088 ) ;
#35763 = LINE ( 'NONE', #12091, #23897 ) ;
#35764 = VERTEX_POINT ( 'NONE', #14375 ) ;
#35765 = DIRECTION ( 'NONE',  ( -0.7378332790417285736, 0.000000000000000000, 0.6749830015182091136 ) ) ;
#35766 = VECTOR ( 'NONE', #7000, 1000.000000000000114 ) ;
#35767 = CARTESIAN_POINT ( 'NONE',  ( -305.0000000000000568, -179.7763290203206452, 20.80804632820241551 ) ) ;
#35769 = DIRECTION ( 'NONE',  ( -0.000000000000000000, 1.000000000000000000, -0.000000000000000000 ) ) ;
#35768 = DIRECTION ( 'NONE',  ( 0.05924062789371441901, 0.000000000000000000, -0.9982437317643214625 ) ) ;
#35770 = EDGE_LOOP ( 'NONE', ( #5009, #6868, #8197, #5891 ) ) ;
#35771 = CIRCLE ( 'NONE', #20662, 125.0000000000000000 ) ;
#35772 = DIRECTION ( 'NONE',  ( -0.000000000000000000, 1.000000000000000000, -0.000000000000000000 ) ) ;
#35773 = PLANE ( 'NONE',  #48838 ) ;
#35774 =( LENGTH_UNIT ( ) NAMED_UNIT ( * ) SI_UNIT ( .MILLI., .METRE. ) );
#35775 = ORIENTED_EDGE ( 'NONE', *, *, #4476, .F. ) ;
#35776 = DIRECTION ( 'NONE',  ( 0.000000000000000000, 1.000000000000000000, 0.000000000000000000 ) ) ;
#35777 = CARTESIAN_POINT ( 'NONE',  ( -238.7407812814481076, -193.5000000000000000, 10.00000000000000178 ) ) ;
#35778 = CARTESIAN_POINT ( 'NONE',  ( -47.97059563285963435, -175.3837268820161057, 0.8610436117673654355 ) ) ;
#35779 = EDGE_CURVE ( 'NONE', #19701, #32359, #18575, .T. ) ;
#35780 = ORIENTED_EDGE ( 'NONE', *, *, #36002, .F. ) ;
#35781 = LINE ( 'NONE', #43428, #4107 ) ;
#35782 = DIRECTION ( 'NONE',  ( 0.000000000000000000, 0.9350162426854194964, 0.3546048870425235200 ) ) ;
#35783 = ADVANCED_FACE ( 'NONE', ( #30921 ), #2019, .T. ) ;
#35784 = ORIENTED_EDGE ( 'NONE', *, *, #33600, .T. ) ;
#35785 = DIRECTION ( 'NONE',  ( 1.000000000000000000, -0.000000000000000000, 0.000000000000000000 ) ) ;
#35786 = ORIENTED_EDGE ( 'NONE', *, *, #15389, .F. ) ;
#35787 = VECTOR ( 'NONE', #46736, 1000.000000000000000 ) ;
#35788 = AXIS2_PLACEMENT_3D ( 'NONE', #46106, #25334, #41350 ) ;
#35789 = CARTESIAN_POINT ( 'NONE',  ( 64.72501964220592185, -175.3837268820161057, 53.00774697410174952 ) ) ;
#35790 = LINE ( 'NONE', #51848, #27764 ) ;
#35791 = AXIS2_PLACEMENT_3D ( 'NONE', #28408, #44192, #12110 ) ;
#35792 = FACE_OUTER_BOUND ( 'NONE', #37211, .T. ) ;
#35793 = LINE ( 'NONE', #47376, #31447 ) ;
#35794 = DIRECTION ( 'NONE',  ( -0.05924062789370006937, 0.000000000000000000, -0.9982437317643222396 ) ) ;
#35795 = EDGE_CURVE ( 'NONE', #40543, #39339, #14206, .T. ) ;
#35796 = EDGE_CURVE ( 'NONE', #26067, #43448, #2297, .T. ) ;
#35797 = CARTESIAN_POINT ( 'NONE',  ( -339.1964088526558498, -64.99044476834248485, -7.608018572113150135 ) ) ;
#35798 = VECTOR ( 'NONE', #39456, 1000.000000000000000 ) ;
#35799 = EDGE_CURVE ( 'NONE', #24349, #31431, #37766, .T. ) ;
#35800 = AXIS2_PLACEMENT_3D ( 'NONE', #20058, #51121, #19537 ) ;
#35801 = CARTESIAN_POINT ( 'NONE',  ( 2.066935079424583765, -193.5000000000000000, -114.3245189510257802 ) ) ;
#35802 = CARTESIAN_POINT ( 'NONE',  ( -330.4913330509368166, -79.66942718702493664, 39.49849221029193558 ) ) ;
#35804 = ORIENTED_EDGE ( 'NONE', *, *, #39774, .T. ) ;
#35803 = DIRECTION ( 'NONE',  ( -0.000000000000000000, 1.000000000000000000, -0.000000000000000000 ) ) ;
#35805 = MANIFOLD_SOLID_BREP ( 'Cut-Extrude10', #14540 ) ;
#35806 = VECTOR ( 'NONE', #48874, 1000.000000000000000 ) ;
#35807 = VECTOR ( 'NONE', #37926, 1000.000000000000000 ) ;
#35808 = EDGE_LOOP ( 'NONE', ( #31412, #6694, #16195, #1152 ) ) ;
#35809 = CARTESIAN_POINT ( 'NONE',  ( -60.00000000000000000, -43.50000000000000000, 60.00000000000000711 ) ) ;
#35810 = AXIS2_PLACEMENT_3D ( 'NONE', #33512, #13277, #48516 ) ;
#35811 = VECTOR ( 'NONE', #344, 1000.000000000000000 ) ;
#35812 = CARTESIAN_POINT ( 'NONE',  ( -48.47912675150885065, -188.5000000000000284, 6.938893903907228378E-15 ) ) ;
#35813 = VERTEX_POINT ( 'NONE', #27743 ) ;
#35814 = ORIENTED_EDGE ( 'NONE', *, *, #30449, .F. ) ;
#35815 = ORIENTED_EDGE ( 'NONE', *, *, #31162, .T. ) ;
#35816 = EDGE_CURVE ( 'NONE', #34017, #18494, #42217, .T. ) ;
#35817 = LINE ( 'NONE', #44952, #49369 ) ;
#35818 = CARTESIAN_POINT ( 'NONE',  ( -336.3521761649654422, -69.26746417191145611, -23.38292116578723068 ) ) ;
#35819 = CARTESIAN_POINT ( 'NONE',  ( -47.92047998570520662, -183.6283474603465606, 0.8294056854502119824 ) ) ;
#35820 = CARTESIAN_POINT ( 'NONE',  ( -62.32061382540516092, -175.3837268820161057, 123.2250735253144285 ) ) ;
#35821 = VERTEX_POINT ( 'NONE', #31949 ) ;
#35822 = ORIENTED_EDGE ( 'NONE', *, *, #50823, .T. ) ;
#35823 = ORIENTED_EDGE ( 'NONE', *, *, #49465, .F. ) ;
#35824 = DIRECTION ( 'NONE',  ( 0.000000000000000000, 1.000000000000000000, 0.000000000000000000 ) ) ;
#35825 = FACE_OUTER_BOUND ( 'NONE', #14369, .T. ) ;
#35826 = AXIS2_PLACEMENT_3D ( 'NONE', #24815, #32696, #9316 ) ;
#35827 = FACE_OUTER_BOUND ( 'NONE', #42651, .T. ) ;
#35828 = VECTOR ( 'NONE', #9255, 1000.000000000000000 ) ;
#35829 = LINE ( 'NONE', #23744, #20322 ) ;
#35830 = DIRECTION ( 'NONE',  ( -1.000000000000000000, 0.000000000000000000, 0.000000000000000000 ) ) ;
#35831 = EDGE_LOOP ( 'NONE', ( #51901, #7577, #39442, #21671 ) ) ;
#35832 = DIRECTION ( 'NONE',  ( -0.9995608365087940150, 0.000000000000000000, -0.02963332782257007206 ) ) ;
#35833 = VECTOR ( 'NONE', #15330, 1000.000000000000000 ) ;
#35834 = DIRECTION ( 'NONE',  ( 0.000000000000000000, 0.000000000000000000, 1.000000000000000000 ) ) ;
#35835 = CARTESIAN_POINT ( 'NONE',  ( 72.89680503569744019, -193.5000000000000000, -25.37485791684304459 ) ) ;
#35836 = VERTEX_POINT ( 'NONE', #7777 ) ;
#35837 = EDGE_LOOP ( 'NONE', ( #50574, #34781, #19409, #38674 ) ) ;
#35838 = AXIS2_PLACEMENT_3D ( 'NONE', #47921, #35824, #7716 ) ;
#35839 = VERTEX_POINT ( 'NONE', #3058 ) ;
#35840 = CARTESIAN_POINT ( 'NONE',  ( -336.3521761649654422, -126.1322888500942270, -59.00000000000001421 ) ) ;
#35841 = DIRECTION ( 'NONE',  ( 0.000000000000000000, 1.000000000000000000, 0.000000000000000000 ) ) ;
#35842 = AXIS2_PLACEMENT_3D ( 'NONE', #18711, #27355, #23435 ) ;
#35843 = ORIENTED_EDGE ( 'NONE', *, *, #38691, .T. ) ;
#35844 = CARTESIAN_POINT ( 'NONE',  ( -117.6101668435555325, -193.5000000000000000, -102.9412430821794544 ) ) ;
#35845 = VECTOR ( 'NONE', #3707, 1000.000000000000114 ) ;
#35846 = DIRECTION ( 'NONE',  ( -0.000000000000000000, 1.000000000000000000, -0.000000000000000000 ) ) ;
#35847 = ADVANCED_FACE ( 'NONE', ( #43002 ), #7008, .T. ) ;
#35848 = ADVANCED_FACE ( 'NONE', ( #31173 ), #35628, .T. ) ;
#35849 = CARTESIAN_POINT ( 'NONE',  ( -48.47912675150885065, -177.1207230881787780, 6.938893903907228378E-15 ) ) ;
#35850 = VERTEX_POINT ( 'NONE', #15161 ) ;
#35851 = LINE ( 'NONE', #43735, #6589 ) ;
#35852 = PRESENTATION_LAYER_ASSIGNMENT (  '', '', ( #14037 ) ) ;
#35853 = VECTOR ( 'NONE', #29698, 1000.000000000000000 ) ;
#35854 = ORIENTED_EDGE ( 'NONE', *, *, #13734, .F. ) ;
#35855 = DIRECTION ( 'NONE',  ( 0.000000000000000000, 0.000000000000000000, 1.000000000000000000 ) ) ;
#35856 = CARTESIAN_POINT ( 'NONE',  ( -49.08592689732743963, -177.1207230881787780, -0.7948544414133539293 ) ) ;
#35857 = DIRECTION ( 'NONE',  ( 0.1768902751225733261, 0.000000000000000000, -0.9842305779475966077 ) ) ;
#35858 = ORIENTED_EDGE ( 'NONE', *, *, #9901, .F. ) ;
#35859 = CARTESIAN_POINT ( 'NONE',  ( -330.4913330509368166, -123.5000000000000284, 0.000000000000000000 ) ) ;
#35860 = CARTESIAN_POINT ( 'NONE',  ( -74.33510315702946514, -177.1207230881787780, -121.2748789083718748 ) ) ;
#35861 = LINE ( 'NONE', #7499, #28186 ) ;
#35862 = ADVANCED_FACE ( 'NONE', ( #51426 ), #39045, .F. ) ;
#35863 = LINE ( 'NONE', #39784, #9804 ) ;
#35864 = EDGE_CURVE ( 'NONE', #33745, #16360, #15423, .T. ) ;
#35865 = ORIENTED_EDGE ( 'NONE', *, *, #8050, .T. ) ;
#35866 = CARTESIAN_POINT ( 'NONE',  ( 0.000000000000000000, 20.00000000000000355, 20.00000000000000000 ) ) ;
#35867 = ORIENTED_EDGE ( 'NONE', *, *, #37150, .F. ) ;
#35868 = EDGE_LOOP ( 'NONE', ( #41064, #40147, #38687, #752 ) ) ;
#35869 = CIRCLE ( 'NONE', #24106, 125.0000000000000000 ) ;
#35870 = AXIS2_PLACEMENT_3D ( 'NONE', #31247, #47300, #50990 ) ;
#35871 = EDGE_CURVE ( 'NONE', #21665, #13211, #19103, .T. ) ;
#35872 = DIRECTION ( 'NONE',  ( -0.000000000000000000, -0.3546048870425267951, 0.9350162426854181641 ) ) ;
#35874 = VERTEX_POINT ( 'NONE', #27490 ) ;
#35873 = DIRECTION ( 'NONE',  ( 0.000000000000000000, 1.000000000000000000, 0.000000000000000000 ) ) ;
#35875 = CIRCLE ( 'NONE', #19116, 125.0000000000000000 ) ;
#35876 = ADVANCED_FACE ( 'NONE', ( #23549 ), #47469, .T. ) ;
#35877 = ORIENTED_EDGE ( 'NONE', *, *, #47495, .F. ) ;
#35878 = DIRECTION ( 'NONE',  ( -0.000000000000000000, -0.8229838658936596829, -0.5680647467311510379 ) ) ;
#35879 = PLANE ( 'NONE',  #5011 ) ;
#35880 = VECTOR ( 'NONE', #6434, 1000.000000000000000 ) ;
#35881 = ORIENTED_EDGE ( 'NONE', *, *, #38701, .F. ) ;
#35882 = CARTESIAN_POINT ( 'NONE',  ( 0.000000000000000000, -180.7855672281370119, 14.11962419296635396 ) ) ;
#35883 = VECTOR ( 'NONE', #43901, 1000.000000000000000 ) ;
#35884 = DIRECTION ( 'NONE',  ( 0.000000000000000000, 0.000000000000000000, 1.000000000000000000 ) ) ;
#35885 = ORIENTED_EDGE ( 'NONE', *, *, #14472, .F. ) ;
#35886 = CARTESIAN_POINT ( 'NONE',  ( -2.174401709722249887, -177.1207230881787780, -115.0304316645280096 ) ) ;
#35887 = CARTESIAN_POINT ( 'NONE',  ( 76.46082103836693022, -175.3837268820161057, 3.874202661595785191 ) ) ;
#35888 = AXIS2_PLACEMENT_3D ( 'NONE', #37725, #25626, #50339 ) ;
#35889 = VECTOR ( 'NONE', #43609, 1000.000000000000000 ) ;
#35890 = DIRECTION ( 'NONE',  ( -0.000000000000000000, 1.000000000000000000, 0.000000000000000000 ) ) ;
#35891 = DIRECTION ( 'NONE',  ( -0.8455960035018199594, 0.000000000000000000, -0.5338233779648003940 ) ) ;
#35892 = ORIENTED_EDGE ( 'NONE', *, *, #3999, .T. ) ;
#35893 = ORIENTED_EDGE ( 'NONE', *, *, #25013, .T. ) ;
#35894 = ORIENTED_EDGE ( 'NONE', *, *, #8774, .T. ) ;
#35895 = VECTOR ( 'NONE', #4749, 1000.000000000000114 ) ;
#35896 = LINE ( 'NONE', #15936, #12314 ) ;
#35897 = DIRECTION ( 'NONE',  ( 0.000000000000000000, -0.000000000000000000, 1.000000000000000000 ) ) ;
#35898 = CARTESIAN_POINT ( 'NONE',  ( -305.0000000000000568, -89.82879061784676367, -49.66134974749672182 ) ) ;
#35899 = CARTESIAN_POINT ( 'NONE',  ( -332.3517673607765914, -169.4076645216271402, -37.15394033962039089 ) ) ;
#35900 = DIRECTION ( 'NONE',  ( -1.000000000000000000, -0.000000000000000000, -0.000000000000000000 ) ) ;
#35901 = VERTEX_POINT ( 'NONE', #43530 ) ;
#35902 = DIRECTION ( 'NONE',  ( -0.3482016354344059095, 0.000000000000000000, 0.9374196611341183427 ) ) ;
#35903 = EDGE_CURVE ( 'NONE', #21423, #40951, #7530, .T. ) ;
#35904 = ORIENTED_EDGE ( 'NONE', *, *, #10225, .F. ) ;
#35906 = EDGE_LOOP ( 'NONE', ( #29737, #11364, #47150, #9753 ) ) ;
#35905 = CARTESIAN_POINT ( 'NONE',  ( 12.54192669111252734, -183.6283474603465606, 107.9473519284347418 ) ) ;
#35907 = AXIS2_PLACEMENT_3D ( 'NONE', #6711, #51376, #42950 ) ;
#35908 = ORIENTED_EDGE ( 'NONE', *, *, #21324, .T. ) ;
#35909 = AXIS2_PLACEMENT_3D ( 'NONE', #50925, #39067, #51192 ) ;
#35910 = FACE_OUTER_BOUND ( 'NONE', #12066, .T. ) ;
#35911 = DIRECTION ( 'NONE',  ( 0.000000000000000000, -1.000000000000000000, 0.000000000000000000 ) ) ;
#35912 = AXIS2_PLACEMENT_3D ( 'NONE', #41566, #37894, #13988 ) ;
#35913 = EDGE_CURVE ( 'NONE', #50038, #30132, #24079, .T. ) ;
#35914 = DIRECTION ( 'NONE',  ( 0.000000000000000000, -1.000000000000000000, 0.000000000000000000 ) ) ;
#35915 = EDGE_CURVE ( 'NONE', #8372, #34970, #16765, .T. ) ;
#35916 = EDGE_CURVE ( 'NONE', #10098, #7641, #35118, .T. ) ;
#35917 = DIRECTION ( 'NONE',  ( 0.6068001458186002006, 0.000000000000000000, -0.7948544414133481562 ) ) ;
#35918 = ORIENTED_EDGE ( 'NONE', *, *, #18982, .T. ) ;
#35919 = CARTESIAN_POINT ( 'NONE',  ( -180.0000000000000568, -123.5000000000000284, -15.24495751795539000 ) ) ;
#35920 = ORIENTED_EDGE ( 'NONE', *, *, #14677, .F. ) ;
#35921 = ADVANCED_FACE ( 'NONE', ( #19607 ), #15680, .T. ) ;
#35922 = ORIENTED_EDGE ( 'NONE', *, *, #30096, .F. ) ;
#35923 = VECTOR ( 'NONE', #37828, 999.9999999999998863 ) ;
#35924 = ADVANCED_FACE ( 'NONE', ( #51949 ), #15938, .T. ) ;
#35925 = DIRECTION ( 'NONE',  ( 1.000000000000000000, -1.050884489711542826E-17, 8.654812430365590163E-17 ) ) ;
#35926 = CARTESIAN_POINT ( 'NONE',  ( -336.3521761649654422, -65.24746378767824240, -9.724760635741734660 ) ) ;
#35927 = CARTESIAN_POINT ( 'NONE',  ( -332.3517673607765914, -67.75522407825191351, 19.39547174791671935 ) ) ;
#35928 = CARTESIAN_POINT ( 'NONE',  ( -339.1964088526558498, -68.51134412508183402, -21.38919645685240312 ) ) ;
#35929 = ADVANCED_FACE ( 'NONE', ( #20120 ), #36149, .T. ) ;
#35930 = ORIENTED_EDGE ( 'NONE', *, *, #29152, .F. ) ;
#35931 = LINE ( 'NONE', #16482, #4523 ) ;
#35932 = CARTESIAN_POINT ( 'NONE',  ( 45.66222513722992460, -193.5000000000000000, 80.70646587903453906 ) ) ;
#35933 = EDGE_CURVE ( 'NONE', #12706, #46515, #33945, .T. ) ;
#35934 = AXIS2_PLACEMENT_3D ( 'NONE', #29427, #28905, #9472 ) ;
#35935 = FACE_BOUND ( 'NONE', #9178, .T. ) ;
#35936 = ORIENTED_EDGE ( 'NONE', *, *, #3849, .F. ) ;
#35937 = EDGE_CURVE ( 'NONE', #28874, #3974, #24327, .T. ) ;
#35938 = DIRECTION ( 'NONE',  ( -0.000000000000000000, 1.000000000000000000, -0.000000000000000000 ) ) ;
#35939 = DIRECTION ( 'NONE',  ( -0.000000000000000000, -1.000000000000000000, -0.000000000000000000 ) ) ;
#35940 = EDGE_CURVE ( 'NONE', #48835, #41991, #48773, .T. ) ;
#35941 = VERTEX_POINT ( 'NONE', #44315 ) ;
#35942 = DIRECTION ( 'NONE',  ( 0.000000000000000000, 1.000000000000000000, 0.000000000000000000 ) ) ;
#35943 = ORIENTED_EDGE ( 'NONE', *, *, #5838, .F. ) ;
#35944 = EDGE_CURVE ( 'NONE', #37865, #41127, #24283, .T. ) ;
#35945 = EDGE_CURVE ( 'NONE', #27120, #32525, #32472, .T. ) ;
#35946 =( GEOMETRIC_REPRESENTATION_CONTEXT ( 3 ) GLOBAL_UNCERTAINTY_ASSIGNED_CONTEXT ( ( #2740 ) ) GLOBAL_UNIT_ASSIGNED_CONTEXT ( ( #29982, #42313, #46037 ) ) REPRESENTATION_CONTEXT ( 'NONE', 'WORKASPACE' ) );
#35947 = LINE ( 'NONE', #8350, #20073 ) ;
#35948 = VECTOR ( 'NONE', #17711, 1000.000000000000000 ) ;
#35949 = CIRCLE ( 'NONE', #42663, 60.00000000000000000 ) ;
#35950 = FACE_BOUND ( 'NONE', #18641, .T. ) ;
#35951 = LINE ( 'NONE', #16499, #10317 ) ;
#35952 = VECTOR ( 'NONE', #11831, 1000.000000000000114 ) ;
#35953 = CARTESIAN_POINT ( 'NONE',  ( -33.52607327456454556, -175.3837268820161057, -124.1024020384603119 ) ) ;
#35954 = ADVANCED_FACE ( 'NONE', ( #44820 ), #49999, .F. ) ;
#35955 = VERTEX_POINT ( 'NONE', #40865 ) ;
#35956 = EDGE_LOOP ( 'NONE', ( #864, #19022, #42554, #34507 ) ) ;
#35957 = CARTESIAN_POINT ( 'NONE',  ( 75.01583293582056911, -175.3837268820161057, 11.18012358327989375 ) ) ;
#35958 = VECTOR ( 'NONE', #37763, 1000.000000000000000 ) ;
#35959 = ORIENTED_EDGE ( 'NONE', *, *, #29216, .F. ) ;
#35960 = PLANE ( 'NONE',  #39354 ) ;
#35961 = DIRECTION ( 'NONE',  ( 0.000000000000000000, 0.000000000000000000, -1.000000000000000000 ) ) ;
#35962 = AXIS2_PLACEMENT_3D ( 'NONE', #23875, #3921, #35976 ) ;
#35963 = DIRECTION ( 'NONE',  ( 0.000000000000000000, 0.000000000000000000, -1.000000000000000000 ) ) ;
#35964 = CARTESIAN_POINT ( 'NONE',  ( -50.83192613281180172, -193.5000000000000000, 123.9784823535113816 ) ) ;
#35965 = EDGE_LOOP ( 'NONE', ( #40149, #16200, #14063, #11204 ) ) ;
#35968 = ORIENTED_EDGE ( 'NONE', *, *, #9969, .T. ) ;
#35967 = CARTESIAN_POINT ( 'NONE',  ( -305.0000000000000568, -162.9117225908391333, -45.24064679492040852 ) ) ;
#35966 = CARTESIAN_POINT ( 'NONE',  ( 42.10477485469927927, -183.6283474603465606, 86.13684908212515268 ) ) ;
#35969 = ORIENTED_EDGE ( 'NONE', *, *, #8935, .T. ) ;
#35970 = LINE ( 'NONE', #47030, #14750 ) ;
#35971 = ORIENTED_EDGE ( 'NONE', *, *, #4849, .F. ) ;
#35972 = CARTESIAN_POINT ( 'NONE',  ( 66.42899531795131907, -183.6283474603465606, 49.20491319441622124 ) ) ;
#35973 = ORIENTED_EDGE ( 'NONE', *, *, #6971, .T. ) ;
#35974 = ADVANCED_FACE ( 'NONE', ( #13005 ), #20378, .T. ) ;
#35975 = ADVANCED_FACE ( 'NONE', ( #36403 ), #10054, .F. ) ;
#35976 = DIRECTION ( 'NONE',  ( 0.000000000000000000, 0.000000000000000000, -1.000000000000000000 ) ) ;
#35977 = ORIENTED_EDGE ( 'NONE', *, *, #32988, .T. ) ;
#35979 = DIRECTION ( 'NONE',  ( 0.000000000000000000, 1.000000000000000000, 0.000000000000000000 ) ) ;
#35978 = LINE ( 'NONE', #40170, #39233 ) ;
#35980 = ORIENTED_EDGE ( 'NONE', *, *, #34025, .T. ) ;
#35981 = EDGE_CURVE ( 'NONE', #33577, #40405, #41131, .T. ) ;
#35982 = EDGE_CURVE ( 'NONE', #31431, #2085, #8344, .T. ) ;
#35983 = AXIS2_PLACEMENT_3D ( 'NONE', #43613, #43365, #7613 ) ;
#35984 = ORIENTED_EDGE ( 'NONE', *, *, #38093, .F. ) ;
#35985 = LINE ( 'NONE', #35447, #48910 ) ;
#35986 = VECTOR ( 'NONE', #48476, 1000.000000000000114 ) ;
#35987 = CARTESIAN_POINT ( 'NONE',  ( -122.3978016498073345, -193.5000000000000000, -100.8019320314827070 ) ) ;
#35988 = COLOUR_RGB ( '', 0.40784314, 0.44705882, 0.49803922) ;
#35989 = DIRECTION ( 'NONE',  ( 0.6300878435817038881, 0.000000000000000000, 0.7765238627180482966 ) ) ;
#35990 = PLANE ( 'NONE',  #26545 ) ;
#35991 = CARTESIAN_POINT ( 'NONE',  ( -140.1460956102404509, -175.3837268820161057, 84.98333260264820410 ) ) ;
#35992 = VECTOR ( 'NONE', #30212, 1000.000000000000000 ) ;
#35993 = DIRECTION ( 'NONE',  ( -0.000000000000000000, 1.000000000000000000, 0.000000000000000000 ) ) ;
#35994 = ORIENTED_EDGE ( 'NONE', *, *, #36263, .F. ) ;
#35995 = CARTESIAN_POINT ( 'NONE',  ( 0.000000000000000000, 0.000000000000000000, 0.000000000000000000 ) ) ;
#35996 = CARTESIAN_POINT ( 'NONE',  ( 73.80528149577284580, -175.3837268820161057, 25.91377046305969145 ) ) ;
#35997 = CARTESIAN_POINT ( 'NONE',  ( -47.64924157374594671, -175.3837268820161057, 123.9972451320097377 ) ) ;
#35998 = DIRECTION ( 'NONE',  ( -0.000000000000000000, -1.000000000000000000, 0.000000000000000000 ) ) ;
#35999 = ORIENTED_EDGE ( 'NONE', *, *, #27910, .F. ) ;
#36000 = CIRCLE ( 'NONE', #41850, 125.0000000000000000 ) ;
#36001 = DIRECTION ( 'NONE',  ( 0.000000000000000000, 0.000000000000000000, 1.000000000000000000 ) ) ;
#36002 = EDGE_CURVE ( 'NONE', #5608, #11764, #41914, .T. ) ;
#36003 = CARTESIAN_POINT ( 'NONE',  ( -305.0000000000000568, -123.5000000000000284, 0.000000000000000000 ) ) ;
#36004 = CYLINDRICAL_SURFACE ( 'NONE', #11874, 125.0000000000000000 ) ;
#36005 = ORIENTED_EDGE ( 'NONE', *, *, #45737, .F. ) ;
#36006 = ORIENTED_EDGE ( 'NONE', *, *, #42575, .F. ) ;
#36007 = ORIENTED_EDGE ( 'NONE', *, *, #10832, .T. ) ;
#36008 = EDGE_CURVE ( 'NONE', #40165, #21836, #46103, .T. ) ;
#36009 = VECTOR ( 'NONE', #44836, 1000.000000000000000 ) ;
#36010 = DIRECTION ( 'NONE',  ( 0.5085311186492273983, 0.000000000000000000, -0.8610436117673514467 ) ) ;
#36011 = PLANE ( 'NONE',  #17807 ) ;
#36012 = DIRECTION ( 'NONE',  ( 0.000000000000000000, 0.000000000000000000, -1.000000000000000000 ) ) ;
#36013 = DIRECTION ( 'NONE',  ( -0.000000000000000000, 1.000000000000000000, 0.000000000000000000 ) ) ;
#36014 = ORIENTED_EDGE ( 'NONE', *, *, #22486, .F. ) ;
#36015 = DIRECTION ( 'NONE',  ( 1.000000000000000000, 0.000000000000000000, -0.000000000000000000 ) ) ;
#36016 = ORIENTED_EDGE ( 'NONE', *, *, #9468, .F. ) ;
#36017 = EDGE_LOOP ( 'NONE', ( #9151, #28087, #28551, #2789 ) ) ;
#36018 = ORIENTED_EDGE ( 'NONE', *, *, #7644, .T. ) ;
#36019 = AXIS2_PLACEMENT_3D ( 'NONE', #48291, #20960, #28563 ) ;
#36020 = ORIENTED_EDGE ( 'NONE', *, *, #35602, .F. ) ;
#36021 = DIRECTION ( 'NONE',  ( 0.000000000000000000, 0.000000000000000000, -1.000000000000000000 ) ) ;
#36022 = EDGE_LOOP ( 'NONE', ( #38063, #13437, #16887, #30983 ) ) ;
#36023 = DIRECTION ( 'NONE',  ( 0.000000000000000000, -1.000000000000000000, -0.000000000000000000 ) ) ;
#36024 = FACE_OUTER_BOUND ( 'NONE', #20399, .T. ) ;
#36027 = ORIENTED_EDGE ( 'NONE', *, *, #20670, .F. ) ;
#36026 = LINE ( 'NONE', #40216, #51847 ) ;
#36025 = DIRECTION ( 'NONE',  ( -0.8838680338115276758, 0.000000000000000000, 0.4677363560876407478 ) ) ;
#36028 = CARTESIAN_POINT ( 'NONE',  ( -162.0868781531755758, -177.1207230881787780, -49.69312418816311094 ) ) ;
#36029 = ORIENTED_EDGE ( 'NONE', *, *, #24731, .F. ) ;
#36030 = CARTESIAN_POINT ( 'NONE',  ( -336.3521761649654422, -69.26746417191145611, -23.38292116578723068 ) ) ;
#36031 = ORIENTED_EDGE ( 'NONE', *, *, #3239, .T. ) ;
#36032 = ADVANCED_FACE ( 'NONE', ( #29033 ), #16974, .T. ) ;
#36033 = CARTESIAN_POINT ( 'NONE',  ( -336.3521761649654422, -165.9166037625627439, 41.09453333279358134 ) ) ;
#36034 = CARTESIAN_POINT ( 'NONE',  ( 57.31108707223382481, -193.5000000000000000, -66.58401203837755133 ) ) ;
#36036 = CARTESIAN_POINT ( 'NONE',  ( -49.42645310536303782, -175.3837268820161057, -0.3202698538628417357 ) ) ;
#36035 = LINE ( 'NONE', #43912, #26583 ) ;
#36037 = ORIENTED_EDGE ( 'NONE', *, *, #35402, .F. ) ;
#36038 = VECTOR ( 'NONE', #22350, 1000.000000000000114 ) ;
#36039 = LINE ( 'NONE', #36826, #16436 ) ;
#36040 = CARTESIAN_POINT ( 'NONE',  ( -129.9529520667707629, -189.7472609257535510, -94.79987230211962412 ) ) ;
#36041 = FACE_OUTER_BOUND ( 'NONE', #23252, .T. ) ;
#36042 = VERTEX_POINT ( 'NONE', #44559 ) ;
#36043 = SURFACE_SIDE_STYLE ('',( #4771 ) ) ;
#36044 = LINE ( 'NONE', #24737, #19008 ) ;
#36045 = DIRECTION ( 'NONE',  ( 0.000000000000000000, -0.000000000000000000, 1.000000000000000000 ) ) ;
#36046 = ORIENTED_EDGE ( 'NONE', *, *, #7472, .T. ) ;
#36047 = DIRECTION ( 'NONE',  ( -0.4031234292879665171, 0.000000000000000000, -0.9151456172430210145 ) ) ;
#36048 = LINE ( 'NONE', #48406, #39044 ) ;
#36049 = ORIENTED_EDGE ( 'NONE', *, *, #18638, .T. ) ;
#36050 = CARTESIAN_POINT ( 'NONE',  ( -98.62206515315352817, -175.3837268820161057, 113.4093733337831225 ) ) ;
#36051 = ORIENTED_EDGE ( 'NONE', *, *, #12187, .T. ) ;
#36052 = AXIS2_PLACEMENT_3D ( 'NONE', #2779, #34571, #10930 ) ;
#36053 = CARTESIAN_POINT ( 'NONE',  ( -332.3517673607765914, -171.1288023355047585, 34.85916744524404720 ) ) ;
#36054 = DIRECTION ( 'NONE',  ( 0.000000000000000000, -1.137978600240785454E-13, -1.000000000000000000 ) ) ;
#36055 = EDGE_CURVE ( 'NONE', #7418, #31469, #24579, .T. ) ;
#36056 = FACE_OUTER_BOUND ( 'NONE', #43479, .T. ) ;
#36057 = LINE ( 'NONE', #7442, #39837 ) ;
#36058 = CARTESIAN_POINT ( 'NONE',  ( -330.4913330509368166, -171.7720157143604069, -33.92731199008473197 ) ) ;
#36059 = ADVANCED_FACE ( 'NONE', ( #32977, #4613 ), #2150, .T. ) ;
#36060 = DIRECTION ( 'NONE',  ( -1.000000000000000000, 0.000000000000000000, -4.884776371667511665E-16 ) ) ;
#36061 = CARTESIAN_POINT ( 'NONE',  ( -120.2975302769383177, -193.5000000000000000, 102.3089288139533863 ) ) ;
#36062 = CARTESIAN_POINT ( 'NONE',  ( -8.721998590732173540, -183.6283474603465606, -118.5089480183145128 ) ) ;
#36064 = VERTEX_POINT ( 'NONE', #1899 ) ;
#36063 = CARTESIAN_POINT ( 'NONE',  ( 71.15591247552653442, -177.1207230881787780, 36.22785377504035154 ) ) ;
#36065 = ORIENTED_EDGE ( 'NONE', *, *, #4777, .F. ) ;
#36066 = LINE ( 'NONE', #12407, #30810 ) ;
#36067 = EDGE_CURVE ( 'NONE', #43082, #23765, #47776, .T. ) ;
#36068 = AXIS2_PLACEMENT_3D ( 'NONE', #47738, #36401, #43773 ) ;
#36069 = VECTOR ( 'NONE', #34510, 1000.000000000000000 ) ;
#36070 = DIRECTION ( 'NONE',  ( 0.9374196611341231167, 0.000000000000000000, -0.3482016354343928088 ) ) ;
#36071 = VERTEX_POINT ( 'NONE', #30790 ) ;
#36072 = ORIENTED_EDGE ( 'NONE', *, *, #39775, .F. ) ;
#36073 = ORIENTED_EDGE ( 'NONE', *, *, #29096, .F. ) ;
#36074 = CARTESIAN_POINT ( 'NONE',  ( -138.3664773286546108, -193.5000000000000000, -85.41934182508015283 ) ) ;
#36075 = CARTESIAN_POINT ( 'NONE',  ( -158.3442440847886985, -175.3837268820161057, -59.62093586438118109 ) ) ;
#36076 = CARTESIAN_POINT ( 'NONE',  ( -65.47874029382337824, -183.6283474603465606, 122.8300162461137006 ) ) ;
#36077 = DIRECTION ( 'NONE',  ( -0.5085311186492094127, 0.000000000000000000, -0.8610436117673619938 ) ) ;
#36078 = ORIENTED_EDGE ( 'NONE', *, *, #14096, .T. ) ;
#36079 = ORIENTED_EDGE ( 'NONE', *, *, #644, .F. ) ;
#36080 = EDGE_LOOP ( 'NONE', ( #30, #31620, #40349, #11397 ) ) ;
#36081 = ADVANCED_FACE ( 'NONE', ( #50516 ), #51046, .F. ) ;
#36082 = DIRECTION ( 'NONE',  ( -0.000000000000000000, 1.000000000000000000, -0.000000000000000000 ) ) ;
#36083 = CARTESIAN_POINT ( 'NONE',  ( 76.47090317495664635, -189.7472609257535510, -3.534122433557455256 ) ) ;
#36084 = CARTESIAN_POINT ( 'NONE',  ( -16.77927958806650821, -183.6283474603465606, -120.9136869416130082 ) ) ;
#36085 = AXIS2_PLACEMENT_3D ( 'NONE', #790, #17096, #20492 ) ;
#36086 = CARTESIAN_POINT ( 'NONE',  ( -330.4913330509368166, -79.00630452878421295, 38.74998146212088557 ) ) ;
#36087 = LINE ( 'NONE', #27686, #6298 ) ;
#36088 = ORIENTED_EDGE ( 'NONE', *, *, #46549, .F. ) ;
#36089 = CARTESIAN_POINT ( 'NONE',  ( -339.1964088526558498, -116.8846903019852164, -58.63009191191289915 ) ) ;
#36090 = EDGE_CURVE ( 'NONE', #2653, #22822, #50265, .T. ) ;
#36091 = CARTESIAN_POINT ( 'NONE',  ( 42.96730897722186171, 30.00000000000000355, -41.16782622478179832 ) ) ;
#36092 = CARTESIAN_POINT ( 'NONE',  ( -91.49662025983745650, -189.7472609257535510, -116.2991637277475547 ) ) ;
#36093 = DIRECTION ( 'NONE',  ( 1.000000000000000000, 0.000000000000000000, 0.000000000000000000 ) ) ;
#36094 = EDGE_LOOP ( 'NONE', ( #20920, #37228, #15607, #38735 ) ) ;
#36095 = ORIENTED_EDGE ( 'NONE', *, *, #2799, .F. ) ;
#36096 = EDGE_CURVE ( 'NONE', #22268, #11734, #34722, .T. ) ;
#36097 = ORIENTED_EDGE ( 'NONE', *, *, #2230, .F. ) ;
#36098 = DIRECTION ( 'NONE',  ( -0.000000000000000000, 1.000000000000000000, 0.000000000000000000 ) ) ;
#36099 = DIRECTION ( 'NONE',  ( -0.000000000000000000, 0.9927088740980538617, -0.1205366802553232974 ) ) ;
#36100 = ORIENTED_EDGE ( 'NONE', *, *, #42312, .F. ) ;
#36101 = PLANE ( 'NONE',  #5590 ) ;
#36102 = CARTESIAN_POINT ( 'NONE',  ( -30.31202594373734627, -193.5000000000000000, -123.6727797384705809 ) ) ;
#36103 = EDGE_CURVE ( 'NONE', #26805, #28748, #14515, .T. ) ;
#36104 = FACE_OUTER_BOUND ( 'NONE', #15865, .T. ) ;
#36105 = ORIENTED_EDGE ( 'NONE', *, *, #916, .F. ) ;
#36106 = FACE_OUTER_BOUND ( 'NONE', #8162, .T. ) ;
#36107 = CIRCLE ( 'NONE', #3364, 125.0000000000000000 ) ;
#36108 = VECTOR ( 'NONE', #42845, 999.9999999999998863 ) ;
#36109 = VERTEX_POINT ( 'NONE', #19230 ) ;
#36110 = LINE ( 'NONE', #31909, #46701 ) ;
#36111 = ORIENTED_EDGE ( 'NONE', *, *, #39812, .T. ) ;
#36112 = PLANE ( 'NONE',  #12841 ) ;
#36113 = DIRECTION ( 'NONE',  ( 0.000000000000000000, 0.000000000000000000, 1.000000000000000000 ) ) ;
#36114 = ADVANCED_FACE ( 'NONE', ( #22907 ), #38415, .T. ) ;
#36115 = ORIENTED_EDGE ( 'NONE', *, *, #36067, .T. ) ;
#36116 = DIRECTION ( 'NONE',  ( -0.9266896074318317078, 0.000000000000000000, -0.3758275821142421647 ) ) ;
#36117 = DIRECTION ( 'NONE',  ( 1.000000000000000000, -0.000000000000000000, 0.000000000000000000 ) ) ;
#36118 = CARTESIAN_POINT ( 'NONE',  ( -336.3521761649654422, -70.49953203435293858, 25.97334715265942151 ) ) ;
#36119 = DIRECTION ( 'NONE',  ( -0.000000000000000000, 1.000000000000000000, -0.000000000000000000 ) ) ;
#36120 = ORIENTED_EDGE ( 'NONE', *, *, #635, .F. ) ;
#36121 = CARTESIAN_POINT ( 'NONE',  ( 65.38692482895591240, -193.5000000000000000, -51.57055649762701677 ) ) ;
#36122 = EDGE_LOOP ( 'NONE', ( #20928, #48107, #22298, #46376 ) ) ;
#36123 = ORIENTED_EDGE ( 'NONE', *, *, #50415, .F. ) ;
#36124 = VECTOR ( 'NONE', #18320, 999.9999999999998863 ) ;
#36125 = DIRECTION ( 'NONE',  ( 0.000000000000000000, 0.9927088740980556381, 0.1205366802553095168 ) ) ;
#36127 = ORIENTED_EDGE ( 'NONE', *, *, #48297, .F. ) ;
#36126 = FACE_OUTER_BOUND ( 'NONE', #15606, .T. ) ;
#36128 = VERTEX_POINT ( 'NONE', #31039 ) ;
#36129 = PLANE ( 'NONE',  #43889 ) ;
#36130 = DIRECTION ( 'NONE',  ( 0.000000000000000000, 0.000000000000000000, 1.000000000000000000 ) ) ;
#36131 = ORIENTED_EDGE ( 'NONE', *, *, #633, .F. ) ;
#36132 = DIRECTION ( 'NONE',  ( 0.000000000000000000, -0.8229838658936536877, 0.5680647467311596976 ) ) ;
#36133 = FACE_OUTER_BOUND ( 'NONE', #50556, .T. ) ;
#36134 = ORIENTED_EDGE ( 'NONE', *, *, #2143, .T. ) ;
#36135 = CARTESIAN_POINT ( 'NONE',  ( -330.4913330509368166, -175.5095439275177398, -27.86139516340860212 ) ) ;
#36136 = CARTESIAN_POINT ( 'NONE',  ( -336.3521761649654422, -123.5000000000000284, 0.000000000000000000 ) ) ;
#36137 = VECTOR ( 'NONE', #29521, 999.9999999999998863 ) ;
#36138 = EDGE_CURVE ( 'NONE', #39416, #29039, #26839, .T. ) ;
#36139 = EDGE_CURVE ( 'NONE', #4082, #17420, #38664, .T. ) ;
#36140 = CARTESIAN_POINT ( 'NONE',  ( -330.4913330509368166, -84.08827740916123616, -45.24064679492067853 ) ) ;
#36141 = DIRECTION ( 'NONE',  ( 0.000000000000000000, 0.000000000000000000, -1.000000000000000000 ) ) ;
#36142 = EDGE_LOOP ( 'NONE', ( #25372, #33121 ) ) ;
#36143 = VERTEX_POINT ( 'NONE', #42618 ) ;
#36144 = VECTOR ( 'NONE', #21626, 1000.000000000000000 ) ;
#36146 = VERTEX_POINT ( 'NONE', #6633 ) ;
#36145 = VECTOR ( 'NONE', #15794, 1000.000000000000000 ) ;
#36147 = CARTESIAN_POINT ( 'NONE',  ( -144.2430459457361280, -193.5000000000000000, 78.77358243914957825 ) ) ;
#36148 = LINE ( 'NONE', #16451, #5034 ) ;
#36149 = PLANE ( 'NONE',  #27616 ) ;
#36150 = FACE_BOUND ( 'NONE', #2469, .T. ) ;
#36151 = DIRECTION ( 'NONE',  ( 0.000000000000000000, 0.000000000000000000, -1.000000000000000000 ) ) ;
#36152 = ORIENTED_EDGE ( 'NONE', *, *, #1884, .F. ) ;
#36153 = EDGE_CURVE ( 'NONE', #3854, #1503, #30179, .T. ) ;
#36154 = EDGE_CURVE ( 'NONE', #50970, #12506, #18708, .T. ) ;
#36155 = DIRECTION ( 'NONE',  ( 0.9995608365087946812, 0.000000000000000000, -0.02963332782254913048 ) ) ;
#36156 = ORIENTED_EDGE ( 'NONE', *, *, #47006, .T. ) ;
#36158 = VERTEX_POINT ( 'NONE', #34990 ) ;
#36157 = PLANE ( 'NONE',  #45798 ) ;
#36159 = ORIENTED_EDGE ( 'NONE', *, *, #11834, .T. ) ;
#36160 = EDGE_CURVE ( 'NONE', #41614, #35813, #34377, .T. ) ;
#36161 = CIRCLE ( 'NONE', #30277, 125.0000000000000000 ) ;
#36162 = CYLINDRICAL_SURFACE ( 'NONE', #50968, 4.999999999999997335 ) ;
#36163 = CARTESIAN_POINT ( 'NONE',  ( 0.000000000000000000, -144.4216883355098844, -55.16595831843940090 ) ) ;
#36164 = LINE ( 'NONE', #27508, #49003 ) ;
#36165 = DIRECTION ( 'NONE',  ( 0.000000000000000000, 0.000000000000000000, 1.000000000000000000 ) ) ;
#36166 = EDGE_LOOP ( 'NONE', ( #35762, #37078, #39822, #47878 ) ) ;
#36167 = CARTESIAN_POINT ( 'NONE',  ( -149.1282321233094876, -189.7472609257535510, -72.42760398749013007 ) ) ;
#36168 = ORIENTED_EDGE ( 'NONE', *, *, #35411, .F. ) ;
#36169 = ORIENTED_EDGE ( 'NONE', *, *, #22462, .F. ) ;
#36170 = DIRECTION ( 'NONE',  ( 0.8124868780056825335, 0.000000000000000000, -0.5829794791144703447 ) ) ;
#36171 = DIRECTION ( 'NONE',  ( -0.000000000000000000, 1.000000000000000000, -0.000000000000000000 ) ) ;
#36172 = DIRECTION ( 'NONE',  ( 0.000000000000000000, 0.000000000000000000, -1.000000000000000000 ) ) ;
#36173 = CIRCLE ( 'NONE', #32803, 125.0000000000000000 ) ;
#36174 = CARTESIAN_POINT ( 'NONE',  ( -48.47912675150885065, -175.3837268820161057, 6.938893903907228378E-15 ) ) ;
#36175 = LINE ( 'NONE', #32232, #19501 ) ;
#36176 = ORIENTED_EDGE ( 'NONE', *, *, #1927, .T. ) ;
#36177 = PLANE ( 'NONE',  #13753 ) ;
#36178 = DIRECTION ( 'NONE',  ( -0.000000000000000000, 1.000000000000000000, 0.000000000000000000 ) ) ;
#36179 = CIRCLE ( 'NONE', #37045, 125.0000000000000000 ) ;
#36180 = FACE_BOUND ( 'NONE', #22644, .T. ) ;
#36181 = ORIENTED_EDGE ( 'NONE', *, *, #10472, .T. ) ;
#36182 = LINE ( 'NONE', #8077, #23943 ) ;
#36183 = CARTESIAN_POINT ( 'NONE',  ( -48.47912675150885065, -189.7472609257535510, 6.938893903907228378E-15 ) ) ;
#36184 = CARTESIAN_POINT ( 'NONE',  ( 60.58466639580034041, -193.5000000000000000, -61.07445476073405644 ) ) ;
#36185 = EDGE_LOOP ( 'NONE', ( #31735, #46204, #26538, #11011 ) ) ;
#36186 = DIRECTION ( 'NONE',  ( 0.4827922027307490205, 0.000000000000000000, -0.8757349421956345248 ) ) ;
#36187 = VECTOR ( 'NONE', #51112, 1000.000000000000000 ) ;
#36188 = CYLINDRICAL_SURFACE ( 'NONE', #13342, 125.0000000000000000 ) ;
#36190 = EDGE_LOOP ( 'NONE', ( #23935, #13855, #50737, #4165, #48391 ) ) ;
#36189 = LINE ( 'NONE', #24626, #48926 ) ;
#36191 = ADVANCED_FACE ( 'NONE', ( #50771 ), #31296, .F. ) ;
#36192 = EDGE_CURVE ( 'NONE', #755, #40102, #2494, .T. ) ;
#36193 = ADVANCED_FACE ( 'NONE', ( #46833 ), #10820, .F. ) ;
#36194 = DIRECTION ( 'NONE',  ( 0.000000000000000000, 0.5680647467311596976, 0.8229838658936536877 ) ) ;
#36195 = EDGE_LOOP ( 'NONE', ( #10024, #40238, #42789, #16056 ) ) ;
#36196 = EDGE_CURVE ( 'NONE', #51929, #39115, #38575, .T. ) ;
#36197 = EDGE_LOOP ( 'NONE', ( #35169, #9863, #6201, #41112 ) ) ;
#36198 = CARTESIAN_POINT ( 'NONE',  ( -112.1919339979530150, -193.5000000000000000, 107.5438431188761683 ) ) ;
#36199 = ORIENTED_EDGE ( 'NONE', *, *, #26364, .T. ) ;
#36200 = EDGE_CURVE ( 'NONE', #26846, #17445, #43403, .T. ) ;
#36201 = PLANE ( 'NONE',  #11640 ) ;
#36202 = EDGE_CURVE ( 'NONE', #9658, #8712, #43597, .T. ) ;
#36203 = DIRECTION ( 'NONE',  ( -1.000000000000000000, 0.000000000000000000, 0.000000000000000000 ) ) ;
#36204 = CIRCLE ( 'NONE', #15254, 125.0000000000000000 ) ;
#36205 = ADVANCED_FACE ( 'NONE', ( #34469 ), #46572, .T. ) ;
#36206 = VECTOR ( 'NONE', #9619, 1000.000000000000000 ) ;
#36207 = ADVANCED_FACE ( 'NONE', ( #15538 ), #31553, .T. ) ;
#36208 = VECTOR ( 'NONE', #1359, 1000.000000000000000 ) ;
#36209 = PLANE ( 'NONE',  #34297 ) ;
#36210 = LINE ( 'NONE', #206, #11348 ) ;
#36211 = EDGE_LOOP ( 'NONE', ( #11465, #14142, #4196, #7493 ) ) ;
#36214 = VERTEX_POINT ( 'NONE', #47863 ) ;
#36213 = CARTESIAN_POINT ( 'NONE',  ( 50.08808042611238420, -177.1207230881787780, -76.87330921200083367 ) ) ;
#36212 = DIRECTION ( 'NONE',  ( 0.000000000000000000, -1.000000000000000000, 0.000000000000000000 ) ) ;
#36215 = ORIENTED_EDGE ( 'NONE', *, *, #29162, .F. ) ;
#36216 = ADVANCED_FACE ( 'NONE', ( #3970 ), #12359, .T. ) ;
#36217 = LINE ( 'NONE', #25187, #8059 ) ;
#36218 = ORIENTED_EDGE ( 'NONE', *, *, #21985, .F. ) ;
#36219 = DIRECTION ( 'NONE',  ( -0.2059786187410953262, 0.000000000000000000, -0.9785564922995046988 ) ) ;
#36220 = ORIENTED_EDGE ( 'NONE', *, *, #6812, .T. ) ;
#36221 = ADVANCED_FACE ( 'NONE', ( #16588 ), #36271, .F. ) ;
#36222 = LINE ( 'NONE', #9167, #49423 ) ;
#36223 = ORIENTED_EDGE ( 'NONE', *, *, #44298, .T. ) ;
#36225 = DIRECTION ( 'NONE',  ( -0.000000000000000000, 1.000000000000000000, -0.000000000000000000 ) ) ;
#36224 = LINE ( 'NONE', #23618, #14041 ) ;
#36226 = ORIENTED_EDGE ( 'NONE', *, *, #29400, .F. ) ;
#36227 = AXIS2_PLACEMENT_3D ( 'NONE', #4019, #37097, #39990 ) ;
#36228 = ORIENTED_EDGE ( 'NONE', *, *, #51954, .T. ) ;
#36229 = DIRECTION ( 'NONE',  ( -0.000000000000000000, -0.9927088740980530845, 0.1205366802553303057 ) ) ;
#36231 = VECTOR ( 'NONE', #23428, 1000.000000000000000 ) ;
#36230 = FACE_OUTER_BOUND ( 'NONE', #27998, .T. ) ;
#36232 = DIRECTION ( 'NONE',  ( -0.000000000000000000, 1.000000000000000000, -0.000000000000000000 ) ) ;
#36233 = CARTESIAN_POINT ( 'NONE',  ( -336.3521761649654422, -120.8677111499054320, 59.00000000000000000 ) ) ;
#36234 = DIRECTION ( 'NONE',  ( 0.000000000000000000, -1.000000000000000000, 0.000000000000000000 ) ) ;
#36235 = CARTESIAN_POINT ( 'NONE',  ( -159.5526844214375615, -177.1207230881787780, 57.33816169485226055 ) ) ;
#36236 = ORIENTED_EDGE ( 'NONE', *, *, #11875, .T. ) ;
#36237 = SHAPE_DEFINITION_REPRESENTATION ( #6300, #2890 ) ;
#36238 = DIRECTION ( 'NONE',  ( 0.000000000000000000, 0.8660254037844354880, -0.5000000000000054401 ) ) ;
#36239 = EDGE_CURVE ( 'NONE', #47580, #28774, #24201, .T. ) ;
#36240 = LINE ( 'NONE', #24175, #46651 ) ;
#36241 = PLANE ( 'NONE',  #40524 ) ;
#36242 = ORIENTED_EDGE ( 'NONE', *, *, #22462, .T. ) ;
#36243 = LINE ( 'NONE', #20474, #4708 ) ;
#36244 = AXIS2_PLACEMENT_3D ( 'NONE', #19740, #27640, #8437 ) ;
#36245 = CARTESIAN_POINT ( 'NONE',  ( -14.52059121095390992, -183.6283474603465606, 119.2602935412682399 ) ) ;
#36246 = DIRECTION ( 'NONE',  ( 0.000000000000000000, -0.8854560256532044704, 0.4647231720437789981 ) ) ;
#36247 = ORIENTED_EDGE ( 'NONE', *, *, #48285, .F. ) ;
#36248 = EDGE_LOOP ( 'NONE', ( #13542, #33893, #21743, #48278 ) ) ;
#36249 = CIRCLE ( 'NONE', #49703, 125.0000000000000000 ) ;
#36250 = ORIENTED_EDGE ( 'NONE', *, *, #5959, .F. ) ;
#36251 = AXIS2_PLACEMENT_3D ( 'NONE', #17854, #9982, #5792 ) ;
#36252 = EDGE_CURVE ( 'NONE', #26962, #20303, #48114, .T. ) ;
#36253 = PLANE ( 'NONE',  #44399 ) ;
#36254 = CARTESIAN_POINT ( 'NONE',  ( 71.35177504360963496, -175.3837268820161057, 31.88354567335082024 ) ) ;
#36255 = CARTESIAN_POINT ( 'NONE',  ( -112.1919339979530150, -175.3837268820161057, 107.5438431188761683 ) ) ;
#36256 = ORIENTED_EDGE ( 'NONE', *, *, #34076, .T. ) ;
#36257 = EDGE_CURVE ( 'NONE', #32445, #37251, #1556, .T. ) ;
#36258 = EDGE_CURVE ( 'NONE', #4155, #32314, #43898, .T. ) ;
#36259 = EDGE_CURVE ( 'NONE', #51089, #46182, #4227, .T. ) ;
#36260 = FACE_OUTER_BOUND ( 'NONE', #1165, .T. ) ;
#36261 = CIRCLE ( 'NONE', #32097, 4.999999999999997335 ) ;
#36262 = ORIENTED_EDGE ( 'NONE', *, *, #46422, .T. ) ;
#36263 = EDGE_CURVE ( 'NONE', #8885, #50347, #4488, .T. ) ;
#36264 = ORIENTED_EDGE ( 'NONE', *, *, #19516, .F. ) ;
#36265 = VECTOR ( 'NONE', #21617, 1000.000000000000000 ) ;
#36266 = AXIS2_PLACEMENT_3D ( 'NONE', #10113, #29559, #25617 ) ;
#36267 = ORIENTED_EDGE ( 'NONE', *, *, #19334, .T. ) ;
#36268 = CARTESIAN_POINT ( 'NONE',  ( -164.2529447963538871, -193.5000000000000000, 44.41421852208715393 ) ) ;
#36269 = EDGE_CURVE ( 'NONE', #26701, #34028, #47702, .T. ) ;
#36270 = EDGE_LOOP ( 'NONE', ( #45682, #21736, #26496, #42392 ) ) ;
#36271 = PLANE ( 'NONE',  #40140 ) ;
#36272 = PLANE ( 'NONE',  #18522 ) ;
#36275 = ORIENTED_EDGE ( 'NONE', *, *, #16236, .F. ) ;
#36274 = DIRECTION ( 'NONE',  ( 0.000000000000000000, -1.000000000000000000, 0.000000000000000000 ) ) ;
#36273 = DIRECTION ( 'NONE',  ( -0.000000000000000000, 0.2393156642875547968, -0.9709418174260527890 ) ) ;
#36276 = EDGE_CURVE ( 'NONE', #17499, #40613, #7645, .T. ) ;
#36277 = PLANE ( 'NONE',  #39877 ) ;
#36278 = EDGE_LOOP ( 'NONE', ( #8320, #15862 ) ) ;
#36279 = CARTESIAN_POINT ( 'NONE',  ( -5.732832253866452454, -189.7472609257535510, -117.4638425504666799 ) ) ;
#36280 = VECTOR ( 'NONE', #43352, 1000.000000000000000 ) ;
#36281 = VERTEX_POINT ( 'NONE', #7895 ) ;
#36282 = EDGE_CURVE ( 'NONE', #21757, #6199, #15928, .T. ) ;
#36283 = CARTESIAN_POINT ( 'NONE',  ( -336.3521761649654422, -67.75522407825191351, 19.39547174791671935 ) ) ;
#36284 = CARTESIAN_POINT ( 'NONE',  ( 69.99104047056317768, -175.3837268820161057, -39.87254040532513244 ) ) ;
#36286 = CARTESIAN_POINT ( 'NONE',  ( -260.0000000000000000, -123.5000000000000284, 20.00000000000002487 ) ) ;
#36285 = DIRECTION ( 'NONE',  ( 0.000000000000000000, -0.000000000000000000, -1.000000000000000000 ) ) ;
#36287 = ORIENTED_EDGE ( 'NONE', *, *, #27452, .F. ) ;
#36288 = EDGE_CURVE ( 'NONE', #50756, #19096, #48647, .T. ) ;
#36289 = AXIS2_PLACEMENT_3D ( 'NONE', #32054, #48359, #8152 ) ;
#36290 = LINE ( 'NONE', #12102, #28148 ) ;
#36291 = DIRECTION ( 'NONE',  ( -0.000000000000000000, 1.000000000000000000, -0.000000000000000000 ) ) ;
#36292 =( LENGTH_UNIT ( ) NAMED_UNIT ( * ) SI_UNIT ( .MILLI., .METRE. ) );
#36293 = ORIENTED_EDGE ( 'NONE', *, *, #6800, .T. ) ;
#36294 = PLANE ( 'NONE',  #25806 ) ;
#36295 = FACE_OUTER_BOUND ( 'NONE', #10675, .T. ) ;
#36296 = DIRECTION ( 'NONE',  ( 0.000000000000000000, -1.000000000000000000, -0.000000000000000000 ) ) ;
#36297 = VERTEX_POINT ( 'NONE', #8421 ) ;
#36298 = CARTESIAN_POINT ( 'NONE',  ( -336.3521761649654422, -181.0704707379907745, 16.90091414705587525 ) ) ;
#36299 = CIRCLE ( 'NONE', #29588, 125.0000000000000000 ) ;
#36301 = VECTOR ( 'NONE', #35577, 1000.000000000000227 ) ;
#36300 = FACE_OUTER_BOUND ( 'NONE', #42999, .T. ) ;
#36302 = ADVANCED_FACE ( 'NONE', ( #24448 ), #19720, .F. ) ;
#36303 = VERTEX_POINT ( 'NONE', #3436 ) ;
#36304 = DIRECTION ( 'NONE',  ( 0.000000000000000000, 0.000000000000000000, -1.000000000000000000 ) ) ;
#36305 = ORIENTED_EDGE ( 'NONE', *, *, #22522, .T. ) ;
#36306 = VECTOR ( 'NONE', #5771, 1000.000000000000000 ) ;
#36307 = VECTOR ( 'NONE', #11816, 1000.000000000000000 ) ;
#36308 = CARTESIAN_POINT ( 'NONE',  ( -330.4913330509368166, -182.1300919119129560, -6.615309698014691264 ) ) ;
#36309 = CARTESIAN_POINT ( 'NONE',  ( -336.3521761649654422, -65.92952926200918284, -16.90091414705545247 ) ) ;
#36310 = DIRECTION ( 'NONE',  ( 0.9842305779475980509, 0.000000000000000000, -0.1768902751225666647 ) ) ;
#36311 = DIRECTION ( 'NONE',  ( 0.000000000000000000, 0.8229838658936536877, -0.5680647467311596976 ) ) ;
#36312 = DIRECTION ( 'NONE',  ( -0.000000000000000000, 1.000000000000000000, -0.000000000000000000 ) ) ;
#36313 = VECTOR ( 'NONE', #13124, 1000.000000000000000 ) ;
#36314 = DIRECTION ( 'NONE',  ( -0.000000000000000000, 1.000000000000000000, 0.000000000000000000 ) ) ;
#36315 = DIRECTION ( 'NONE',  ( 0.000000000000000000, -0.000000000000000000, -1.000000000000000000 ) ) ;
#36316 = CARTESIAN_POINT ( 'NONE',  ( -305.0000000000000568, -118.8878589706978914, -59.82247199109903590 ) ) ;
#36318 = ORIENTED_EDGE ( 'NONE', *, *, #51160, .T. ) ;
#36317 = DIRECTION ( 'NONE',  ( -1.000000000000000000, -0.000000000000000000, 0.000000000000000000 ) ) ;
#36319 = MANIFOLD_SOLID_BREP ( 'Boss-Extrude10', #32112 ) ;
#36320 = VECTOR ( 'NONE', #10386, 1000.000000000000114 ) ;
#36321 = ORIENTED_EDGE ( 'NONE', *, *, #48139, .T. ) ;
#36322 = ADVANCED_FACE ( 'NONE', ( #25491 ), #28639, .T. ) ;
#36323 = ADVANCED_FACE ( 'NONE', ( #45476 ), #36805, .F. ) ;
#36324 = CARTESIAN_POINT ( 'NONE',  ( -330.0000000000000568, -123.5000000000000284, -31.65769145387501027 ) ) ;
#36325 = AXIS2_PLACEMENT_3D ( 'NONE', #35812, #15861, #19517 ) ;
#36326 = CARTESIAN_POINT ( 'NONE',  ( -91.84482189527193441, -193.5000000000000000, -117.2365833888816695 ) ) ;
#36327 = ORIENTED_EDGE ( 'NONE', *, *, #30508, .T. ) ;
#36328 = ORIENTED_EDGE ( 'NONE', *, *, #49284, .F. ) ;
#36329 = EDGE_LOOP ( 'NONE', ( #3340, #26201, #3700, #4375 ) ) ;
#36330 = CARTESIAN_POINT ( 'NONE',  ( -112.2501518587238962, -189.7472609257535510, -106.3450133598699807 ) ) ;
#36331 = DIRECTION ( 'NONE',  ( 0.000000000000000000, 0.2393156642875685636, 0.9709418174260492362 ) ) ;
#36332 = CARTESIAN_POINT ( 'NONE',  ( -48.59739992243020623, -189.7472609257535510, -0.9929810960135115883 ) ) ;
#36334 = ORIENTED_EDGE ( 'NONE', *, *, #45210, .T. ) ;
#36333 = VECTOR ( 'NONE', #50742, 1000.000000000000000 ) ;
#36335 = VECTOR ( 'NONE', #41434, 1000.000000000000000 ) ;
#36336 = VERTEX_POINT ( 'NONE', #33111 ) ;
#36337 = ORIENTED_EDGE ( 'NONE', *, *, #49078, .T. ) ;
#36338 = CARTESIAN_POINT ( 'NONE',  ( -6.938893903907228378E-15, -63.50000000000000000, 0.000000000000000000 ) ) ;
#36339 = LINE ( 'NONE', #333, #42824 ) ;
#36341 = ORIENTED_EDGE ( 'NONE', *, *, #41916, .F. ) ;
#36340 = CARTESIAN_POINT ( 'NONE',  ( 30.00000000000000711, -43.50000000000000000, 0.000000000000000000 ) ) ;
#36342 = AXIS2_PLACEMENT_3D ( 'NONE', #37268, #41201, #33335 ) ;
#36343 = EDGE_CURVE ( 'NONE', #48288, #49251, #801, .T. ) ;
#36344 = LINE ( 'NONE', #12430, #32889 ) ;
#36345 = CARTESIAN_POINT ( 'NONE',  ( -140.5933766095837427, -175.3837268820161057, -84.49831343337066869 ) ) ;
#36346 = ORIENTED_EDGE ( 'NONE', *, *, #41565, .F. ) ;
#36347 = CARTESIAN_POINT ( 'NONE',  ( 46.81796867211178181, 28.00000000000000355, -47.30331996785741211 ) ) ;
#36348 = VECTOR ( 'NONE', #22513, 1000.000000000000000 ) ;
#36349 = CARTESIAN_POINT ( 'NONE',  ( -154.2693405752510500, -193.5000000000000000, 66.58401203837830451 ) ) ;
#36350 = DIRECTION ( 'NONE',  ( 0.000000000000000000, 0.000000000000000000, 1.000000000000000000 ) ) ;
#36351 = CARTESIAN_POINT ( 'NONE',  ( -138.3664773286545824, -183.6283474603465606, -85.41934182508016704 ) ) ;
#36352 = EDGE_CURVE ( 'NONE', #37026, #31066, #1313, .T. ) ;
#36353 = VERTEX_POINT ( 'NONE', #37590 ) ;
#36354 = VERTEX_POINT ( 'NONE', #21820 ) ;
#36355 = ORIENTED_EDGE ( 'NONE', *, *, #32057, .T. ) ;
#36356 = DIRECTION ( 'NONE',  ( 0.000000000000000000, 1.000000000000000000, 0.000000000000000000 ) ) ;
#36357 = CARTESIAN_POINT ( 'NONE',  ( -305.0000000000000568, -108.6560878169898956, 58.13482838284708976 ) ) ;
#36358 = ORIENTED_EDGE ( 'NONE', *, *, #44666, .T. ) ;
#36359 = FACE_OUTER_BOUND ( 'NONE', #7855, .T. ) ;
#36360 = VECTOR ( 'NONE', #18422, 1000.000000000000000 ) ;
#36361 = FACE_OUTER_BOUND ( 'NONE', #35720, .T. ) ;
#36362 = ORIENTED_EDGE ( 'NONE', *, *, #29996, .T. ) ;
#36363 = CARTESIAN_POINT ( 'NONE',  ( -49.17567778057184569, -183.6283474603465606, -0.7175072570443327136 ) ) ;
#36364 = AXIS2_PLACEMENT_3D ( 'NONE', #49486, #25807, #12925 ) ;
#36365 = ORIENTED_EDGE ( 'NONE', *, *, #32659, .F. ) ;
#36366 = CARTESIAN_POINT ( 'NONE',  ( -48.64924157374595381, -175.3837268820161057, 123.9998842437354227 ) ) ;
#36367 = ORIENTED_EDGE ( 'NONE', *, *, #9704, .T. ) ;
#36368 = FACE_BOUND ( 'NONE', #14615, .T. ) ;
#36369 = FACE_OUTER_BOUND ( 'NONE', #36429, .T. ) ;
#36370 = ORIENTED_EDGE ( 'NONE', *, *, #852, .T. ) ;
#36371 = CARTESIAN_POINT ( 'NONE',  ( 50.88012955800437709, -183.6283474603465606, 74.18852968774250201 ) ) ;
#36372 = CARTESIAN_POINT ( 'NONE',  ( 1.459872500689274649E-15, 91.20387711827495991, -106.5147620531948007 ) ) ;
#36373 = PLANE ( 'NONE',  #1399 ) ;
#36374 = AXIS2_PLACEMENT_3D ( 'NONE', #5600, #2665, #49735 ) ;
#36375 = CARTESIAN_POINT ( 'NONE',  ( -332.3517673607765914, -65.24746378767824240, -9.724760635741734660 ) ) ;
#36376 = ORIENTED_EDGE ( 'NONE', *, *, #41980, .T. ) ;
#36377 = CARTESIAN_POINT ( 'NONE',  ( -339.1964088526558498, -130.1153096980144426, 58.63009191191295599 ) ) ;
#36378 = ORIENTED_EDGE ( 'NONE', *, *, #21509, .T. ) ;
#36379 = ORIENTED_EDGE ( 'NONE', *, *, #45856, .F. ) ;
#36380 = AXIS2_PLACEMENT_3D ( 'NONE', #45369, #20392, #13298 ) ;
#36381 = CARTESIAN_POINT ( 'NONE',  ( 73.50869128264331209, -177.1207230881787780, -22.25084316132035056 ) ) ;
#36383 = ORIENTED_EDGE ( 'NONE', *, *, #42322, .T. ) ;
#36382 = LINE ( 'NONE', #32185, #12699 ) ;
#36384 = VERTEX_POINT ( 'NONE', #16846 ) ;
#36385 = CARTESIAN_POINT ( 'NONE',  ( 36.10886851198521441, -193.5000000000000000, 92.03190238880813467 ) ) ;
#36386 = ADVANCED_FACE ( 'NONE', ( #1830 ), #49160, .F. ) ;
#36387 = DIRECTION ( 'NONE',  ( -1.000000000000000000, -0.000000000000000000, 0.000000000000000000 ) ) ;
#36388 = ORIENTED_EDGE ( 'NONE', *, *, #14346, .T. ) ;
#36389 = LINE ( 'NONE', #40319, #7967 ) ;
#36390 = ORIENTED_EDGE ( 'NONE', *, *, #10517, .T. ) ;
#36391 = LINE ( 'NONE', #43517, #26659 ) ;
#36392 = DIRECTION ( 'NONE',  ( -0.000000000000000000, 1.000000000000000000, -0.000000000000000000 ) ) ;
#36393 = AXIS2_PLACEMENT_3D ( 'NONE', #5506, #9185, #17076 ) ;
#36394 = CARTESIAN_POINT ( 'NONE',  ( -339.1964088526558498, -156.6043281241909426, 48.84008046109164525 ) ) ;
#36395 = CARTESIAN_POINT ( 'NONE',  ( -339.1964088526558498, -151.3613951634084742, 52.00954392751779665 ) ) ;
#36396 = ORIENTED_EDGE ( 'NONE', *, *, #25292, .F. ) ;
#36397 = VERTEX_POINT ( 'NONE', #13409 ) ;
#36398 = VECTOR ( 'NONE', #14415, 1000.000000000000000 ) ;
#36399 = ORIENTED_EDGE ( 'NONE', *, *, #9184, .F. ) ;
#36400 = CARTESIAN_POINT ( 'NONE',  ( -49.47868758801764955, -193.5000000000000000, -0.02963332782256313663 ) ) ;
#36401 = DIRECTION ( 'NONE',  ( -0.000000000000000000, 1.000000000000000000, -0.000000000000000000 ) ) ;
#36402 = EDGE_CURVE ( 'NONE', #7460, #5112, #13927, .T. ) ;
#36403 = FACE_OUTER_BOUND ( 'NONE', #33973, .T. ) ;
#36404 = FACE_BOUND ( 'NONE', #24962, .T. ) ;
#36405 = CARTESIAN_POINT ( 'NONE',  ( -336.3521761649654422, -98.41210887299327226, -53.46519113769058151 ) ) ;
#36406 = ORIENTED_EDGE ( 'NONE', *, *, #25497, .T. ) ;
#36407 = VECTOR ( 'NONE', #49866, 1000.000000000000000 ) ;
#36408 = ORIENTED_EDGE ( 'NONE', *, *, #568, .T. ) ;
#36410 = EDGE_LOOP ( 'NONE', ( #14391, #48179, #19927, #33895 ) ) ;
#36409 = CARTESIAN_POINT ( 'NONE',  ( 47.28479244271901649, -193.5000000000000000, -78.77358243914883928 ) ) ;
#36411 = ORIENTED_EDGE ( 'NONE', *, *, #15645, .F. ) ;
#36412 = FACE_OUTER_BOUND ( 'NONE', #15837, .T. ) ;
#36413 = DIRECTION ( 'NONE',  ( 0.000000000000000000, 0.000000000000000000, 1.000000000000000000 ) ) ;
#36414 = CARTESIAN_POINT ( 'NONE',  ( -77.77032474405882567, -175.3837268820161057, 120.4907712303052989 ) ) ;
#36415 = CARTESIAN_POINT ( 'NONE',  ( -305.0000000000000568, -84.08827740916102300, -45.24064679492050089 ) ) ;
#36416 = VERTEX_POINT ( 'NONE', #48902 ) ;
#36417 = CARTESIAN_POINT ( 'NONE',  ( 18.00181100848372040, -183.6283474603465606, -105.8550183720733742 ) ) ;
#36418 = VERTEX_POINT ( 'NONE', #46007 ) ;
#36419 = ORIENTED_EDGE ( 'NONE', *, *, #18012, .T. ) ;
#36420 = CARTESIAN_POINT ( 'NONE',  ( 62.13187335169531877, -177.1207230881787780, -58.22548115875871844 ) ) ;
#36421 = DIRECTION ( 'NONE',  ( -0.9995608365087946812, 0.000000000000000000, 0.02963332782254913048 ) ) ;
#36422 = CARTESIAN_POINT ( 'NONE',  ( -99.02518858244150124, -193.5000000000000000, 114.3245189510261497 ) ) ;
#36423 = CIRCLE ( 'NONE', #42323, 125.0000000000000000 ) ;
#36424 = CARTESIAN_POINT ( 'NONE',  ( -48.47912675150885065, -177.1207230881787780, 6.938893903907228378E-15 ) ) ;
#36425 = VECTOR ( 'NONE', #33594, 1000.000000000000000 ) ;
#36426 = EDGE_CURVE ( 'NONE', #3068, #27986, #691, .T. ) ;
#36427 = DIRECTION ( 'NONE',  ( 0.000000000000000000, -1.000000000000000000, -0.000000000000000000 ) ) ;
#36428 = DIRECTION ( 'NONE',  ( 0.000000000000000000, 1.000000000000000000, 0.000000000000000000 ) ) ;
#36429 = EDGE_LOOP ( 'NONE', ( #26971, #31690, #33609, #30330 ) ) ;
#36430 = DIRECTION ( 'NONE',  ( -1.000000000000000000, 0.000000000000000000, 0.000000000000000000 ) ) ;
#36431 = CARTESIAN_POINT ( 'NONE',  ( -18.95304271317703382, -193.5000000000000000, -121.4627941443854837 ) ) ;
#36432 = CIRCLE ( 'NONE', #7047, 60.00000000000000000 ) ;
#36433 = EDGE_CURVE ( 'NONE', #1427, #30234, #17106, .T. ) ;
#36434 = CARTESIAN_POINT ( 'NONE',  ( 41.41233698655026529, -193.5000000000000000, 86.85922373029363541 ) ) ;
#36435 = FACE_BOUND ( 'NONE', #3255, .T. ) ;
#36436 = ORIENTED_EDGE ( 'NONE', *, *, #47218, .T. ) ;
#36437 = DIRECTION ( 'NONE',  ( 0.000000000000000000, 0.000000000000000000, -1.000000000000000000 ) ) ;
#36438 = CARTESIAN_POINT ( 'NONE',  ( 74.31448861501728231, -183.6283474603465606, -23.38221600314289361 ) ) ;
#36439 = ORIENTED_EDGE ( 'NONE', *, *, #24708, .T. ) ;
#36440 = DIRECTION ( 'NONE',  ( -0.8610436117673548884, 0.000000000000000000, -0.5085311186492216251 ) ) ;
#36441 = EDGE_CURVE ( 'NONE', #32906, #32186, #9469, .T. ) ;
#36442 = CIRCLE ( 'NONE', #38130, 124.9999999999999858 ) ;
#36443 = ORIENTED_EDGE ( 'NONE', *, *, #41068, .F. ) ;
#36444 = ADVANCED_FACE ( 'NONE', ( #9994 ), #37054, .T. ) ;
#36445 = DIRECTION ( 'NONE',  ( 0.000000000000000000, 0.8854560256532110207, 0.4647231720437664526 ) ) ;
#36446 = EDGE_CURVE ( 'NONE', #37128, #10115, #35949, .T. ) ;
#36447 = FACE_BOUND ( 'NONE', #30229, .T. ) ;
#36449 = EDGE_LOOP ( 'NONE', ( #7090, #43557, #4744, #45304 ) ) ;
#36448 = DIRECTION ( 'NONE',  ( 0.000000000000000000, -1.000000000000000000, 0.000000000000000000 ) ) ;
#36450 = LINE ( 'NONE', #20171, #7580 ) ;
#36451 = VERTEX_POINT ( 'NONE', #20776 ) ;
#36452 = ORIENTED_EDGE ( 'NONE', *, *, #3815, .F. ) ;
#36453 = CARTESIAN_POINT ( 'NONE',  ( -336.3521761649654422, -104.7054247829104412, -56.98038208374145341 ) ) ;
#36454 = EDGE_LOOP ( 'NONE', ( #46122, #44464, #50983, #35701 ) ) ;
#36455 = EDGE_CURVE ( 'NONE', #35554, #1331, #29175, .T. ) ;
#36456 = CARTESIAN_POINT ( 'NONE',  ( -336.3521761649654422, -139.2044816956407089, -56.89493493766761389 ) ) ;
#36457 = VECTOR ( 'NONE', #35500, 1000.000000000000000 ) ;
#36458 = DIRECTION ( 'NONE',  ( 0.000000000000000000, 0.000000000000000000, -1.000000000000000000 ) ) ;
#36459 = VECTOR ( 'NONE', #40683, 1000.000000000000114 ) ;
#36460 = AXIS2_PLACEMENT_3D ( 'NONE', #27455, #3800, #47953 ) ;
#36461 = CYLINDRICAL_SURFACE ( 'NONE', #44072, 125.0000000000000000 ) ;
#36462 = ORIENTED_EDGE ( 'NONE', *, *, #41329, .F. ) ;
#36465 = ORIENTED_EDGE ( 'NONE', *, *, #41443, .T. ) ;
#36464 = DIRECTION ( 'NONE',  ( 1.000000000000000000, 0.000000000000000000, 0.000000000000000000 ) ) ;
#36463 = DIRECTION ( 'NONE',  ( 1.000000000000000000, 0.000000000000000000, 0.000000000000000000 ) ) ;
#36466 = ORIENTED_EDGE ( 'NONE', *, *, #6643, .T. ) ;
#36467 = VECTOR ( 'NONE', #51747, 1000.000000000000114 ) ;
#36468 = FACE_OUTER_BOUND ( 'NONE', #44545, .T. ) ;
#36469 = ORIENTED_EDGE ( 'NONE', *, *, #19193, .F. ) ;
#36470 = PLANE ( 'NONE',  #37371 ) ;
#36471 = ORIENTED_EDGE ( 'NONE', *, *, #23861, .F. ) ;
#36472 = PLANE ( 'NONE',  #49797 ) ;
#36473 = LINE ( 'NONE', #12574, #14154 ) ;
#36474 = ORIENTED_EDGE ( 'NONE', *, *, #11504, .T. ) ;
#36476 = CARTESIAN_POINT ( 'NONE',  ( -145.0195698084541505, -189.7472609257535510, 79.40367028273126948 ) ) ;
#36475 = DIRECTION ( 'NONE',  ( 0.000000000000000000, 0.000000000000000000, 1.000000000000000000 ) ) ;
#36477 = VECTOR ( 'NONE', #33951, 1000.000000000000000 ) ;
#36478 = EDGE_LOOP ( 'NONE', ( #30046, #20018, #14543, #19719, #35199 ) ) ;
#36479 = EDGE_LOOP ( 'NONE', ( #38176, #10846, #5516, #3106 ) ) ;
#36480 = DIRECTION ( 'NONE',  ( 0.000000000000000000, 0.000000000000000000, 1.000000000000000000 ) ) ;
#36481 = DIRECTION ( 'NONE',  ( -1.000000000000000000, 0.000000000000000000, 0.000000000000000000 ) ) ;
#36482 = CARTESIAN_POINT ( 'NONE',  ( -47.97059563285962724, -183.6283474603465606, -0.8610436117673480050 ) ) ;
#36483 = CARTESIAN_POINT ( 'NONE',  ( 30.00000000000000711, 0.000000000000000000, 30.00000000000000355 ) ) ;
#36484 = CARTESIAN_POINT ( 'NONE',  ( -305.0000000000000568, -123.5000000000000284, 20.00000000000000355 ) ) ;
#36485 = DIRECTION ( 'NONE',  ( -0.000000000000000000, 1.000000000000000000, -0.000000000000000000 ) ) ;
#36486 = EDGE_CURVE ( 'NONE', #27201, #20876, #7521, .T. ) ;
#36487 = EDGE_CURVE ( 'NONE', #21200, #38380, #42807, .T. ) ;
#36488 = SHAPE_DEFINITION_REPRESENTATION ( #30626, #11639 ) ;
#36489 = PLANE ( 'NONE',  #41291 ) ;
#36490 = LINE ( 'NONE', #45977, #9549 ) ;
#36491 = DIRECTION ( 'NONE',  ( 0.2920567706369628924, 0.000000000000000000, 0.9564009842765264224 ) ) ;
#36492 = DIRECTION ( 'NONE',  ( 0.000000000000000000, -0.000000000000000000, -1.000000000000000000 ) ) ;
#36493 = ORIENTED_EDGE ( 'NONE', *, *, #11898, .T. ) ;
#36494 = ORIENTED_EDGE ( 'NONE', *, *, #42927, .F. ) ;
#36495 = VECTOR ( 'NONE', #5628, 1000.000000000000114 ) ;
#36496 = CARTESIAN_POINT ( 'NONE',  ( 35.67816836544800907, -177.1207230881787780, -92.42591454022745268 ) ) ;
#36497 = EDGE_CURVE ( 'NONE', #7901, #18571, #14972, .T. ) ;
#36498 = VECTOR ( 'NONE', #7483, 1000.000000000000000 ) ;
#36499 = VECTOR ( 'NONE', #16752, 1000.000000000000000 ) ;
#36500 = PLANE ( 'NONE',  #13499 ) ;
#36501 = CARTESIAN_POINT ( 'NONE',  ( -336.3521761649654422, -164.5945333327934463, -42.41660376256285048 ) ) ;
#36502 = ORIENTED_EDGE ( 'NONE', *, *, #27401, .T. ) ;
#36503 = ORIENTED_EDGE ( 'NONE', *, *, #21336, .T. ) ;
#36504 = ADVANCED_FACE ( 'NONE', ( #22840 ), #31231, .T. ) ;
#36505 = ORIENTED_EDGE ( 'NONE', *, *, #18240, .T. ) ;
#36506 = VECTOR ( 'NONE', #36311, 1000.000000000000114 ) ;
#36507 = EDGE_CURVE ( 'NONE', #34352, #38645, #10486, .T. ) ;
#36508 = LINE ( 'NONE', #4730, #15072 ) ;
#36509 = EDGE_CURVE ( 'NONE', #40230, #41523, #28389, .T. ) ;
#36510 = DIRECTION ( 'NONE',  ( 0.000000000000000000, -0.3546048870425426158, -0.9350162426854120579 ) ) ;
#36511 = VECTOR ( 'NONE', #42286, 1000.000000000000000 ) ;
#36512 = DIRECTION ( 'NONE',  ( 0.000000000000000000, -0.4647231720437664526, 0.8854560256532110207 ) ) ;
#36513 = DIRECTION ( 'NONE',  ( 0.000000000000000000, 0.000000000000000000, 1.000000000000000000 ) ) ;
#36514 = AXIS2_PLACEMENT_3D ( 'NONE', #42145, #6169, #1956 ) ;
#36515 = EDGE_CURVE ( 'NONE', #16210, #20990, #2609, .T. ) ;
#36516 = ORIENTED_EDGE ( 'NONE', *, *, #25967, .T. ) ;
#36517 = CARTESIAN_POINT ( 'NONE',  ( -365.0160704661291788, -93.50000000000002842, 51.54700538379266561 ) ) ;
#36518 = CIRCLE ( 'NONE', #30664, 125.0000000000000000 ) ;
#36519 = LINE ( 'NONE', #8671, #31061 ) ;
#36520 = VERTEX_POINT ( 'NONE', #38348 ) ;
#36521 = CARTESIAN_POINT ( 'NONE',  ( -63.96873441216509093, -175.3837268820161057, -123.0287672223651612 ) ) ;
#36522 = VERTEX_POINT ( 'NONE', #2362 ) ;
#36523 = VECTOR ( 'NONE', #13410, 1000.000000000000000 ) ;
#36524 = EDGE_LOOP ( 'NONE', ( #15028, #18791, #27672, #33720 ) ) ;
#36525 = DIRECTION ( 'NONE',  ( 0.000000000000000000, 0.000000000000000000, 1.000000000000000000 ) ) ;
#36526 = CARTESIAN_POINT ( 'NONE',  ( -339.1964088526558498, -178.4886558749180949, 21.38919645685277970 ) ) ;
#36527 = FACE_OUTER_BOUND ( 'NONE', #27331, .T. ) ;
#36528 = EDGE_CURVE ( 'NONE', #4350, #39566, #20881, .T. ) ;
#36531 = ORIENTED_EDGE ( 'NONE', *, *, #13166, .T. ) ;
#36530 = CARTESIAN_POINT ( 'NONE',  ( -60.00000000000000000, -63.50000000000000000, 60.00000000000000711 ) ) ;
#36529 = DIRECTION ( 'NONE',  ( 0.7378332790417239107, 0.000000000000000000, 0.6749830015182142207 ) ) ;
#36532 = AXIS2_PLACEMENT_3D ( 'NONE', #11090, #42381, #50799 ) ;
#36533 = CARTESIAN_POINT ( 'NONE',  ( -47.60339180931321579, -189.7472609257535510, -0.4827922027307358088 ) ) ;
#36534 = CIRCLE ( 'NONE', #29830, 125.0000000000000568 ) ;
#36535 = ORIENTED_EDGE ( 'NONE', *, *, #43712, .T. ) ;
#36536 = CARTESIAN_POINT ( 'NONE',  ( -339.1964088526558498, -151.3613951634092700, -52.00954392751739164 ) ) ;
#36537 = DIRECTION ( 'NONE',  ( 0.000000000000000000, 0.4647231720437789981, 0.8854560256532044704 ) ) ;
#36538 = ORIENTED_EDGE ( 'NONE', *, *, #43975, .F. ) ;
#36539 = AXIS2_PLACEMENT_3D ( 'NONE', #32363, #12392, #28416 ) ;
#36540 = PLANE ( 'NONE',  #45101 ) ;
#36541 = DIRECTION ( 'NONE',  ( 0.000000000000000000, -1.000000000000000000, 0.000000000000000000 ) ) ;
#36543 = DIRECTION ( 'NONE',  ( 0.000000000000000000, 1.000000000000000000, 0.000000000000000000 ) ) ;
#36542 = LINE ( 'NONE', #39959, #4808 ) ;
#36544 = ORIENTED_EDGE ( 'NONE', *, *, #4412, .T. ) ;
#36545 = ADVANCED_FACE ( 'NONE', ( #34152 ), #2082, .T. ) ;
#36546 = DIRECTION ( 'NONE',  ( 1.000000000000000000, -0.000000000000000000, 0.000000000000000000 ) ) ;
#36547 = CARTESIAN_POINT ( 'NONE',  ( -59.16959496120699669, -183.6283474603465606, 123.5388265266452379 ) ) ;
#36548 = CARTESIAN_POINT ( 'NONE',  ( -48.47912675150885065, -177.1207230881787780, 6.938893903907228378E-15 ) ) ;
#36549 = ORIENTED_EDGE ( 'NONE', *, *, #51338, .T. ) ;
#36550 = CIRCLE ( 'NONE', #28964, 60.00000000000000000 ) ;
#36551 = DIRECTION ( 'NONE',  ( 0.000000000000000000, 0.000000000000000000, -1.000000000000000000 ) ) ;
#36552 = CARTESIAN_POINT ( 'NONE',  ( -336.3521761649654422, -114.7679482383557144, 58.37307289257701370 ) ) ;
#36553 = AXIS2_PLACEMENT_3D ( 'NONE', #42539, #26771, #34649 ) ;
#36554 = CARTESIAN_POINT ( 'NONE',  ( 15.80042947435468470, -189.7472609257535510, 107.2060569716377927 ) ) ;
#36555 = ADVANCED_FACE ( 'NONE', ( #6817 ), #38859, .F. ) ;
#36556 = EDGE_CURVE ( 'NONE', #44074, #33733, #15219, .T. ) ;
#36557 = EDGE_CURVE ( 'NONE', #31094, #23911, #34910, .T. ) ;
#36558 = ORIENTED_EDGE ( 'NONE', *, *, #5807, .F. ) ;
#36559 = ADVANCED_FACE ( 'NONE', ( #22064 ), #38606, .T. ) ;
#36560 = CARTESIAN_POINT ( 'NONE',  ( -44.48323084606168720, -193.5000000000000000, 124.9361149384469769 ) ) ;
#36561 = VECTOR ( 'NONE', #30091, 1000.000000000000000 ) ;
#36562 = DIRECTION ( 'NONE',  ( -0.3482016354343866471, 0.000000000000000000, -0.9374196611341253371 ) ) ;
#36563 = EDGE_CURVE ( 'NONE', #28503, #7450, #34411, .T. ) ;
#36564 = EDGE_LOOP ( 'NONE', ( #49131, #9547, #32216, #25375 ) ) ;
#36565 = LINE ( 'NONE', #13186, #20738 ) ;
#36566 = EDGE_LOOP ( 'NONE', ( #49946, #31663, #34922, #13553 ) ) ;
#36567 = LINE ( 'NONE', #569, #39050 ) ;
#36568 = ADVANCED_FACE ( 'NONE', ( #7073 ), #30978, .F. ) ;
#36569 = CARTESIAN_POINT ( 'NONE',  ( -339.1964088526558498, -150.9396941197155968, -53.35787839313373127 ) ) ;
#36570 = FACE_OUTER_BOUND ( 'NONE', #29679, .T. ) ;
#36571 = FACE_OUTER_BOUND ( 'NONE', #39513, .T. ) ;
#36572 = CARTESIAN_POINT ( 'NONE',  ( -330.4913330509368166, -70.60684477890951882, 28.32515014536777542 ) ) ;
#36573 = ADVANCED_FACE ( 'NONE', ( #39113 ), #43067, .F. ) ;
#36574 = EDGE_CURVE ( 'NONE', #21083, #40342, #6299, .T. ) ;
#36575 = DIRECTION ( 'NONE',  ( -0.9374196611341206742, 0.000000000000000000, -0.3482016354343996367 ) ) ;
#36576 = VECTOR ( 'NONE', #40188, 1000.000000000000114 ) ;
#36577 = EDGE_CURVE ( 'NONE', #42139, #7207, #31491, .T. ) ;
#36578 = CARTESIAN_POINT ( 'NONE',  ( -330.4913330509368166, -144.8891964568525452, -54.98865587491815177 ) ) ;
#36579 = LINE ( 'NONE', #11362, #1204 ) ;
#36581 = ORIENTED_EDGE ( 'NONE', *, *, #40156, .F. ) ;
#36580 = LINE ( 'NONE', #4799, #43807 ) ;
#36582 = MANIFOLD_SOLID_BREP ( 'Cut-Extrude9', #21210 ) ;
#36583 = VECTOR ( 'NONE', #10017, 1000.000000000000000 ) ;
#36584 = AXIS2_PLACEMENT_3D ( 'NONE', #27834, #8141, #4718 ) ;
#36585 = EDGE_CURVE ( 'NONE', #46182, #8223, #39879, .T. ) ;
#36586 = ORIENTED_EDGE ( 'NONE', *, *, #50725, .F. ) ;
#36587 = DIRECTION ( 'NONE',  ( 1.043714542225393539E-14, -0.8854560256532110207, -0.4647231720437664526 ) ) ;
#36588 = EDGE_CURVE ( 'NONE', #51365, #51208, #44378, .T. ) ;
#36589 = CARTESIAN_POINT ( 'NONE',  ( -47.64924157374594671, -193.5000000000000000, 123.9972451320097377 ) ) ;
#36590 = ORIENTED_EDGE ( 'NONE', *, *, #5437, .T. ) ;
#36591 = VERTEX_POINT ( 'NONE', #27288 ) ;
#36592 = VECTOR ( 'NONE', #5031, 1000.000000000000114 ) ;
#36593 = ORIENTED_EDGE ( 'NONE', *, *, #1695, .F. ) ;
#36594 = CARTESIAN_POINT ( 'NONE',  ( -332.3517673607765914, -175.3529239922484351, 30.18731974611377211 ) ) ;
#36595 = VECTOR ( 'NONE', #51637, 1000.000000000000000 ) ;
#36597 = VECTOR ( 'NONE', #29703, 1000.000000000000114 ) ;
#36596 = CARTESIAN_POINT ( 'NONE',  ( -48.82732838694325750, -183.6283474603465606, 0.9374196611341252261 ) ) ;
#36598 = LINE ( 'NONE', #32656, #36682 ) ;
#36599 = ORIENTED_EDGE ( 'NONE', *, *, #17683, .F. ) ;
#36600 = ORIENTED_EDGE ( 'NONE', *, *, #8636, .F. ) ;
#36601 = ADVANCED_FACE ( 'NONE', ( #7339 ), #8366, .T. ) ;
#36602 = EDGE_CURVE ( 'NONE', #24982, #5217, #43328, .T. ) ;
#36603 = AXIS2_PLACEMENT_3D ( 'NONE', #17305, #4685, #44627 ) ;
#36604 = DIRECTION ( 'NONE',  ( -0.000000000000000000, 0.3546048870425331789, -0.9350162426854158326 ) ) ;
#36605 = DIRECTION ( 'NONE',  ( -0.8455960035018311727, 0.000000000000000000, 0.5338233779647826305 ) ) ;
#36607 = ORIENTED_EDGE ( 'NONE', *, *, #22408, .F. ) ;
#36606 = DIRECTION ( 'NONE',  ( 0.000000000000000000, 0.000000000000000000, 1.000000000000000000 ) ) ;
#36608 = CARTESIAN_POINT ( 'NONE',  ( -336.3521761649654422, -123.5000000000000284, 0.000000000000000000 ) ) ;
#36609 = FACE_OUTER_BOUND ( 'NONE', #33495, .T. ) ;
#36610 = ORIENTED_EDGE ( 'NONE', *, *, #51350, .T. ) ;
#36611 = CARTESIAN_POINT ( 'NONE',  ( 29.27398957514434130, -183.6283474603465606, -97.87467957287998388 ) ) ;
#36612 = ORIENTED_EDGE ( 'NONE', *, *, #14700, .T. ) ;
#36613 = DIRECTION ( 'NONE',  ( 0.9995608365087944591, 0.000000000000000000, -0.02963332782255633305 ) ) ;
#36614 = DIRECTION ( 'NONE',  ( -0.000000000000000000, 1.000000000000000000, -0.000000000000000000 ) ) ;
#36615 = FACE_OUTER_BOUND ( 'NONE', #23817, .T. ) ;
#36616 = ORIENTED_EDGE ( 'NONE', *, *, #44663, .T. ) ;
#36617 = VECTOR ( 'NONE', #18547, 1000.000000000000000 ) ;
#36618 = ORIENTED_EDGE ( 'NONE', *, *, #12192, .T. ) ;
#36619 = CARTESIAN_POINT ( 'NONE',  ( -332.3517673607765914, -181.3443148879387081, 15.93848283698911317 ) ) ;
#36620 = VECTOR ( 'NONE', #26995, 1000.000000000000114 ) ;
#36621 = CARTESIAN_POINT ( 'NONE',  ( -4.794493649713349015, -189.7472609257535510, -117.1181148702518726 ) ) ;
#36622 = ORIENTED_EDGE ( 'NONE', *, *, #31824, .T. ) ;
#36623 = FACE_OUTER_BOUND ( 'NONE', #46419, .T. ) ;
#36624 = AXIS2_PLACEMENT_3D ( 'NONE', #50736, #14479, #2634 ) ;
#36625 = CARTESIAN_POINT ( 'NONE',  ( -336.3521761649654422, -120.8677111499054178, 59.94223098458771659 ) ) ;
#36626 = EDGE_CURVE ( 'NONE', #32221, #6345, #3907, .T. ) ;
#36627 = EDGE_CURVE ( 'NONE', #46318, #43845, #8102, .T. ) ;
#36628 = EDGE_LOOP ( 'NONE', ( #46000, #41195, #6653, #37114 ) ) ;
#36629 = DIRECTION ( 'NONE',  ( 0.000000000000000000, -0.5680647467311485954, 0.8229838658936613482 ) ) ;
#36630 = DIRECTION ( 'NONE',  ( 0.000000000000000000, 0.000000000000000000, -1.000000000000000000 ) ) ;
#36631 = EDGE_CURVE ( 'NONE', #38201, #16449, #40157, .T. ) ;
#36632 = ADVANCED_FACE ( 'NONE', ( #4420 ), #3634, .T. ) ;
#36633 = VERTEX_POINT ( 'NONE', #52013 ) ;
#36634 = DIRECTION ( 'NONE',  ( 0.000000000000000000, 0.000000000000000000, 1.000000000000000000 ) ) ;
#36635 = VERTEX_POINT ( 'NONE', #23604 ) ;
#36636 = AXIS2_PLACEMENT_3D ( 'NONE', #12693, #32927, #20591 ) ;
#36637 = DIRECTION ( 'NONE',  ( 0.2059786187411021818, 0.000000000000000000, -0.9785564922995032555 ) ) ;
#36638 = EDGE_LOOP ( 'NONE', ( #32999, #35171, #51280, #9976 ) ) ;
#36639 = AXIS2_PLACEMENT_3D ( 'NONE', #7560, #7049, #3609 ) ;
#36640 = AXIS2_PLACEMENT_3D ( 'NONE', #3791, #6532, #22559 ) ;
#36641 = DIRECTION ( 'NONE',  ( -0.5586467658036594619, 0.000000000000000000, 0.8294056854501971054 ) ) ;
#36642 = CARTESIAN_POINT ( 'NONE',  ( 141.7825277784304205, -193.5000000000000000, 10.00000000000000178 ) ) ;
#36643 = DIRECTION ( 'NONE',  ( 1.000000000000000000, -0.000000000000000000, -0.000000000000000000 ) ) ;
#36644 = VECTOR ( 'NONE', #33757, 999.9999999999998863 ) ;
#36645 = DIRECTION ( 'NONE',  ( 0.000000000000000000, -1.047444401652940007E-14, -1.000000000000000000 ) ) ;
#36646 = ORIENTED_EDGE ( 'NONE', *, *, #44570, .F. ) ;
#36648 = CIRCLE ( 'NONE', #31608, 125.0000000000000000 ) ;
#36647 = DIRECTION ( 'NONE',  ( 0.000000000000000000, -0.4647231720437755564, -0.8854560256532062468 ) ) ;
#36649 = ORIENTED_EDGE ( 'NONE', *, *, #22045, .T. ) ;
#36650 = VERTEX_POINT ( 'NONE', #39621 ) ;
#36651 = PRODUCT_DEFINITION ( 'UNKNOWN', '', #48565, #7476 ) ;
#36652 = DIRECTION ( 'NONE',  ( 0.000000000000000000, -0.8854560256532043594, 0.4647231720437789981 ) ) ;
#36654 = ORIENTED_EDGE ( 'NONE', *, *, #51284, .T. ) ;
#36653 = CARTESIAN_POINT ( 'NONE',  ( 75.17589904515342880, -175.3837268820161057, -18.28755301364250130 ) ) ;
#36655 = ORIENTED_EDGE ( 'NONE', *, *, #6032, .T. ) ;
#36656 = CARTESIAN_POINT ( 'NONE',  ( -332.3517673607765914, -77.59233547837267508, 37.15394033962009246 ) ) ;
#36657 = EDGE_CURVE ( 'NONE', #38881, #44484, #48568, .T. ) ;
#36658 = DIRECTION ( 'NONE',  ( 0.000000000000000000, 1.000000000000000000, -0.000000000000000000 ) ) ;
#36659 = AXIS2_PLACEMENT_3D ( 'NONE', #40834, #40306, #36645 ) ;
#36660 = VECTOR ( 'NONE', #15318, 1000.000000000000000 ) ;
#36661 = ORIENTED_EDGE ( 'NONE', *, *, #1208, .F. ) ;
#36662 = DIRECTION ( 'NONE',  ( 0.000000000000000000, 0.000000000000000000, -1.000000000000000000 ) ) ;
#36663 = VERTEX_POINT ( 'NONE', #20185 ) ;
#36664 = PLANE ( 'NONE',  #18304 ) ;
#36665 = DIRECTION ( 'NONE',  ( 0.000000000000000000, -0.000000000000000000, -1.000000000000000000 ) ) ;
#36666 = VECTOR ( 'NONE', #12135, 1000.000000000000114 ) ;
#36667 = CARTESIAN_POINT ( 'NONE',  ( -48.47912675150885065, -177.1207230881787780, 6.938893903907228378E-15 ) ) ;
#36668 = DIRECTION ( 'NONE',  ( -0.000000000000000000, 1.000000000000000000, -0.000000000000000000 ) ) ;
#36669 = VERTEX_POINT ( 'NONE', #16518 ) ;
#36670 = ORIENTED_EDGE ( 'NONE', *, *, #15475, .T. ) ;
#36671 = ORIENTED_EDGE ( 'NONE', *, *, #48461, .F. ) ;
#36672 = DIRECTION ( 'NONE',  ( -0.000000000000000000, 1.000000000000000000, -0.000000000000000000 ) ) ;
#36673 = DIRECTION ( 'NONE',  ( 0.7765238627180437447, 0.000000000000000000, -0.6300878435817094392 ) ) ;
#36674 = VECTOR ( 'NONE', #51559, 1000.000000000000000 ) ;
#36675 = CIRCLE ( 'NONE', #24898, 60.00000000000000000 ) ;
#36676 = CARTESIAN_POINT ( 'NONE',  ( -170.0502155641509319, -177.1207230881787780, -29.07697310430878090 ) ) ;
#36677 = VECTOR ( 'NONE', #26849, 1000.000000000000227 ) ;
#36679 = VECTOR ( 'NONE', #11350, 1000.000000000000000 ) ;
#36678 = FACE_BOUND ( 'NONE', #38657, .T. ) ;
#36680 = FACE_OUTER_BOUND ( 'NONE', #44111, .T. ) ;
#36681 = EDGE_LOOP ( 'NONE', ( #10730, #21877, #25489, #38393 ) ) ;
#36682 = VECTOR ( 'NONE', #48700, 1000.000000000000000 ) ;
#36683 = AXIS2_PLACEMENT_3D ( 'NONE', #18659, #10767, #11012 ) ;
#36684 = ORIENTED_EDGE ( 'NONE', *, *, #24591, .T. ) ;
#36686 = ORIENTED_EDGE ( 'NONE', *, *, #36756, .T. ) ;
#36685 = PLANE ( 'NONE',  #44093 ) ;
#36687 = DIRECTION ( 'NONE',  ( -0.000000000000000000, 1.000000000000000000, -0.000000000000000000 ) ) ;
#36688 = EDGE_LOOP ( 'NONE', ( #36493, #21326, #666, #39356 ) ) ;
#36689 = DIRECTION ( 'NONE',  ( -0.000000000000000000, 1.000000000000000000, -0.000000000000000000 ) ) ;
#36690 = DIRECTION ( 'NONE',  ( -0.000000000000000000, 1.000000000000000000, -0.000000000000000000 ) ) ;
#36691 = LINE ( 'NONE', #48785, #24636 ) ;
#36692 = ADVANCED_FACE ( 'NONE', ( #20441 ), #36209, .T. ) ;
#36693 = DIRECTION ( 'NONE',  ( -1.000000000000000000, 0.000000000000000000, 0.000000000000000000 ) ) ;
#36694 = ORIENTED_EDGE ( 'NONE', *, *, #20036, .T. ) ;
#36695 = CARTESIAN_POINT ( 'NONE',  ( -339.1964088526558498, -102.1108035431470427, 54.98865587491797413 ) ) ;
#36696 = EDGE_LOOP ( 'NONE', ( #32752, #41869, #37106, #33738 ) ) ;
#36697 = ORIENTED_EDGE ( 'NONE', *, *, #28496, .T. ) ;
#36698 = DIRECTION ( 'NONE',  ( 0.000000000000000000, 0.000000000000000000, -1.000000000000000000 ) ) ;
#36699 = AXIS2_PLACEMENT_3D ( 'NONE', #19366, #23561, #51186 ) ;
#36700 = VECTOR ( 'NONE', #8989, 1000.000000000000000 ) ;
#36701 = LINE ( 'NONE', #20402, #4334 ) ;
#36702 = DIRECTION ( 'NONE',  ( 0.9027978299657387629, 0.000000000000000000, 0.4300652022765304450 ) ) ;
#36703 = DIRECTION ( 'NONE',  ( 8.659560562354941486E-17, -0.7071067811865469066, 0.7071067811865482389 ) ) ;
#36704 = VECTOR ( 'NONE', #49917, 1000.000000000000000 ) ;
#36705 = DIRECTION ( 'NONE',  ( 0.7765238627180437447, 0.000000000000000000, -0.6300878435817094392 ) ) ;
#36706 = DIRECTION ( 'NONE',  ( 0.000000000000000000, 0.000000000000000000, -1.000000000000000000 ) ) ;
#36707 = DIRECTION ( 'NONE',  ( 0.000000000000000000, 0.000000000000000000, 1.000000000000000000 ) ) ;
#36708 = ORIENTED_EDGE ( 'NONE', *, *, #3184, .F. ) ;
#36709 = DIRECTION ( 'NONE',  ( -1.000000000000000000, 0.000000000000000000, 0.000000000000000000 ) ) ;
#36710 = CARTESIAN_POINT ( 'NONE',  ( -48.47912675150885065, -175.3837268820161057, 6.938893903907228378E-15 ) ) ;
#36711 = DIRECTION ( 'NONE',  ( -0.000000000000000000, 1.000000000000000000, -0.000000000000000000 ) ) ;
#36712 = FACE_BOUND ( 'NONE', #10241, .T. ) ;
#36713 = EDGE_LOOP ( 'NONE', ( #27290, #43411, #1491, #1415 ) ) ;
#36714 = VECTOR ( 'NONE', #44235, 1000.000000000000114 ) ;
#36715 = AXIS2_PLACEMENT_3D ( 'NONE', #28449, #41315, #24512 ) ;
#36716 = EDGE_CURVE ( 'NONE', #11672, #15110, #9153, .T. ) ;
#36717 = DIRECTION ( 'NONE',  ( -0.000000000000000000, 1.000000000000000000, -0.000000000000000000 ) ) ;
#36718 = ORIENTED_EDGE ( 'NONE', *, *, #43369, .T. ) ;
#36719 = VECTOR ( 'NONE', #2031, 1000.000000000000000 ) ;
#36720 = LINE ( 'NONE', #8848, #17748 ) ;
#36721 = ORIENTED_EDGE ( 'NONE', *, *, #24518, .F. ) ;
#36722 = CARTESIAN_POINT ( 'NONE',  ( 25.00456841203573077, 45.00000000000000000, 0.000000000000000000 ) ) ;
#36723 = AXIS2_PLACEMENT_3D ( 'NONE', #32284, #32816, #35715 ) ;
#36724 = ORIENTED_EDGE ( 'NONE', *, *, #612, .T. ) ;
#36725 = CARTESIAN_POINT ( 'NONE',  ( -330.4913330509368166, -167.9936954712156023, -38.74998146212117689 ) ) ;
#36726 = DIRECTION ( 'NONE',  ( 0.000000000000000000, 0.000000000000000000, 1.000000000000000000 ) ) ;
#36727 = DIRECTION ( 'NONE',  ( 1.000000000000000000, 0.000000000000000000, 0.000000000000000000 ) ) ;
#36728 = ADVANCED_FACE ( 'NONE', ( #40658 ), #36995, .F. ) ;
#36729 = DIRECTION ( 'NONE',  ( 0.000000000000000000, -1.000000000000000000, 0.000000000000000000 ) ) ;
#36730 = ORIENTED_EDGE ( 'NONE', *, *, #30628, .T. ) ;
#36731 = ORIENTED_EDGE ( 'NONE', *, *, #4181, .T. ) ;
#36732 =( REPRESENTATION_RELATIONSHIP ('NONE','NONE', #4578, #40181 ) REPRESENTATION_RELATIONSHIP_WITH_TRANSFORMATION ( #5769 )SHAPE_REPRESENTATION_RELATIONSHIP( ) );
#36733 = DIRECTION ( 'NONE',  ( 0.000000000000000000, 0.000000000000000000, 1.000000000000000000 ) ) ;
#36734 = AXIS2_PLACEMENT_3D ( 'NONE', #28461, #44508, #8495 ) ;
#36735 = DIRECTION ( 'NONE',  ( -0.000000000000000000, 1.000000000000000000, -0.000000000000000000 ) ) ;
#36736 = CIRCLE ( 'NONE', #14090, 60.00000000000000000 ) ;
#36737 = ADVANCED_FACE ( 'NONE', ( #9661 ), #45168, .T. ) ;
#36738 = VERTEX_POINT ( 'NONE', #48585 ) ;
#36739 = LINE ( 'NONE', #33313, #729 ) ;
#36740 = DIRECTION ( 'NONE',  ( -0.000000000000000000, 1.000000000000000000, -0.000000000000000000 ) ) ;
#36741 = DIRECTION ( 'NONE',  ( 0.9473263538541923934, 0.000000000000000000, -0.3202698538628350744 ) ) ;
#36742 = VECTOR ( 'NONE', #21681, 1000.000000000000114 ) ;
#36743 = ADVANCED_FACE ( 'NONE', ( #40933 ), #8614, .T. ) ;
#36744 = LINE ( 'NONE', #20708, #25084 ) ;
#36745 = CARTESIAN_POINT ( 'NONE',  ( 7.403327498934737960, -175.3837268820161057, -110.6939782313521192 ) ) ;
#36746 = VERTEX_POINT ( 'NONE', #4682 ) ;
#36749 = ORIENTED_EDGE ( 'NONE', *, *, #49963, .F. ) ;
#36748 = DIRECTION ( 'NONE',  ( 0.000000000000000000, -0.3546048870425267951, 0.9350162426854181641 ) ) ;
#36747 = CARTESIAN_POINT ( 'NONE',  ( 46.00000000000000711, 35.00000000000000000, -35.00000000000000000 ) ) ;
#36750 = ORIENTED_EDGE ( 'NONE', *, *, #50117, .T. ) ;
#36751 = DIRECTION ( 'NONE',  ( 0.000000000000000000, 1.000000000000000000, 0.000000000000000000 ) ) ;
#36752 = VERTEX_POINT ( 'NONE', #41716 ) ;
#36753 = CARTESIAN_POINT ( 'NONE',  ( 2.390048994689182728E-16, 105.2299100483173078, -110.8702827025711599 ) ) ;
#36754 = ORIENTED_EDGE ( 'NONE', *, *, #51100, .T. ) ;
#36755 = DIRECTION ( 'NONE',  ( 0.000000000000000000, 1.000000000000000000, 0.000000000000000000 ) ) ;
#36756 = EDGE_CURVE ( 'NONE', #13900, #17812, #17044, .T. ) ;
#36757 = DIRECTION ( 'NONE',  ( -0.000000000000000000, 1.000000000000000000, -0.000000000000000000 ) ) ;
#36758 = ORIENTED_EDGE ( 'NONE', *, *, #4156, .F. ) ;
#36760 = CARTESIAN_POINT ( 'NONE',  ( -339.1964088526558498, -108.8949048983204051, 57.16590939599314680 ) ) ;
#36759 = CARTESIAN_POINT ( 'NONE',  ( -160.0000000000000284, -123.5000000000000284, -37.63467731922663972 ) ) ;
#36761 = ORIENTED_EDGE ( 'NONE', *, *, #50938, .F. ) ;
#36762 = EDGE_CURVE ( 'NONE', #46453, #19312, #3244, .T. ) ;
#36763 = AXIS2_PLACEMENT_3D ( 'NONE', #39623, #12028, #208 ) ;
#36764 = VERTEX_POINT ( 'NONE', #49363 ) ;
#36765 = DIRECTION ( 'NONE',  ( -0.1476465640024918202, 0.000000000000000000, 0.9890401873221624784 ) ) ;
#36766 = EDGE_CURVE ( 'NONE', #48486, #30945, #36744, .T. ) ;
#36767 = DIRECTION ( 'NONE',  ( 0.000000000000000000, -0.7071067811865469066, -0.7071067811865482389 ) ) ;
#36768 = CARTESIAN_POINT ( 'NONE',  ( -336.3521761649654422, -135.0638248728647852, 57.91551518289418254 ) ) ;
#36769 = DIRECTION ( 'NONE',  ( 1.000000000000000000, 4.952603889764026625E-17, 7.175085443855094401E-17 ) ) ;
#36770 = ORIENTED_EDGE ( 'NONE', *, *, #44513, .T. ) ;
#36771 = CARTESIAN_POINT ( 'NONE',  ( -336.3521761649654422, -107.7955183043589500, 56.89493493766750731 ) ) ;
#36772 = CONTEXT_DEPENDENT_SHAPE_REPRESENTATION ( #47478, #44864 ) ;
#36773 = DIRECTION ( 'NONE',  ( 1.000000000000000000, 0.000000000000000000, 0.000000000000000000 ) ) ;
#36774 = DIRECTION ( 'NONE',  ( 0.8124868780056825335, 0.000000000000000000, -0.5829794791144703447 ) ) ;
#36775 = DIRECTION ( 'NONE',  ( 0.000000000000000000, 0.000000000000000000, -1.000000000000000000 ) ) ;
#36776 = DIRECTION ( 'NONE',  ( 0.000000000000000000, -1.000000000000000000, -0.000000000000000000 ) ) ;
#36777 = ORIENTED_EDGE ( 'NONE', *, *, #30622, .T. ) ;
#36778 = ORIENTED_EDGE ( 'NONE', *, *, #20539, .T. ) ;
#36779 = AXIS2_PLACEMENT_3D ( 'NONE', #19372, #34864, #35385 ) ;
#36780 = CARTESIAN_POINT ( 'NONE',  ( -48.71401279728982558, -193.5000000000000000, -0.9720229140804069745 ) ) ;
#36781 = VECTOR ( 'NONE', #22654, 1000.000000000000000 ) ;
#36782 = ADVANCED_FACE ( 'NONE', ( #17302 ), #25179, .T. ) ;
#36783 = AXIS2_PLACEMENT_3D ( 'NONE', #12081, #24447, #36525 ) ;
#36784 = DIRECTION ( 'NONE',  ( 0.000000000000000000, -1.000000000000000000, 0.000000000000000000 ) ) ;
#36785 = LINE ( 'NONE', #24429, #25789 ) ;
#36786 = VERTEX_POINT ( 'NONE', #21755 ) ;
#36787 = ORIENTED_EDGE ( 'NONE', *, *, #10249, .F. ) ;
#36788 = VERTEX_POINT ( 'NONE', #37770 ) ;
#36789 = AXIS2_PLACEMENT_3D ( 'NONE', #39613, #35423, #19157 ) ;
#36790 = CYLINDRICAL_SURFACE ( 'NONE', #46099, 125.0000000000000000 ) ;
#36791 = CARTESIAN_POINT ( 'NONE',  ( -339.1964088526558498, -64.86990808808704401, 6.615309698014191220 ) ) ;
#36792 = CARTESIAN_POINT ( 'NONE',  ( 20.65191334053706029, -189.7472609257535510, 102.9412430821799802 ) ) ;
#36793 = DIRECTION ( 'NONE',  ( 0.000000000000000000, 0.000000000000000000, -1.000000000000000000 ) ) ;
#36794 = ORIENTED_EDGE ( 'NONE', *, *, #51209, .F. ) ;
#36795 = DIRECTION ( 'NONE',  ( 0.9960498426152171181, 0.000000000000000000, -0.08879589532293157006 ) ) ;
#36796 = CARTESIAN_POINT ( 'NONE',  ( -92.43312097795266880, -189.7472609257535510, -115.9484881370935483 ) ) ;
#36797 = VERTEX_POINT ( 'NONE', #37517 ) ;
#36798 = AXIS2_PLACEMENT_3D ( 'NONE', #47555, #12039, #15491 ) ;
#36799 = CARTESIAN_POINT ( 'NONE',  ( 74.60098876342244978, -177.1207230881787780, 21.82395850507349522 ) ) ;
#36800 = ORIENTED_EDGE ( 'NONE', *, *, #26777, .F. ) ;
#36801 = EDGE_LOOP ( 'NONE', ( #45392, #16032, #2213, #42540 ) ) ;
#36802 = DIRECTION ( 'NONE',  ( -0.6300878435817094392, 0.000000000000000000, -0.7765238627180437447 ) ) ;
#36803 = EDGE_CURVE ( 'NONE', #44752, #39919, #5215, .T. ) ;
#36804 = EDGE_CURVE ( 'NONE', #6572, #51893, #49612, .T. ) ;
#36805 = PLANE ( 'NONE',  #22638 ) ;
#36806 = CARTESIAN_POINT ( 'NONE',  ( -134.9506378406916838, -189.7472609257535510, 90.26448786734087548 ) ) ;
#36809 = EDGE_LOOP ( 'NONE', ( #26, #49790, #27809, #39172 ) ) ;
#36808 = CARTESIAN_POINT ( 'NONE',  ( 64.44365795514079309, -189.7472609257535510, -53.60452120946192878 ) ) ;
#36807 = DIRECTION ( 'NONE',  ( 0.000000000000000000, -0.000000000000000000, 1.000000000000000000 ) ) ;
#36810 = VECTOR ( 'NONE', #12958, 1000.000000000000000 ) ;
#36811 = AXIS2_PLACEMENT_3D ( 'NONE', #6570, #18644, #23104 ) ;
#36812 = DIRECTION ( 'NONE',  ( 0.4300652022765245608, 0.000000000000000000, -0.9027978299657416494 ) ) ;
#36813 = ADVANCED_BREP_SHAPE_REPRESENTATION ( '', ( #35805, #31742 ), #46023 ) ;
#36814 = ORIENTED_EDGE ( 'NONE', *, *, #5015, .F. ) ;
#36815 = LINE ( 'NONE', #13674, #40652 ) ;
#36817 = STYLED_ITEM ( 'NONE', ( #25174 ), #35629 ) ;
#36816 = CARTESIAN_POINT ( 'NONE',  ( -126.2322430781613605, -183.6283474603465606, 97.87467957288053810 ) ) ;
#36818 = EDGE_LOOP ( 'NONE', ( #14641, #21823, #39898, #42224 ) ) ;
#36819 = EDGE_CURVE ( 'NONE', #14709, #6578, #13351, .T. ) ;
#36820 = LINE ( 'NONE', #48913, #14948 ) ;
#36822 = DIRECTION ( 'NONE',  ( -0.000000000000000000, 1.000000000000000000, -0.000000000000000000 ) ) ;
#36821 = CARTESIAN_POINT ( 'NONE',  ( -330.4913330509368166, -162.9117225908385365, 45.24064679492094143 ) ) ;
#36823 = ORIENTED_EDGE ( 'NONE', *, *, #3234, .F. ) ;
#36824 = ADVANCED_FACE ( 'NONE', ( #29622 ), #8879, .F. ) ;
#36825 = VECTOR ( 'NONE', #3901, 1000.000000000000000 ) ;
#36826 = CARTESIAN_POINT ( 'NONE',  ( -5.113431607746562690, -189.7472609257535510, 117.2365833888819537 ) ) ;
#36827 = DIRECTION ( 'NONE',  ( -1.000000000000000000, 0.000000000000000000, -0.000000000000000000 ) ) ;
#36828 = EDGE_CURVE ( 'NONE', #9325, #21275, #44623, .T. ) ;
#36829 = CARTESIAN_POINT ( 'NONE',  ( -43.48323084606168720, -183.6283474603465606, 124.9001241957026167 ) ) ;
#36830 = VERTEX_POINT ( 'NONE', #9408 ) ;
#36831 = LINE ( 'NONE', #17125, #48428 ) ;
#36832 = DIRECTION ( 'NONE',  ( 0.000000000000000000, 1.000000000000000000, 0.000000000000000000 ) ) ;
#36833 = CARTESIAN_POINT ( 'NONE',  ( -49.32472275501068282, -193.5000000000000000, 0.5338233779647895139 ) ) ;
#36834 = EDGE_CURVE ( 'NONE', #42669, #47727, #25433, .T. ) ;
#36835 = VERTEX_POINT ( 'NONE', #13600 ) ;
#36836 = DIRECTION ( 'NONE',  ( -0.9960498426152177842, 0.000000000000000000, 0.08879589532292482545 ) ) ;
#36837 = VECTOR ( 'NONE', #36693, 1000.000000000000000 ) ;
#36838 = CARTESIAN_POINT ( 'NONE',  ( -48.47912675150885065, -189.7472609257535510, 6.938893903907228378E-15 ) ) ;
#36839 = ORIENTED_EDGE ( 'NONE', *, *, #46548, .F. ) ;
#36840 = CARTESIAN_POINT ( 'NONE',  ( -336.3521761649654422, -72.01665693856799066, -28.86398714850468039 ) ) ;
#36841 = DIRECTION ( 'NONE',  ( -0.8124868780056825335, 0.000000000000000000, 0.5829794791144703447 ) ) ;
#36842 = DIRECTION ( 'NONE',  ( -0.01787127051204794384, -0.8746197071393964073, 0.4844801188631808198 ) ) ;
#36843 = CARTESIAN_POINT ( 'NONE',  ( -48.47912675150885065, -189.7472609257535510, 6.938893903907228378E-15 ) ) ;
#36844 = FACE_OUTER_BOUND ( 'NONE', #945, .T. ) ;
#36845 = DIRECTION ( 'NONE',  ( -1.000000000000000000, 0.000000000000000000, -0.000000000000000000 ) ) ;
#36846 = AXIS2_PLACEMENT_3D ( 'NONE', #7318, #3618, #31743 ) ;
#36847 = DIRECTION ( 'NONE',  ( -0.9063077870366494926, 5.175581015019669255E-17, -0.4226182617407002740 ) ) ;
#36848 = CARTESIAN_POINT ( 'NONE',  ( -135.6699833737243353, -175.3837268820161057, 89.56983042009326823 ) ) ;
#36850 = ORIENTED_EDGE ( 'NONE', *, *, #568, .F. ) ;
#36849 = DIRECTION ( 'NONE',  ( 0.000000000000000000, -1.000000000000000000, 0.000000000000000000 ) ) ;
#36851 = MANIFOLD_SOLID_BREP ( 'Boss-Extrude11', #35479 ) ;
#36852 = VERTEX_POINT ( 'NONE', #43167 ) ;
#36853 = DIRECTION ( 'NONE',  ( 0.000000000000000000, -1.000000000000000000, 0.000000000000000000 ) ) ;
#36854 = DIRECTION ( 'NONE',  ( 0.1182731709213592358, 0.000000000000000000, 0.9929810960135178055 ) ) ;
#36855 = EDGE_LOOP ( 'NONE', ( #21642, #24918, #15664, #35059 ) ) ;
#36856 = CIRCLE ( 'NONE', #49452, 125.0000000000000000 ) ;
#36857 = VERTEX_POINT ( 'NONE', #7172 ) ;
#36859 = ADVANCED_FACE ( 'NONE', ( #39231 ), #48095, .T. ) ;
#36858 = ORIENTED_EDGE ( 'NONE', *, *, #16951, .T. ) ;
#36860 = DIRECTION ( 'NONE',  ( 0.000000000000000000, 1.000000000000000000, 0.000000000000000000 ) ) ;
#36861 = ADVANCED_FACE ( 'NONE', ( #20483 ), #1031, .T. ) ;
#36862 = EDGE_CURVE ( 'NONE', #42377, #20555, #36508, .T. ) ;
#36863 = EDGE_CURVE ( 'NONE', #18649, #51271, #508, .T. ) ;
#36864 = DIRECTION ( 'NONE',  ( 0.000000000000000000, 0.3546048870425300148, -0.9350162426854169428 ) ) ;
#36865 = FACE_OUTER_BOUND ( 'NONE', #32872, .T. ) ;
#36866 = ORIENTED_EDGE ( 'NONE', *, *, #18900, .F. ) ;
#36867 = ORIENTED_EDGE ( 'NONE', *, *, #35945, .T. ) ;
#36868 = EDGE_CURVE ( 'NONE', #49664, #36451, #15029, .T. ) ;
#36869 = AXIS2_PLACEMENT_3D ( 'NONE', #43210, #27700, #7222 ) ;
#36870 = DIRECTION ( 'NONE',  ( 1.000000000000000000, -0.000000000000000000, 0.000000000000000000 ) ) ;
#36872 = EDGE_LOOP ( 'NONE', ( #42835, #12324, #47735, #51464 ) ) ;
#36871 = CARTESIAN_POINT ( 'NONE',  ( -163.3245969606054473, -193.5000000000000000, -46.76022031560622594 ) ) ;
#36873 = ADVANCED_FACE ( 'NONE', ( #32305 ), #4212, .F. ) ;
#36874 = DIRECTION ( 'NONE',  ( 0.000000000000000000, -1.000000000000000000, 0.000000000000000000 ) ) ;
#36875 = ORIENTED_EDGE ( 'NONE', *, *, #27407, .F. ) ;
#36876 = DIRECTION ( 'NONE',  ( 0.1182731709213660498, 0.000000000000000000, -0.9929810960135169173 ) ) ;
#36877 = ORIENTED_EDGE ( 'NONE', *, *, #23117, .T. ) ;
#36878 = CARTESIAN_POINT ( 'NONE',  ( -332.3517673607765914, -161.4024510877913485, 45.24454186338643780 ) ) ;
#36879 = EDGE_CURVE ( 'NONE', #51152, #22837, #17087, .T. ) ;
#36880 = DIRECTION ( 'NONE',  ( -1.000000000000000000, 0.000000000000000000, 0.000000000000000000 ) ) ;
#36881 = PLANE ( 'NONE',  #47536 ) ;
#36882 = ADVANCED_FACE ( 'NONE', ( #8406 ), #36253, .T. ) ;
#36883 = EDGE_LOOP ( 'NONE', ( #28524, #4299, #22528, #33693 ) ) ;
#36884 = ORIENTED_EDGE ( 'NONE', *, *, #33903, .T. ) ;
#36885 = CYLINDRICAL_SURFACE ( 'NONE', #21400, 20.00000000000001776 ) ;
#36886 = ADVANCED_FACE ( 'NONE', ( #48630 ), #40449, .T. ) ;
#36888 = VECTOR ( 'NONE', #26169, 1000.000000000000000 ) ;
#36887 = DIRECTION ( 'NONE',  ( 0.000000000000000000, 0.000000000000000000, 1.000000000000000000 ) ) ;
#36889 = EDGE_LOOP ( 'NONE', ( #40010, #32009, #30728, #49942 ) ) ;
#36890 = DIRECTION ( 'NONE',  ( 1.000000000000000000, -0.000000000000000000, 0.000000000000000000 ) ) ;
#36891 = AXIS2_PLACEMENT_3D ( 'NONE', #41250, #42549, #30711 ) ;
#36892 = EDGE_CURVE ( 'NONE', #41489, #40958, #25220, .T. ) ;
#36893 = CYLINDRICAL_SURFACE ( 'NONE', #13654, 125.0000000000000000 ) ;
#36894 = EDGE_LOOP ( 'NONE', ( #30353, #28337, #25599, #21826 ) ) ;
#36895 = CARTESIAN_POINT ( 'NONE',  ( -120.2975302769383177, -183.6283474603465606, 102.3089288139533863 ) ) ;
#36896 = EDGE_CURVE ( 'NONE', #22006, #32508, #251, .T. ) ;
#36897 = CYLINDRICAL_SURFACE ( 'NONE', #14681, 125.0000000000000000 ) ;
#36898 = ORIENTED_EDGE ( 'NONE', *, *, #29540, .T. ) ;
#36899 = DIRECTION ( 'NONE',  ( 0.000000000000000000, 0.000000000000000000, -1.000000000000000000 ) ) ;
#36900 = EDGE_LOOP ( 'NONE', ( #28366, #50617, #23606, #8519 ) ) ;
#36901 = DIRECTION ( 'NONE',  ( -0.000000000000000000, -1.000000000000000000, 0.000000000000000000 ) ) ;
#36902 = ORIENTED_EDGE ( 'NONE', *, *, #29744, .F. ) ;
#36903 = DIRECTION ( 'NONE',  ( -0.000000000000000000, -1.000000000000000000, 0.000000000000000000 ) ) ;
#36904 = PLANE ( 'NONE',  #20494 ) ;
#36905 = DIRECTION ( 'NONE',  ( -0.000000000000000000, 0.000000000000000000, -1.000000000000000000 ) ) ;
#36906 = FACE_OUTER_BOUND ( 'NONE', #48958, .T. ) ;
#36907 = ADVANCED_FACE ( 'NONE', ( #44145 ), #36790, .T. ) ;
#36908 = VECTOR ( 'NONE', #25425, 1000.000000000000000 ) ;
#36909 = EDGE_LOOP ( 'NONE', ( #25194, #26022, #39295, #7185 ) ) ;
#36910 = DIRECTION ( 'NONE',  ( -0.000000000000000000, 0.000000000000000000, 1.000000000000000000 ) ) ;
#36911 = EDGE_LOOP ( 'NONE', ( #20102, #24978, #48730, #3312 ) ) ;
#36912 = ORIENTED_EDGE ( 'NONE', *, *, #31391, .F. ) ;
#36913 = FACE_OUTER_BOUND ( 'NONE', #2820, .T. ) ;
#36915 = ORIENTED_EDGE ( 'NONE', *, *, #7964, .T. ) ;
#36914 = LINE ( 'NONE', #49006, #18614 ) ;
#36916 = ORIENTED_EDGE ( 'NONE', *, *, #32113, .T. ) ;
#36917 = LINE ( 'NONE', #5654, #23215 ) ;
#36918 = EDGE_CURVE ( 'NONE', #42898, #47538, #12862, .T. ) ;
#36919 = CARTESIAN_POINT ( 'NONE',  ( -305.0000000000000568, -65.12585595286530804, -13.87297036558380725 ) ) ;
#36920 = ORIENTED_EDGE ( 'NONE', *, *, #48473, .T. ) ;
#36921 = VECTOR ( 'NONE', #21145, 999.9999999999998863 ) ;
#36922 = CARTESIAN_POINT ( 'NONE',  ( 12.12533326292403935, -177.1207230881787780, 109.3256576763158847 ) ) ;
#36923 = ORIENTED_EDGE ( 'NONE', *, *, #1105, .F. ) ;
#36924 = CARTESIAN_POINT ( 'NONE',  ( 51.05451324771861010, -183.6283474603465606, 75.61781872352699452 ) ) ;
#36925 = DIRECTION ( 'NONE',  ( 1.000000000000000000, 0.000000000000000000, 0.000000000000000000 ) ) ;
#36926 = EDGE_CURVE ( 'NONE', #49023, #49872, #21015, .T. ) ;
#36927 = ADVANCED_FACE ( 'NONE', ( #24965 ), #32051, .T. ) ;
#36928 = ADVANCED_FACE ( 'NONE', ( #45213 ), #9199, .T. ) ;
#36929 = DIRECTION ( 'NONE',  ( 0.000000000000000000, 0.8229838658936556861, -0.5680647467311569221 ) ) ;
#36930 = DIRECTION ( 'NONE',  ( -0.5085311186492273983, 0.000000000000000000, 0.8610436117673514467 ) ) ;
#36931 = EDGE_LOOP ( 'NONE', ( #9780, #28556, #20811, #18611 ) ) ;
#36932 = ORIENTED_EDGE ( 'NONE', *, *, #28552, .F. ) ;
#36933 = EDGE_CURVE ( 'NONE', #35575, #27476, #50293, .T. ) ;
#36934 = ORIENTED_EDGE ( 'NONE', *, *, #18127, .T. ) ;
#36935 = DIRECTION ( 'NONE',  ( 0.9266896074318370369, 0.000000000000000000, -0.3758275821142292306 ) ) ;
#36936 = PLANE ( 'NONE',  #10087 ) ;
#36937 = DIRECTION ( 'NONE',  ( 5.399917434947259359E-17, 1.000000000000000000, -0.000000000000000000 ) ) ;
#36938 = FACE_BOUND ( 'NONE', #36696, .T. ) ;
#36939 = DIRECTION ( 'NONE',  ( 0.000000000000000000, -0.8854560256532062468, 0.4647231720437755564 ) ) ;
#36940 = EDGE_LOOP ( 'NONE', ( #22930, #10416, #34975, #15593 ) ) ;
#36941 = AXIS2_PLACEMENT_3D ( 'NONE', #1708, #49291, #45096 ) ;
#36942 = AXIS2_PLACEMENT_3D ( 'NONE', #21669, #29786, #45586 ) ;
#36943 = ORIENTED_EDGE ( 'NONE', *, *, #7419, .T. ) ;
#36945 = ORIENTED_EDGE ( 'NONE', *, *, #48869, .F. ) ;
#36944 = CARTESIAN_POINT ( 'NONE',  ( 0.000000000000000000, -63.50000000000000000, -16.00000000000000000 ) ) ;
#36946 = ORIENTED_EDGE ( 'NONE', *, *, #48225, .F. ) ;
#36947 = ADVANCED_FACE ( 'NONE', ( #18379 ), #14431, .T. ) ;
#36948 = CARTESIAN_POINT ( 'NONE',  ( -172.4195137048758397, -175.3837268820161057, -3.844569333772413611 ) ) ;
#36949 = LINE ( 'NONE', #5160, #32512 ) ;
#36950 = EDGE_CURVE ( 'NONE', #51223, #5652, #1294, .T. ) ;
#36951 = LINE ( 'NONE', #32487, #24561 ) ;
#36952 = DIRECTION ( 'NONE',  ( 0.000000000000000000, -1.000000000000000000, 0.000000000000000000 ) ) ;
#36953 = ORIENTED_EDGE ( 'NONE', *, *, #45317, .F. ) ;
#36954 = PLANE ( 'NONE',  #45203 ) ;
#36955 = ORIENTED_EDGE ( 'NONE', *, *, #8275, .F. ) ;
#36956 = EDGE_CURVE ( 'NONE', #12493, #23734, #50441, .T. ) ;
#36957 = VERTEX_POINT ( 'NONE', #29933 ) ;
#36958 = CARTESIAN_POINT ( 'NONE',  ( -339.1964088526558498, -64.99044476834235695, 7.608018572112245970 ) ) ;
#36959 = VECTOR ( 'NONE', #4405, 1000.000000000000000 ) ;
#36960 = DIRECTION ( 'NONE',  ( -0.000000000000000000, 1.000000000000000000, -0.000000000000000000 ) ) ;
#36961 = CARTESIAN_POINT ( 'NONE',  ( -336.3521761649654422, -67.40061919120938683, 18.46045550523129819 ) ) ;
#36962 = DIRECTION ( 'NONE',  ( 0.000000000000000000, -0.000000000000000000, 1.000000000000000000 ) ) ;
#36963 = LINE ( 'NONE', #427, #1045 ) ;
#36964 = ORIENTED_EDGE ( 'NONE', *, *, #22414, .F. ) ;
#36965 = CARTESIAN_POINT ( 'NONE',  ( -145.4373324222573842, -189.7472609257535510, -78.89300572996837957 ) ) ;
#36966 = CYLINDRICAL_SURFACE ( 'NONE', #24883, 4.999999999999997335 ) ;
#36967 = LINE ( 'NONE', #28549, #6850 ) ;
#36968 = FACE_BOUND ( 'NONE', #41335, .T. ) ;
#36969 = ORIENTED_EDGE ( 'NONE', *, *, #51732, .F. ) ;
#36970 = DIRECTION ( 'NONE',  ( -0.000000000000000000, 1.000000000000000000, -0.000000000000000000 ) ) ;
#36971 = ORIENTED_EDGE ( 'NONE', *, *, #3848, .F. ) ;
#36972 = PLANE ( 'NONE',  #20240 ) ;
#36973 = ORIENTED_EDGE ( 'NONE', *, *, #40743, .T. ) ;
#36974 = DIRECTION ( 'NONE',  ( -0.7575112421616284619, 0.000000000000000000, 0.6528221181905119463 ) ) ;
#36975 = VERTEX_POINT ( 'NONE', #25473 ) ;
#36976 = VECTOR ( 'NONE', #37055, 1000.000000000000000 ) ;
#36977 = VECTOR ( 'NONE', #14550, 1000.000000000000227 ) ;
#36978 = FACE_OUTER_BOUND ( 'NONE', #51420, .T. ) ;
#36979 = FACE_OUTER_BOUND ( 'NONE', #11662, .T. ) ;
#36981 = ORIENTED_EDGE ( 'NONE', *, *, #22934, .F. ) ;
#36980 = DIRECTION ( 'NONE',  ( -1.000000000000000000, 0.000000000000000000, -0.000000000000000000 ) ) ;
#36982 = EDGE_CURVE ( 'NONE', #13514, #17674, #37295, .T. ) ;
#36983 = EDGE_CURVE ( 'NONE', #19289, #10180, #17353, .T. ) ;
#36984 = CARTESIAN_POINT ( 'NONE',  ( -132.6364218684650211, -183.6283474603465606, 92.42591454022807795 ) ) ;
#36985 = VERTEX_POINT ( 'NONE', #41230 ) ;
#36986 = ORIENTED_EDGE ( 'NONE', *, *, #34838, .F. ) ;
#36987 = VERTEX_POINT ( 'NONE', #37814 ) ;
#36988 = CARTESIAN_POINT ( 'NONE',  ( -30.00000000000000000, 0.000000000000000000, 30.00000000000000355 ) ) ;
#36989 = LINE ( 'NONE', #13857, #23478 ) ;
#36990 = VECTOR ( 'NONE', #29807, 1000.000000000000000 ) ;
#36991 = ORIENTED_EDGE ( 'NONE', *, *, #17167, .T. ) ;
#36992 = LINE ( 'NONE', #49083, #10813 ) ;
#36993 = DIRECTION ( 'NONE',  ( 0.000000000000000000, 0.000000000000000000, -1.000000000000000000 ) ) ;
#36994 = DIRECTION ( 'NONE',  ( -0.9960498426152158968, 0.000000000000000000, -0.08879589532294571153 ) ) ;
#36995 = PLANE ( 'NONE',  #10810 ) ;
#36996 = LINE ( 'NONE', #16251, #23103 ) ;
#36997 = VERTEX_POINT ( 'NONE', #41490 ) ;
#37000 = ORIENTED_EDGE ( 'NONE', *, *, #1739, .F. ) ;
#36999 = CARTESIAN_POINT ( 'NONE',  ( -330.4913330509368166, -123.5000000000000284, 0.000000000000000000 ) ) ;
#36998 = PLANE ( 'NONE',  #34904 ) ;
#37001 = ORIENTED_EDGE ( 'NONE', *, *, #20080, .F. ) ;
#37002 = ADVANCED_FACE ( 'NONE', ( #50188 ), #45457, .T. ) ;
#37003 = DIRECTION ( 'NONE',  ( 0.05924062789370748011, 0.000000000000000000, 0.9982437317643217956 ) ) ;
#37004 = ORIENTED_EDGE ( 'NONE', *, *, #38929, .T. ) ;
#37005 = CARTESIAN_POINT ( 'NONE',  ( -332.3517673607765914, -123.5000000000000284, 0.000000000000000000 ) ) ;
#37006 = ORIENTED_EDGE ( 'NONE', *, *, #17882, .T. ) ;
#37007 = CARTESIAN_POINT ( 'NONE',  ( -48.47912675150885065, -189.7472609257535510, 6.938893903907228378E-15 ) ) ;
#37008 = CARTESIAN_POINT ( 'NONE',  ( 0.000000000000000000, -167.6621341420952547, -39.12423683620669124 ) ) ;
#37009 = EDGE_LOOP ( 'NONE', ( #49709, #32576, #48943, #15977 ) ) ;
#37010 = DIRECTION ( 'NONE',  ( 1.000000000000000000, -0.000000000000000000, -0.000000000000000000 ) ) ;
#37011 = ORIENTED_EDGE ( 'NONE', *, *, #8357, .T. ) ;
#37012 = ADVANCED_FACE ( 'NONE', ( #22047 ), #17853, .T. ) ;
#37013 = AXIS2_PLACEMENT_3D ( 'NONE', #32299, #16285, #28362 ) ;
#37014 = ORIENTED_EDGE ( 'NONE', *, *, #27919, .F. ) ;
#37015 = DIRECTION ( 'NONE',  ( 0.9473263538541876194, 0.000000000000000000, 0.3202698538628486746 ) ) ;
#37016 = DIRECTION ( 'NONE',  ( 0.9027978299657477557, 0.000000000000000000, -0.4300652022765115712 ) ) ;
#37017 = CARTESIAN_POINT ( 'NONE',  ( -336.3521761649654422, -173.5513585866778214, -31.34948880313881503 ) ) ;
#37018 = PLANE ( 'NONE',  #39952 ) ;
#37019 = EDGE_LOOP ( 'NONE', ( #3530, #17939, #50280, #43449 ) ) ;
#37020 = LINE ( 'NONE', #44654, #4591 ) ;
#37021 = DIRECTION ( 'NONE',  ( 0.000000000000000000, 0.000000000000000000, -1.000000000000000000 ) ) ;
#37022 = CARTESIAN_POINT ( 'NONE',  ( -339.1964088526558498, -96.06030588028492900, -53.35787839313396574 ) ) ;
#37023 = DIRECTION ( 'NONE',  ( 1.043714542225393065E-14, -0.9709418174260511236, 0.2393156642875615969 ) ) ;
#37024 = DIRECTION ( 'NONE',  ( 0.000000000000000000, 0.000000000000000000, 1.000000000000000000 ) ) ;
#37025 = LINE ( 'NONE', #32292, #44749 ) ;
#37026 = VERTEX_POINT ( 'NONE', #25737 ) ;
#37027 = AXIS2_PLACEMENT_3D ( 'NONE', #44488, #20300, #36331 ) ;
#37028 = LINE ( 'NONE', #8401, #41172 ) ;
#37029 = CARTESIAN_POINT ( 'NONE',  ( -332.3517673607765914, -68.91285928486892942, -22.44790492310182017 ) ) ;
#37030 = ORIENTED_EDGE ( 'NONE', *, *, #113, .F. ) ;
#37031 = VERTEX_POINT ( 'NONE', #33367 ) ;
#37032 = EDGE_LOOP ( 'NONE', ( #26687, #41121, #5660, #28763 ) ) ;
#37033 = EDGE_CURVE ( 'NONE', #50002, #14153, #1565, .T. ) ;
#37034 = CARTESIAN_POINT ( 'NONE',  ( 76.37123734610607073, -183.6283474603465606, 6.114457023561876703 ) ) ;
#37035 = PLANE ( 'NONE',  #3544 ) ;
#37036 = LINE ( 'NONE', #32835, #13645 ) ;
#37037 = CARTESIAN_POINT ( 'NONE',  ( 2.449293598294706119E-15, -63.50000000000000000, -20.00000000000000000 ) ) ;
#37038 = AXIS2_PLACEMENT_3D ( 'NONE', #31664, #12200, #11422 ) ;
#37039 = ORIENTED_EDGE ( 'NONE', *, *, #2683, .T. ) ;
#37040 = DIRECTION ( 'NONE',  ( 0.000000000000000000, 0.7485107481711024136, 0.6631226582407937498 ) ) ;
#37041 = EDGE_CURVE ( 'NONE', #8674, #33846, #10000, .T. ) ;
#37042 = CIRCLE ( 'NONE', #2647, 125.0000000000000000 ) ;
#37043 = FACE_OUTER_BOUND ( 'NONE', #10710, .T. ) ;
#37044 = ORIENTED_EDGE ( 'NONE', *, *, #7346, .F. ) ;
#37045 = AXIS2_PLACEMENT_3D ( 'NONE', #36183, #21205, #44076 ) ;
#37046 = DIRECTION ( 'NONE',  ( 0.000000000000000000, 0.5664407118577555744, -0.8241024935953531472 ) ) ;
#37047 = ORIENTED_EDGE ( 'NONE', *, *, #30108, .T. ) ;
#37048 = CARTESIAN_POINT ( 'NONE',  ( -58.29063029684667185, -177.1207230881787780, 124.6143426664034877 ) ) ;
#37049 = ADVANCED_FACE ( 'NONE', ( #49411 ), #22301, .T. ) ;
#37050 = ORIENTED_EDGE ( 'NONE', *, *, #45549, .T. ) ;
#37051 = CARTESIAN_POINT ( 'NONE',  ( -336.3521761649654422, -140.1754235130667610, -56.65561927338005432 ) ) ;
#37052 = EDGE_CURVE ( 'NONE', #44562, #15649, #49911, .T. ) ;
#37053 = CIRCLE ( 'NONE', #27815, 125.0000000000000000 ) ;
#37054 = PLANE ( 'NONE',  #50334 ) ;
#37055 = DIRECTION ( 'NONE',  ( -1.000000000000000000, -9.758900497077161467E-15, -3.701062773504848780E-15 ) ) ;
#37058 = ORIENTED_EDGE ( 'NONE', *, *, #49430, .F. ) ;
#37057 = LINE ( 'NONE', #48905, #2324 ) ;
#37056 = CARTESIAN_POINT ( 'NONE',  ( -0.5847574683125812411, 58.11708756977395041, -16.46759551110862674 ) ) ;
#37059 = EDGE_CURVE ( 'NONE', #30895, #39858, #45714, .T. ) ;
#37060 = DIRECTION ( 'NONE',  ( 0.000000000000000000, -1.000000000000000000, 0.000000000000000000 ) ) ;
#37061 = ORIENTED_EDGE ( 'NONE', *, *, #9116, .T. ) ;
#37062 = LINE ( 'NONE', #28910, #30575 ) ;
#37063 = PLANE ( 'NONE',  #45947 ) ;
#37064 = EDGE_LOOP ( 'NONE', ( #7251, #20207, #33591, #28517 ) ) ;
#37065 = CARTESIAN_POINT ( 'NONE',  ( -330.4913330509368166, -102.1108035431478811, -54.98865587491830809 ) ) ;
#37067 = CARTESIAN_POINT ( 'NONE',  ( -50.89116676070555911, -177.1207230881787780, 124.9767260852757147 ) ) ;
#37066 = CARTESIAN_POINT ( 'NONE',  ( 52.75081385575904136, -189.7472609257535510, 71.61357856150601719 ) ) ;
#37068 = ORIENTED_EDGE ( 'NONE', *, *, #5627, .T. ) ;
#37069 = PLANE ( 'NONE',  #8093 ) ;
#37070 = DIRECTION ( 'NONE',  ( -0.000000000000000000, 1.000000000000000000, -0.000000000000000000 ) ) ;
#37071 = CARTESIAN_POINT ( 'NONE',  ( -161.4019114581580823, -175.3837268820161057, 53.60452120946281696 ) ) ;
#37072 = ORIENTED_EDGE ( 'NONE', *, *, #9568, .F. ) ;
#37073 = DIRECTION ( 'NONE',  ( 0.000000000000000000, 0.000000000000000000, -1.000000000000000000 ) ) ;
#37074 = CARTESIAN_POINT ( 'NONE',  ( -336.3521761649654422, -110.9652333097088217, -57.67619951860654481 ) ) ;
#37075 = DIRECTION ( 'NONE',  ( 0.000000000000000000, -1.000000000000000000, 0.000000000000000000 ) ) ;
#37076 = AXIS2_PLACEMENT_3D ( 'NONE', #29443, #45495, #49692 ) ;
#37077 = PLANE ( 'NONE',  #20683 ) ;
#37078 = ORIENTED_EDGE ( 'NONE', *, *, #7396, .F. ) ;
#37079 = VECTOR ( 'NONE', #30419, 1000.000000000000114 ) ;
#37080 = LINE ( 'NONE', #17130, #21259 ) ;
#37081 = DIRECTION ( 'NONE',  ( 0.8858462335218260097, 0.000000000000000000, 0.4639789333096864810 ) ) ;
#37082 = AXIS2_PLACEMENT_3D ( 'NONE', #45774, #26564, #30001 ) ;
#37083 = PLANE ( 'NONE',  #13695 ) ;
#37084 = ORIENTED_EDGE ( 'NONE', *, *, #21867, .F. ) ;
#37085 = LINE ( 'NONE', #29209, #40739 ) ;
#37086 = LINE ( 'NONE', #12647, #46253 ) ;
#37087 = LINE ( 'NONE', #41036, #20166 ) ;
#37088 = EDGE_CURVE ( 'NONE', #19748, #21876, #28424, .T. ) ;
#37089 = CARTESIAN_POINT ( 'NONE',  ( -49.35486169370448550, -175.3837268820161057, -0.4827922027307481878 ) ) ;
#37090 = CIRCLE ( 'NONE', #50540, 125.0000000000000000 ) ;
#37091 = LINE ( 'NONE', #44207, #5310 ) ;
#37092 = EDGE_CURVE ( 'NONE', #1505, #20926, #46240, .T. ) ;
#37093 = CIRCLE ( 'NONE', #14457, 125.0000000000000000 ) ;
#37094 = VECTOR ( 'NONE', #50073, 1000.000000000000114 ) ;
#37095 = DIRECTION ( 'NONE',  ( -0.000000000000000000, 1.000000000000000000, -0.000000000000000000 ) ) ;
#37096 = DIRECTION ( 'NONE',  ( -0.000000000000000000, 1.000000000000000000, -0.000000000000000000 ) ) ;
#37098 = EDGE_LOOP ( 'NONE', ( #27568, #49235, #18, #11394 ) ) ;
#37097 = DIRECTION ( 'NONE',  ( 0.000000000000000000, 0.1205366802553164696, -0.9927088740980548609 ) ) ;
#37099 = ORIENTED_EDGE ( 'NONE', *, *, #12168, .F. ) ;
#37100 = DIRECTION ( 'NONE',  ( 0.9151456172430153524, 0.000000000000000000, 0.4031234292879792847 ) ) ;
#37101 = ADVANCED_FACE ( 'NONE', ( #13646 ), #6282, .F. ) ;
#37102 = ADVANCED_FACE ( 'NONE', ( #18869 ), #23351, .T. ) ;
#37103 = EDGE_CURVE ( 'NONE', #4967, #2171, #15204, .T. ) ;
#37104 = LINE ( 'NONE', #17149, #38056 ) ;
#37106 = ORIENTED_EDGE ( 'NONE', *, *, #22659, .F. ) ;
#37105 = CARTESIAN_POINT ( 'NONE',  ( -330.4913330509368166, -101.7569374291128526, -55.92172413327835301 ) ) ;
#37107 = ORIENTED_EDGE ( 'NONE', *, *, #29452, .T. ) ;
#37108 = ADVANCED_FACE ( 'NONE', ( #39362 ), #14957, .T. ) ;
#37109 = ORIENTED_EDGE ( 'NONE', *, *, #22993, .F. ) ;
#37110 = PLANE ( 'NONE',  #30889 ) ;
#37111 = AXIS2_PLACEMENT_3D ( 'NONE', #49887, #33341, #28858 ) ;
#37112 = CARTESIAN_POINT ( 'NONE',  ( -48.41988612361515010, -183.6283474603465606, 0.9982437317643287900 ) ) ;
#37113 = CARTESIAN_POINT ( 'NONE',  ( -105.7090724259147976, -189.7472609257535510, 111.1293539894142839 ) ) ;
#37114 = ORIENTED_EDGE ( 'NONE', *, *, #28073, .T. ) ;
#37115 = VECTOR ( 'NONE', #5320, 1000.000000000000000 ) ;
#37116 = DIRECTION ( 'NONE',  ( -0.05924062789371441901, 0.000000000000000000, 0.9982437317643214625 ) ) ;
#37118 = ORIENTED_EDGE ( 'NONE', *, *, #2401, .F. ) ;
#37117 = CARTESIAN_POINT ( 'NONE',  ( -332.3517673607765914, -121.8677111499054320, 59.00000000000001421 ) ) ;
#37119 = DIRECTION ( 'NONE',  ( -1.000000000000000000, -0.000000000000000000, 0.000000000000000000 ) ) ;
#37120 = ORIENTED_EDGE ( 'NONE', *, *, #38093, .T. ) ;
#37121 = FACE_OUTER_BOUND ( 'NONE', #18625, .T. ) ;
#37122 = ORIENTED_EDGE ( 'NONE', *, *, #51347, .F. ) ;
#37123 = PLANE ( 'NONE',  #16549 ) ;
#37124 = FACE_OUTER_BOUND ( 'NONE', #520, .T. ) ;
#37125 = CARTESIAN_POINT ( 'NONE',  ( 44.30815888362531041, -189.7472609257535510, 83.75869879877569701 ) ) ;
#37126 = AXIS2_PLACEMENT_3D ( 'NONE', #7391, #23415, #39170 ) ;
#37127 = AXIS2_PLACEMENT_3D ( 'NONE', #47173, #11148, #27173 ) ;
#37128 = VERTEX_POINT ( 'NONE', #7572 ) ;
#37129 = VECTOR ( 'NONE', #34120, 1000.000000000000227 ) ;
#37130 = ORIENTED_EDGE ( 'NONE', *, *, #45143, .F. ) ;
#37131 = AXIS2_PLACEMENT_3D ( 'NONE', #11576, #15261, #7388 ) ;
#37132 = CARTESIAN_POINT ( 'NONE',  ( 63.82222181224018698, -189.7472609257535510, 52.57768177182521896 ) ) ;
#37133 = CARTESIAN_POINT ( 'NONE',  ( 68.72094416275764672, -189.7472609257535510, -40.49875167738976955 ) ) ;
#37134 = ORIENTED_EDGE ( 'NONE', *, *, #10525, .F. ) ;
#37135 = CARTESIAN_POINT ( 'NONE',  ( 18.82962626094778003, -193.5000000000000000, 104.1428419024404519 ) ) ;
#37136 = CARTESIAN_POINT ( 'NONE',  ( -48.07600332222088468, -189.7472609257535510, 0.9151456172430280089 ) ) ;
#37137 = ORIENTED_EDGE ( 'NONE', *, *, #35249, .T. ) ;
#37138 = DIRECTION ( 'NONE',  ( 0.000000000000000000, -0.6631226582408016323, -0.7485107481710953081 ) ) ;
#37139 = CLOSED_SHELL ( 'NONE', ( #20501, #32710, #10608, #50897, #37645, #11056, #38169, #50549 ) ) ;
#37140 = DIRECTION ( 'NONE',  ( -0.000000000000000000, -0.9709418174260526779, -0.2393156642875547968 ) ) ;
#37141 = ORIENTED_EDGE ( 'NONE', *, *, #45998, .T. ) ;
#37142 = CARTESIAN_POINT ( 'NONE',  ( -47.60339180931321579, -177.1207230881787780, 0.4827922027307559594 ) ) ;
#37143 = EDGE_LOOP ( 'NONE', ( #29084, #4087, #31325, #31145 ) ) ;
#37144 = DIRECTION ( 'NONE',  ( 0.000000000000000000, -0.000000000000000000, 1.000000000000000000 ) ) ;
#37145 = LINE ( 'NONE', #12455, #6786 ) ;
#37146 = ORIENTED_EDGE ( 'NONE', *, *, #31701, .T. ) ;
#37147 = AXIS2_PLACEMENT_3D ( 'NONE', #4134, #11478, #166 ) ;
#37148 = ADVANCED_FACE ( 'NONE', ( #39093 ), #30966, .T. ) ;
#37149 = CARTESIAN_POINT ( 'NONE',  ( -48.47912675150885065, -183.6283474603465606, 6.938893903907228378E-15 ) ) ;
#37150 = EDGE_CURVE ( 'NONE', #28257, #39885, #50686, .T. ) ;
#37151 = DIRECTION ( 'NONE',  ( 0.000000000000000000, 0.000000000000000000, -1.000000000000000000 ) ) ;
#37152 = DIRECTION ( 'NONE',  ( -0.000000000000000000, 0.000000000000000000, 1.000000000000000000 ) ) ;
#37153 = EDGE_CURVE ( 'NONE', #2629, #41896, #35673, .T. ) ;
#37154 = FACE_OUTER_BOUND ( 'NONE', #47138, .T. ) ;
#37155 = VECTOR ( 'NONE', #4470, 1000.000000000000114 ) ;
#37156 = ORIENTED_EDGE ( 'NONE', *, *, #47689, .T. ) ;
#37157 = DIRECTION ( 'NONE',  ( 0.000000000000000000, 1.000000000000000000, 0.000000000000000000 ) ) ;
#37158 = ORIENTED_EDGE ( 'NONE', *, *, #9191, .F. ) ;
#37159 = ORIENTED_EDGE ( 'NONE', *, *, #46441, .T. ) ;
#37160 = FACE_OUTER_BOUND ( 'NONE', #42420, .T. ) ;
#37162 = EDGE_LOOP ( 'NONE', ( #16671, #37661, #36867, #17891 ) ) ;
#37161 = CYLINDRICAL_SURFACE ( 'NONE', #51447, 125.0000000000000000 ) ;
#37163 = ADVANCED_FACE ( 'NONE', ( #47010 ), #27012, .T. ) ;
#37164 = EDGE_LOOP ( 'NONE', ( #23918, #39286, #48363, #33293 ) ) ;
#37165 = CARTESIAN_POINT ( 'NONE',  ( 0.000000000000000000, -63.50000000000000000, 0.000000000000000000 ) ) ;
#37166 = EDGE_CURVE ( 'NONE', #32221, #34468, #23082, .T. ) ;
#37167 = CIRCLE ( 'NONE', #17902, 4.000000000000003553 ) ;
#37168 = CIRCLE ( 'NONE', #29621, 60.00000000000000000 ) ;
#37169 = EDGE_CURVE ( 'NONE', #14767, #51107, #11671, .T. ) ;
#37170 = CARTESIAN_POINT ( 'NONE',  ( -339.1964088526558498, -66.09477493971894546, 13.63415328425207917 ) ) ;
#37171 = CARTESIAN_POINT ( 'NONE',  ( 73.66680038934278230, -175.3837268820161057, -26.55884942729568365 ) ) ;
#37172 = VECTOR ( 'NONE', #49135, 1000.000000000000000 ) ;
#37173 = AXIS2_PLACEMENT_3D ( 'NONE', #44902, #1532, #9166 ) ;
#37174 = ORIENTED_EDGE ( 'NONE', *, *, #41769, .T. ) ;
#37175 = EDGE_CURVE ( 'NONE', #29243, #51040, #43052, .T. ) ;
#37176 = DIRECTION ( 'NONE',  ( -0.000000000000000000, 0.1205366802553199113, -0.9927088740980544168 ) ) ;
#37177 = ORIENTED_EDGE ( 'NONE', *, *, #15329, .F. ) ;
#37178 = CYLINDRICAL_SURFACE ( 'NONE', #46815, 125.0000000000000000 ) ;
#37179 = DIRECTION ( 'NONE',  ( 0.4106364553079953628, -0.8746197071393964073, 0.2577170336929271999 ) ) ;
#37180 = EDGE_CURVE ( 'NONE', #51893, #15715, #27269, .T. ) ;
#37181 = CARTESIAN_POINT ( 'NONE',  ( -305.0000000000000568, -168.0775241366801254, -40.16023333900968595 ) ) ;
#37182 = FACE_OUTER_BOUND ( 'NONE', #29238, .T. ) ;
#37183 = VERTEX_POINT ( 'NONE', #35413 ) ;
#37184 = EDGE_LOOP ( 'NONE', ( #33308, #16982, #50712, #29546 ) ) ;
#37185 = ORIENTED_EDGE ( 'NONE', *, *, #27223, .F. ) ;
#37186 = DIRECTION ( 'NONE',  ( 1.043714542225393381E-14, 0.7485107481711069655, 0.6631226582407885317 ) ) ;
#37187 = FACE_OUTER_BOUND ( 'NONE', #9332, .T. ) ;
#37188 = FACE_BOUND ( 'NONE', #46140, .T. ) ;
#37189 = LINE ( 'NONE', #37716, #4571 ) ;
#37190 = CIRCLE ( 'NONE', #30470, 15.00000000000000000 ) ;
#37191 = ORIENTED_EDGE ( 'NONE', *, *, #21809, .T. ) ;
#37192 = ADVANCED_FACE ( 'NONE', ( #35163 ), #38592, .T. ) ;
#37193 = CIRCLE ( 'NONE', #36325, 15.00000000000000000 ) ;
#37194 = EDGE_LOOP ( 'NONE', ( #19656, #14621, #12369, #29003 ) ) ;
#37196 = ORIENTED_EDGE ( 'NONE', *, *, #37153, .T. ) ;
#37195 = DIRECTION ( 'NONE',  ( 0.000000000000000000, 0.000000000000000000, -1.000000000000000000 ) ) ;
#37197 = EDGE_LOOP ( 'NONE', ( #45960, #20228, #35444, #22149 ) ) ;
#37198 = LINE ( 'NONE', #1186, #23318 ) ;
#37199 = CARTESIAN_POINT ( 'NONE',  ( -85.77912150413021664, -189.7472609257535510, -119.3051146910911768 ) ) ;
#37200 = PLANE ( 'NONE',  #9533 ) ;
#37201 = LINE ( 'NONE', #40609, #46081 ) ;
#37202 = EDGE_LOOP ( 'NONE', ( #13219, #40935, #41435, #22960 ) ) ;
#37203 = DIRECTION ( 'NONE',  ( 0.000000000000000000, 1.000000000000000000, -0.000000000000000000 ) ) ;
#37204 = VECTOR ( 'NONE', #27227, 1000.000000000000000 ) ;
#37205 = ORIENTED_EDGE ( 'NONE', *, *, #23780, .F. ) ;
#37206 = EDGE_CURVE ( 'NONE', #21292, #16634, #15736, .T. ) ;
#37207 = ORIENTED_EDGE ( 'NONE', *, *, #428, .F. ) ;
#37208 = FACE_OUTER_BOUND ( 'NONE', #28747, .T. ) ;
#37209 = AXIS2_PLACEMENT_3D ( 'NONE', #49041, #12755, #9358 ) ;
#37210 = DIRECTION ( 'NONE',  ( 0.000000000000000000, 0.000000000000000000, 1.000000000000000000 ) ) ;
#37211 = EDGE_LOOP ( 'NONE', ( #40234, #13321, #13372, #11941 ) ) ;
#37212 = EDGE_CURVE ( 'NONE', #13145, #10439, #51466, .T. ) ;
#37213 = ADVANCED_FACE ( 'NONE', ( #31470 ), #34641, .T. ) ;
#37214 = PLANE ( 'NONE',  #23145 ) ;
#37215 = EDGE_CURVE ( 'NONE', #39568, #43845, #6662, .T. ) ;
#37216 = DIRECTION ( 'NONE',  ( -0.000000000000000000, -0.5680647467311596976, -0.8229838658936536877 ) ) ;
#37217 = LINE ( 'NONE', #1207, #11951 ) ;
#37218 = ADVANCED_FACE ( 'NONE', ( #36978 ), #39859, .T. ) ;
#37219 = CIRCLE ( 'NONE', #258, 125.0000000000000000 ) ;
#37220 = CARTESIAN_POINT ( 'NONE',  ( -339.1964088526558498, -68.51134412508150717, 21.38919645685156112 ) ) ;
#37221 = CARTESIAN_POINT ( 'NONE',  ( -336.3521761649654422, -85.72124494520284088, -46.61293454085073051 ) ) ;
#37222 = ADVANCED_FACE ( 'NONE', ( #19914 ), #44865, .T. ) ;
#37223 = DIRECTION ( 'NONE',  ( -0.000000000000000000, 1.000000000000000000, -0.000000000000000000 ) ) ;
#37224 = DIRECTION ( 'NONE',  ( -0.000000000000000000, 1.000000000000000000, -0.000000000000000000 ) ) ;
#37225 = EDGE_LOOP ( 'NONE', ( #4554, #41360, #44153, #29129 ) ) ;
#37226 = EDGE_CURVE ( 'NONE', #29243, #44016, #35947, .T. ) ;
#37227 = DIRECTION ( 'NONE',  ( -0.6965510290630033685, 0.000000000000000000, 0.7175072570443249420 ) ) ;
#37228 = ORIENTED_EDGE ( 'NONE', *, *, #13687, .F. ) ;
#37229 = VECTOR ( 'NONE', #32235, 1000.000000000000000 ) ;
#37230 = CARTESIAN_POINT ( 'NONE',  ( -111.8989814360438828, -193.5000000000000000, -107.7168604805787027 ) ) ;
#37231 = ORIENTED_EDGE ( 'NONE', *, *, #36096, .F. ) ;
#37232 = DIRECTION ( 'NONE',  ( 0.000000000000000000, 0.7485107481710977506, -0.6631226582407989678 ) ) ;
#37233 = EDGE_CURVE ( 'NONE', #8838, #13900, #26784, .T. ) ;
#37234 = ORIENTED_EDGE ( 'NONE', *, *, #31571, .T. ) ;
#37235 = CIRCLE ( 'NONE', #25490, 125.0000000000000000 ) ;
#37236 = EDGE_CURVE ( 'NONE', #23075, #41331, #10852, .T. ) ;
#37237 = LINE ( 'NONE', #29863, #25968 ) ;
#37238 = EDGE_CURVE ( 'NONE', #3919, #22737, #972, .T. ) ;
#37239 = CARTESIAN_POINT ( 'NONE',  ( -339.1964088526558498, -137.1341532842531876, -57.40522506028080585 ) ) ;
#37241 = ORIENTED_EDGE ( 'NONE', *, *, #8275, .T. ) ;
#37240 = CARTESIAN_POINT ( 'NONE',  ( -365.0000000000001137, -78.50000000000002842, 10.00000000000000711 ) ) ;
#37242 = EDGE_CURVE ( 'NONE', #3706, #33563, #8593, .T. ) ;
#37244 = AXIS2_PLACEMENT_3D ( 'NONE', #22131, #22390, #45535 ) ;
#37243 = PLANE ( 'NONE',  #10099 ) ;
#37245 = ORIENTED_EDGE ( 'NONE', *, *, #21094, .T. ) ;
#37246 = ORIENTED_EDGE ( 'NONE', *, *, #1812, .F. ) ;
#37247 = EDGE_CURVE ( 'NONE', #16129, #37529, #15980, .T. ) ;
#37248 = EDGE_LOOP ( 'NONE', ( #14523, #34959, #21808, #51282 ) ) ;
#37249 = DIRECTION ( 'NONE',  ( 0.6528221181905227155, 0.000000000000000000, -0.7575112421616191360 ) ) ;
#37250 = CARTESIAN_POINT ( 'NONE',  ( -147.6585554144535593, -183.6283474603465606, 76.08180419845380982 ) ) ;
#37251 = VERTEX_POINT ( 'NONE', #28310 ) ;
#37252 = DIRECTION ( 'NONE',  ( 0.000000000000000000, 0.2393156642875516049, -0.9709418174260534551 ) ) ;
#37253 = FACE_OUTER_BOUND ( 'NONE', #32316, .T. ) ;
#37254 = ORIENTED_EDGE ( 'NONE', *, *, #20543, .F. ) ;
#37255 = ADVANCED_FACE ( 'NONE', ( #11758 ), #8085, .T. ) ;
#37256 = DIRECTION ( 'NONE',  ( 0.9027978299657477557, 0.000000000000000000, -0.4300652022765115712 ) ) ;
#37257 = DIRECTION ( 'NONE',  ( 0.000000000000000000, -0.6631226582407989678, -0.7485107481710977506 ) ) ;
#37258 = ORIENTED_EDGE ( 'NONE', *, *, #12487, .F. ) ;
#37261 = ORIENTED_EDGE ( 'NONE', *, *, #25384, .T. ) ;
#37260 = CARTESIAN_POINT ( 'NONE',  ( -47.55243714407701816, -175.3837268820161057, -0.3758275821142288420 ) ) ;
#37259 = CARTESIAN_POINT ( 'NONE',  ( -305.0000000000000568, -65.36517161715278235, -14.84391218300951643 ) ) ;
#37262 = ORIENTED_EDGE ( 'NONE', *, *, #9837, .T. ) ;
#37263 = ORIENTED_EDGE ( 'NONE', *, *, #17605, .T. ) ;
#37264 = LINE ( 'NONE', #44899, #40694 ) ;
#37265 = AXIS2_PLACEMENT_3D ( 'NONE', #40020, #16390, #4045 ) ;
#37266 = ORIENTED_EDGE ( 'NONE', *, *, #8611, .T. ) ;
#37267 = VECTOR ( 'NONE', #36232, 1000.000000000000000 ) ;
#37268 = CARTESIAN_POINT ( 'NONE',  ( -101.9736325116273576, -193.5000000000000000, 112.9749434763330811 ) ) ;
#37269 = CARTESIAN_POINT ( 'NONE',  ( -339.1964088526558498, -66.33409060400673241, -14.60509510167901404 ) ) ;
#37270 = ORIENTED_EDGE ( 'NONE', *, *, #25723, .F. ) ;
#37271 = DIRECTION ( 'NONE',  ( 0.000000000000000000, -0.000000000000000000, -1.000000000000000000 ) ) ;
#37272 = EDGE_LOOP ( 'NONE', ( #15197, #14719, #33880, #25826 ) ) ;
#37273 = VECTOR ( 'NONE', #952, 1000.000000000000000 ) ;
#37274 = ORIENTED_EDGE ( 'NONE', *, *, #23194, .T. ) ;
#37275 = CARTESIAN_POINT ( 'NONE',  ( -339.1964088526558498, -123.5000000000000284, 0.000000000000000000 ) ) ;
#37276 = CARTESIAN_POINT ( 'NONE',  ( -123.5870580700902366, -189.7472609257535510, -98.66508442481458019 ) ) ;
#37277 = CARTESIAN_POINT ( 'NONE',  ( -339.1964088526558498, -71.02573290043878274, -26.97593913775585506 ) ) ;
#37278 = FACE_OUTER_BOUND ( 'NONE', #29568, .T. ) ;
#37279 = VERTEX_POINT ( 'NONE', #23849 ) ;
#37280 = DIRECTION ( 'NONE',  ( 0.000000000000000000, 0.000000000000000000, 1.000000000000000000 ) ) ;
#37281 = EDGE_CURVE ( 'NONE', #4055, #20290, #442, .T. ) ;
#37282 = ADVANCED_FACE ( 'NONE', ( #27783 ), #32519, .T. ) ;
#37283 = APPLICATION_PROTOCOL_DEFINITION ( 'draft international standard', 'automotive_design', 1998, #20613 ) ;
#37284 = CARTESIAN_POINT ( 'NONE',  ( -336.3521761649654422, -64.73342574900661361, 5.491276508483657892 ) ) ;
#37285 = CARTESIAN_POINT ( 'NONE',  ( 4.558749771216725755, -183.6283474603465606, -112.0852863853379233 ) ) ;
#37286 = DIRECTION ( 'NONE',  ( 0.000000000000000000, 0.5680647467311510379, -0.8229838658936596829 ) ) ;
#37287 = FACE_OUTER_BOUND ( 'NONE', #27804, .T. ) ;
#37288 = ADVANCED_FACE ( 'NONE', ( #7820 ), #4157, .T. ) ;
#37289 = CARTESIAN_POINT ( 'NONE',  ( -332.3517673607765914, -65.24746378767824240, -9.724760635741734660 ) ) ;
#37290 = VERTEX_POINT ( 'NONE', #187 ) ;
#37291 = CARTESIAN_POINT ( 'NONE',  ( -52.47502265695602119, -177.1207230881787780, -124.9361149384469485 ) ) ;
#37292 = ORIENTED_EDGE ( 'NONE', *, *, #15006, .F. ) ;
#37293 = CARTESIAN_POINT ( 'NONE',  ( -332.3517673607765914, -181.7525362123217292, 9.724760635742144999 ) ) ;
#37294 = ORIENTED_EDGE ( 'NONE', *, *, #51649, .T. ) ;
#37295 = LINE ( 'NONE', #26236, #13369 ) ;
#37296 = PLANE ( 'NONE',  #24507 ) ;
#37297 = EDGE_CURVE ( 'NONE', #30367, #37834, #16235, .T. ) ;
#37298 = DIRECTION ( 'NONE',  ( 0.000000000000000000, 0.000000000000000000, -1.000000000000000000 ) ) ;
#37299 = DIRECTION ( 'NONE',  ( 0.000000000000000000, 1.000000000000000000, 0.000000000000000000 ) ) ;
#37300 = CIRCLE ( 'NONE', #49084, 125.0000000000000000 ) ;
#37301 = VERTEX_POINT ( 'NONE', #48566 ) ;
#37302 = AXIS2_PLACEMENT_3D ( 'NONE', #51096, #27136, #35286 ) ;
#37303 = PLANE ( 'NONE',  #19078 ) ;
#37304 = CARTESIAN_POINT ( 'NONE',  ( 46.00000000000000711, -57.64213562373095101, -46.00000000000000000 ) ) ;
#37305 = VERTEX_POINT ( 'NONE', #12546 ) ;
#37306 = CIRCLE ( 'NONE', #32261, 125.0000000000000000 ) ;
#37307 = EDGE_CURVE ( 'NONE', #5856, #13819, #41910, .T. ) ;
#37308 = CARTESIAN_POINT ( 'NONE',  ( 60.00000000000001421, 0.000000000000000000, -60.00000000000000711 ) ) ;
#37309 = ORIENTED_EDGE ( 'NONE', *, *, #5373, .T. ) ;
#37310 = CARTESIAN_POINT ( 'NONE',  ( -47.47956591500005885, -189.7472609257535510, 0.02963332782257025594 ) ) ;
#37311 = ORIENTED_EDGE ( 'NONE', *, *, #17002, .T. ) ;
#37312 = CARTESIAN_POINT ( 'NONE',  ( 50.08808042611238420, -183.6283474603465606, -76.87330921200083367 ) ) ;
#37313 = VERTEX_POINT ( 'NONE', #36725 ) ;
#37314 = AXIS2_PLACEMENT_3D ( 'NONE', #40335, #35900, #31430 ) ;
#37315 = CARTESIAN_POINT ( 'NONE',  ( -87.28630321566649286, -183.6283474603465606, 118.8234112238818341 ) ) ;
#37316 = PRODUCT_DEFINITION_SHAPE ( 'NONE', 'NONE',  #52044 ) ;
#37317 = DIRECTION ( 'NONE',  ( -0.2920567706369628924, 0.000000000000000000, -0.9564009842765264224 ) ) ;
#37318 = VERTEX_POINT ( 'NONE', #16770 ) ;
#37321 = ORIENTED_EDGE ( 'NONE', *, *, #40974, .T. ) ;
#37320 = LINE ( 'NONE', #9998, #49102 ) ;
#37319 = CARTESIAN_POINT ( 'NONE',  ( -330.4913330509368166, -162.2499814621216672, -44.49369547121515467 ) ) ;
#37322 = CARTESIAN_POINT ( 'NONE',  ( -336.3521761649654422, -152.3639871485048900, -51.48334306143194539 ) ) ;
#37323 = ORIENTED_EDGE ( 'NONE', *, *, #35138, .F. ) ;
#37324 = CARTESIAN_POINT ( 'NONE',  ( -173.3294908491238004, -177.1207230881787780, -6.114457023560984972 ) ) ;
#37325 = VERTEX_POINT ( 'NONE', #32779 ) ;
#37326 = CARTESIAN_POINT ( 'NONE',  ( -70.42295845586433245, -175.3837268820161057, -123.0587999703024877 ) ) ;
#37329 = ORIENTED_EDGE ( 'NONE', *, *, #3766, .T. ) ;
#37328 = DIRECTION ( 'NONE',  ( -0.000000000000000000, 1.000000000000000000, -0.000000000000000000 ) ) ;
#37327 = DIRECTION ( 'NONE',  ( 1.000000000000000000, -0.000000000000000000, -0.000000000000000000 ) ) ;
#37330 = ORIENTED_EDGE ( 'NONE', *, *, #861, .T. ) ;
#37331 = DIRECTION ( 'NONE',  ( 0.000000000000000000, -0.000000000000000000, -1.000000000000000000 ) ) ;
#37332 = FACE_OUTER_BOUND ( 'NONE', #41031, .T. ) ;
#37333 = DIRECTION ( 'NONE',  ( -1.000000000000000000, -0.000000000000000000, -0.000000000000000000 ) ) ;
#37334 = ORIENTED_EDGE ( 'NONE', *, *, #28564, .T. ) ;
#37335 = CARTESIAN_POINT ( 'NONE',  ( -171.1451123608488274, -175.3837268820161057, 18.13990644964088972 ) ) ;
#37336 = CARTESIAN_POINT ( 'NONE',  ( -47.66663987350317910, -175.3837268820161057, 0.5829794791144832233 ) ) ;
#37337 = FACE_OUTER_BOUND ( 'NONE', #13587, .T. ) ;
#37338 = VECTOR ( 'NONE', #49105, 999.9999999999998863 ) ;
#37339 = CARTESIAN_POINT ( 'NONE',  ( -173.4724443937511467, -177.1207230881787780, 1.292495564989519785 ) ) ;
#37340 = VECTOR ( 'NONE', #22284, 1000.000000000000000 ) ;
#37341 = ORIENTED_EDGE ( 'NONE', *, *, #44767, .F. ) ;
#37342 = ADVANCED_FACE ( 'NONE', ( #4935 ), #12793, .F. ) ;
#37343 = DIRECTION ( 'NONE',  ( -0.000000000000000000, -0.9927088740980534176, 0.1205366802553268502 ) ) ;
#37345 = AXIS2_PLACEMENT_3D ( 'NONE', #49904, #13902, #32635 ) ;
#37344 = DIRECTION ( 'NONE',  ( 0.000000000000000000, 0.000000000000000000, -1.000000000000000000 ) ) ;
#37346 = PLANE ( 'NONE',  #48955 ) ;
#37347 = ORIENTED_EDGE ( 'NONE', *, *, #41539, .T. ) ;
#37348 = CARTESIAN_POINT ( 'NONE',  ( -330.4913330509368166, -131.1080185721132807, -58.50955523165751515 ) ) ;
#37349 = DIRECTION ( 'NONE',  ( -0.000000000000000000, 1.156482317317871232E-16, 1.000000000000000000 ) ) ;
#37350 = CIRCLE ( 'NONE', #6296, 125.0000000000000000 ) ;
#37351 = CIRCLE ( 'NONE', #12157, 125.0000000000000000 ) ;
#37352 = CARTESIAN_POINT ( 'NONE',  ( -180.0000000000000568, -123.5000000000000284, -41.63467731922663972 ) ) ;
#37353 = DIRECTION ( 'NONE',  ( 0.7948544414133481562, 0.000000000000000000, 0.6068001458186002006 ) ) ;
#37354 = AXIS2_PLACEMENT_3D ( 'NONE', #14520, #37653, #42100 ) ;
#37355 = DIRECTION ( 'NONE',  ( -1.000000000000000000, 0.000000000000000000, 0.000000000000000000 ) ) ;
#37356 = VECTOR ( 'NONE', #50708, 1000.000000000000114 ) ;
#37357 = CARTESIAN_POINT ( 'NONE',  ( -154.5708152632604993, -183.6283474603465606, 64.19309449102807719 ) ) ;
#37358 = EDGE_CURVE ( 'NONE', #30881, #32314, #41432, .T. ) ;
#37359 = PLANE ( 'NONE',  #46402 ) ;
#37361 = EDGE_LOOP ( 'NONE', ( #42528, #29665, #5624, #9280 ) ) ;
#37360 = PLANE ( 'NONE',  #41289 ) ;
#37362 = ORIENTED_EDGE ( 'NONE', *, *, #17620, .F. ) ;
#37363 = DIRECTION ( 'NONE',  ( 0.000000000000000000, -1.000000000000000000, 0.000000000000000000 ) ) ;
#37364 = PLANE ( 'NONE',  #5329 ) ;
#37366 = VERTEX_POINT ( 'NONE', #25413 ) ;
#37365 = CARTESIAN_POINT ( 'NONE',  ( -12.76653800058364574, -175.3837268820161057, -119.7898618611244927 ) ) ;
#37367 = VERTEX_POINT ( 'NONE', #9641 ) ;
#37368 = CIRCLE ( 'NONE', #14723, 125.0000000000000000 ) ;
#37369 = ORIENTED_EDGE ( 'NONE', *, *, #9225, .F. ) ;
#37370 = DIRECTION ( 'NONE',  ( 0.4566292373937077542, 0.000000000000000000, 0.8896570909947499883 ) ) ;
#37371 = AXIS2_PLACEMENT_3D ( 'NONE', #2747, #37779, #38997 ) ;
#37372 = VECTOR ( 'NONE', #12256, 1000.000000000000114 ) ;
#37373 = ADVANCED_FACE ( 'NONE', ( #9388 ), #10151, .T. ) ;
#37374 = CARTESIAN_POINT ( 'NONE',  ( 74.49773146996551532, -183.6283474603465606, -22.39848972532281834 ) ) ;
#37375 = DIRECTION ( 'NONE',  ( -0.000000000000000000, 1.000000000000000000, -0.000000000000000000 ) ) ;
#37376 = VERTEX_POINT ( 'NONE', #5452 ) ;
#37377 = CARTESIAN_POINT ( 'NONE',  ( 75.48400724637754422, -193.5000000000000000, -16.06677968424457248 ) ) ;
#37379 = ORIENTED_EDGE ( 'NONE', *, *, #1622, .T. ) ;
#37378 = DIRECTION ( 'NONE',  ( 0.000000000000000000, -1.000000000000000000, 0.000000000000000000 ) ) ;
#37380 = AXIS2_PLACEMENT_3D ( 'NONE', #38797, #2805, #51434 ) ;
#37381 = AXIS2_PLACEMENT_3D ( 'NONE', #12610, #1305, #21552 ) ;
#37382 = CARTESIAN_POINT ( 'NONE',  ( -47.57632892154311577, -183.6283474603465606, 0.4300652022765314997 ) ) ;
#37383 = VERTEX_POINT ( 'NONE', #17275 ) ;
#37384 = DIRECTION ( 'NONE',  ( 0.000000000000000000, -1.000000000000000000, 1.047444401652940007E-14 ) ) ;
#37385 = ORIENTED_EDGE ( 'NONE', *, *, #37938, .F. ) ;
#37386 = PLANE ( 'NONE',  #21569 ) ;
#37387 = AXIS2_PLACEMENT_3D ( 'NONE', #39122, #14710, #47548 ) ;
#37388 = LINE ( 'NONE', #12946, #11384 ) ;
#37389 = DIRECTION ( 'NONE',  ( 0.000000000000000000, -0.3546048870425331789, 0.9350162426854158326 ) ) ;
#37390 = EDGE_CURVE ( 'NONE', #28294, #29691, #22237, .T. ) ;
#37391 = AXIS2_PLACEMENT_3D ( 'NONE', #48459, #23752, #35834 ) ;
#37392 = EDGE_LOOP ( 'NONE', ( #28582, #31113, #7011, #5075 ) ) ;
#37393 = VERTEX_POINT ( 'NONE', #25161 ) ;
#37394 = DIRECTION ( 'NONE',  ( 0.000000000000000000, 0.000000000000000000, -1.000000000000000000 ) ) ;
#37395 = CARTESIAN_POINT ( 'NONE',  ( 67.29303306501925874, -189.7472609257535510, 47.13604789772128356 ) ) ;
#37396 = ORIENTED_EDGE ( 'NONE', *, *, #7918, .F. ) ;
#37397 = CARTESIAN_POINT ( 'NONE',  ( -336.3521761649654422, -155.3847370087607374, 50.82679948493869659 ) ) ;
#37398 = ORIENTED_EDGE ( 'NONE', *, *, #22999, .F. ) ;
#37399 = EDGE_CURVE ( 'NONE', #25303, #18124, #37237, .T. ) ;
#37400 = CYLINDRICAL_SURFACE ( 'NONE', #11633, 125.0000000000000000 ) ;
#37401 = ADVANCED_FACE ( 'NONE', ( #21983 ), #38003, .T. ) ;
#37402 = CARTESIAN_POINT ( 'NONE',  ( -330.4913330509368166, -123.5000000000000284, 0.000000000000000000 ) ) ;
#37403 = ORIENTED_EDGE ( 'NONE', *, *, #29858, .T. ) ;
#37404 = DIRECTION ( 'NONE',  ( 0.000000000000000000, 1.000000000000000000, 0.000000000000000000 ) ) ;
#37405 = VERTEX_POINT ( 'NONE', #45654 ) ;
#37406 = ADVANCED_FACE ( 'NONE', ( #17544 ), #37491, .F. ) ;
#37407 = CARTESIAN_POINT ( 'NONE',  ( -22.62315034598912789, -177.1207230881787780, 121.2748789083720737 ) ) ;
#37408 = LINE ( 'NONE', #48732, #8564 ) ;
#37409 = VERTEX_POINT ( 'NONE', #30128 ) ;
#37410 = VECTOR ( 'NONE', #37866, 999.9999999999998863 ) ;
#37411 = DIRECTION ( 'NONE',  ( 0.000000000000000000, 0.000000000000000000, -1.000000000000000000 ) ) ;
#37412 = DIRECTION ( 'NONE',  ( -0.000000000000000000, -1.000000000000000000, -0.000000000000000000 ) ) ;
#37413 = DIRECTION ( 'NONE',  ( -1.000000000000000000, 1.036104688092337311E-14, 1.258058860540426107E-15 ) ) ;
#37414 = LINE ( 'NONE', #1422, #7293 ) ;
#37415 = ORIENTED_EDGE ( 'NONE', *, *, #13011, .F. ) ;
#37416 = DIRECTION ( 'NONE',  ( 0.000000000000000000, -0.000000000000000000, -1.000000000000000000 ) ) ;
#37417 = ORIENTED_EDGE ( 'NONE', *, *, #8033, .F. ) ;
#37418 = ORIENTED_EDGE ( 'NONE', *, *, #31778, .F. ) ;
#37419 = CIRCLE ( 'NONE', #50004, 125.0000000000000000 ) ;
#37420 = EDGE_CURVE ( 'NONE', #43188, #42645, #41173, .T. ) ;
#37421 = CARTESIAN_POINT ( 'NONE',  ( -305.0000000000000568, -106.5990858529439578, 57.57047073799066794 ) ) ;
#37423 = ORIENTED_EDGE ( 'NONE', *, *, #4534, .T. ) ;
#37422 = CARTESIAN_POINT ( 'NONE',  ( -336.3521761649654422, -83.15397741537739762, 43.07972642080338233 ) ) ;
#37424 = CIRCLE ( 'NONE', #500, 4.999999999999997335 ) ;
#37425 = VERTEX_POINT ( 'NONE', #17789 ) ;
#37426 = DIRECTION ( 'NONE',  ( 0.000000000000000000, 0.000000000000000000, -1.000000000000000000 ) ) ;
#37427 = AXIS2_PLACEMENT_3D ( 'NONE', #27562, #52022, #468 ) ;
#37428 = CIRCLE ( 'NONE', #26509, 125.0000000000000000 ) ;
#37429 = DIRECTION ( 'NONE',  ( -0.000000000000000000, -0.6631226582407885317, 0.7485107481711069655 ) ) ;
#37430 = ORIENTED_EDGE ( 'NONE', *, *, #11850, .T. ) ;
#37431 = LINE ( 'NONE', #34004, #49106 ) ;
#37432 = ORIENTED_EDGE ( 'NONE', *, *, #15267, .T. ) ;
#37433 = DIRECTION ( 'NONE',  ( 0.000000000000000000, -1.000000000000000000, -0.000000000000000000 ) ) ;
#37434 = LINE ( 'NONE', #13275, #50192 ) ;
#37435 = DIRECTION ( 'NONE',  ( 0.000000000000000000, 0.000000000000000000, 1.000000000000000000 ) ) ;
#37436 = DIRECTION ( 'NONE',  ( 0.000000000000000000, 0.000000000000000000, -1.000000000000000000 ) ) ;
#37437 = VERTEX_POINT ( 'NONE', #29079 ) ;
#37438 = EDGE_LOOP ( 'NONE', ( #48089, #41511, #9799, #26400 ) ) ;
#37439 = ORIENTED_EDGE ( 'NONE', *, *, #34702, .T. ) ;
#37440 = CARTESIAN_POINT ( 'NONE',  ( -339.1964088526558498, -90.39567187580801999, 48.84008046109089918 ) ) ;
#37441 = DIRECTION ( 'NONE',  ( 0.4031234292879792847, 0.000000000000000000, -0.9151456172430153524 ) ) ;
#37442 = VECTOR ( 'NONE', #39851, 1000.000000000000000 ) ;
#37443 = CIRCLE ( 'NONE', #16488, 125.0000000000000000 ) ;
#37444 = CIRCLE ( 'NONE', #13936, 125.0000000000000000 ) ;
#37445 = FACE_OUTER_BOUND ( 'NONE', #40942, .T. ) ;
#37446 = DIRECTION ( 'NONE',  ( 0.000000000000000000, -0.000000000000000000, 1.000000000000000000 ) ) ;
#37447 = EDGE_LOOP ( 'NONE', ( #43680, #16578, #20191, #42038 ) ) ;
#37448 = AXIS2_PLACEMENT_3D ( 'NONE', #39407, #22362, #2398 ) ;
#37449 = ADVANCED_FACE ( 'NONE', ( #33808 ), #49852, .T. ) ;
#37450 = EDGE_CURVE ( 'NONE', #38808, #30367, #19265, .T. ) ;
#37451 = ORIENTED_EDGE ( 'NONE', *, *, #48642, .T. ) ;
#37453 = ORIENTED_EDGE ( 'NONE', *, *, #25301, .T. ) ;
#37452 = CARTESIAN_POINT ( 'NONE',  ( -332.3517673607765914, -65.58448481710581746, 11.56382487286456140 ) ) ;
#37454 = FACE_OUTER_BOUND ( 'NONE', #5688, .T. ) ;
#37455 = ORIENTED_EDGE ( 'NONE', *, *, #47868, .F. ) ;
#37456 = CIRCLE ( 'NONE', #19007, 125.0000000000000000 ) ;
#37457 = CARTESIAN_POINT ( 'NONE',  ( 1.755575411425465360, -193.5000000000000000, 114.4616734920527392 ) ) ;
#37458 = CIRCLE ( 'NONE', #12277, 60.00000000000000000 ) ;
#37459 = FACE_OUTER_BOUND ( 'NONE', #24233, .T. ) ;
#37460 = VECTOR ( 'NONE', #47260, 999.9999999999998863 ) ;
#37461 = CIRCLE ( 'NONE', #10644, 125.0000000000000000 ) ;
#37462 = LINE ( 'NONE', #13815, #35428 ) ;
#37463 = LINE ( 'NONE', #33532, #19245 ) ;
#37464 = ORIENTED_EDGE ( 'NONE', *, *, #10235, .T. ) ;
#37465 = EDGE_CURVE ( 'NONE', #41706, #3626, #46132, .T. ) ;
#37466 = PLANE ( 'NONE',  #19148 ) ;
#37467 = AXIS2_PLACEMENT_3D ( 'NONE', #14629, #46432, #26960 ) ;
#37468 = ORIENTED_EDGE ( 'NONE', *, *, #44731, .F. ) ;
#37469 = ADVANCED_FACE ( 'NONE', ( #1496 ), #2277, .T. ) ;
#37470 = AXIS2_PLACEMENT_3D ( 'NONE', #34481, #2939, #46586 ) ;
#37471 = EDGE_LOOP ( 'NONE', ( #46767, #2092, #40881, #45429 ) ) ;
#37472 = FACE_OUTER_BOUND ( 'NONE', #3951, .T. ) ;
#37473 = EDGE_CURVE ( 'NONE', #6572, #29121, #45398, .T. ) ;
#37474 = CARTESIAN_POINT ( 'NONE',  ( -213.8817838414232426, -213.5000000000000000, -10.00000000000000000 ) ) ;
#37475 = VERTEX_POINT ( 'NONE', #45148 ) ;
#37476 = EDGE_CURVE ( 'NONE', #5492, #23514, #18045, .T. ) ;
#37477 = LINE ( 'NONE', #13828, #8873 ) ;
#37478 = FACE_OUTER_BOUND ( 'NONE', #7004, .T. ) ;
#37479 = PLANE ( 'NONE',  #48356 ) ;
#37480 = DIRECTION ( 'NONE',  ( 0.000000000000000000, -1.000000000000000000, 0.000000000000000000 ) ) ;
#37481 = DIRECTION ( 'NONE',  ( 0.000000000000000000, 0.9350162426854121689, -0.3546048870425426158 ) ) ;
#37482 = FACE_BOUND ( 'NONE', #15573, .T. ) ;
#37483 = ORIENTED_EDGE ( 'NONE', *, *, #44292, .F. ) ;
#37484 = VECTOR ( 'NONE', #31016, 1000.000000000000227 ) ;
#37485 = CIRCLE ( 'NONE', #14013, 60.00000000000000000 ) ;
#37486 = DIRECTION ( 'NONE',  ( 0.000000000000000000, -1.000000000000000000, 0.000000000000000000 ) ) ;
#37487 = AXIS2_PLACEMENT_3D ( 'NONE', #25011, #21059, #16868 ) ;
#37488 = VERTEX_POINT ( 'NONE', #49070 ) ;
#37489 = CARTESIAN_POINT ( 'NONE',  ( -336.3521761649654422, -164.5945333327934463, -42.41660376256285048 ) ) ;
#37490 = VERTEX_POINT ( 'NONE', #13052 ) ;
#37491 = PLANE ( 'NONE',  #44465 ) ;
#37492 = AXIS2_PLACEMENT_3D ( 'NONE', #34740, #31846, #35263 ) ;
#37493 = LINE ( 'NONE', #5964, #18410 ) ;
#37494 = CIRCLE ( 'NONE', #3097, 125.0000000000000000 ) ;
#37496 = EDGE_LOOP ( 'NONE', ( #27081, #27466, #32951, #6566 ) ) ;
#37495 = DIRECTION ( 'NONE',  ( 0.000000000000000000, 0.000000000000000000, -1.000000000000000000 ) ) ;
#37497 = VECTOR ( 'NONE', #26597, 1000.000000000000114 ) ;
#37498 = AXIS2_PLACEMENT_3D ( 'NONE', #15069, #35785, #39467 ) ;
#37499 = AXIS2_PLACEMENT_3D ( 'NONE', #41903, #30077, #22711 ) ;
#37500 = DIRECTION ( 'NONE',  ( 0.000000000000000000, 0.000000000000000000, -1.000000000000000000 ) ) ;
#37501 = ORIENTED_EDGE ( 'NONE', *, *, #31771, .F. ) ;
#37502 = VERTEX_POINT ( 'NONE', #9132 ) ;
#37503 = EDGE_LOOP ( 'NONE', ( #7075, #25839, #25583, #36718 ) ) ;
#37504 = AXIS2_PLACEMENT_3D ( 'NONE', #34422, #2620, #46517 ) ;
#37505 = EDGE_CURVE ( 'NONE', #22971, #20552, #22763, .T. ) ;
#37506 = DIRECTION ( 'NONE',  ( -1.000000000000000000, 0.000000000000000000, 0.000000000000000000 ) ) ;
#37507 = LINE ( 'NONE', #49080, #10909 ) ;
#37508 = EDGE_LOOP ( 'NONE', ( #28428, #10479, #35699, #46869 ) ) ;
#37509 = CARTESIAN_POINT ( 'NONE',  ( -48.64924157374596092, -189.7472609257535510, 124.9998842437354227 ) ) ;
#37510 = LINE ( 'NONE', #29616, #1836 ) ;
#37511 = LINE ( 'NONE', #20974, #15464 ) ;
#37512 = ORIENTED_EDGE ( 'NONE', *, *, #3057, .T. ) ;
#37513 = EDGE_CURVE ( 'NONE', #28039, #28978, #11431, .T. ) ;
#37514 = EDGE_CURVE ( 'NONE', #22576, #7887, #19084, .T. ) ;
#37515 = EDGE_CURVE ( 'NONE', #650, #45883, #23016, .T. ) ;
#37516 = ADVANCED_FACE ( 'NONE', ( #11180 ), #3038, .F. ) ;
#37517 = CARTESIAN_POINT ( 'NONE',  ( 18.49541618049842384, -183.6283474603465606, 105.5434062319798016 ) ) ;
#37518 = LINE ( 'NONE', #6951, #461 ) ;
#37519 = ORIENTED_EDGE ( 'NONE', *, *, #29564, .F. ) ;
#37521 = VERTEX_POINT ( 'NONE', #34827 ) ;
#37520 = CARTESIAN_POINT ( 'NONE',  ( -339.1964088526558498, -182.0095552316575152, 7.608018572113563138 ) ) ;
#37522 = AXIS2_PLACEMENT_3D ( 'NONE', #19879, #23819, #408 ) ;
#37523 = ORIENTED_EDGE ( 'NONE', *, *, #43648, .F. ) ;
#37524 = VECTOR ( 'NONE', #18938, 1000.000000000000000 ) ;
#37525 = EDGE_CURVE ( 'NONE', #7546, #18880, #25152, .T. ) ;
#37526 = ORIENTED_EDGE ( 'NONE', *, *, #50958, .F. ) ;
#37527 = DIRECTION ( 'NONE',  ( 0.000000000000000000, 0.000000000000000000, 1.000000000000000000 ) ) ;
#37528 = DIRECTION ( 'NONE',  ( 0.000000000000000000, -1.000000000000000000, 0.000000000000000000 ) ) ;
#37529 = VERTEX_POINT ( 'NONE', #51161 ) ;
#37530 = VECTOR ( 'NONE', #19360, 999.9999999999998863 ) ;
#37531 = CARTESIAN_POINT ( 'NONE',  ( -49.32472275501067571, -175.3837268820161057, -0.5338233779647935107 ) ) ;
#37532 = CARTESIAN_POINT ( 'NONE',  ( -48.13092511607445090, -175.3837268820161057, -0.9374196611341135688 ) ) ;
#37533 = ORIENTED_EDGE ( 'NONE', *, *, #42577, .T. ) ;
#37534 = EDGE_CURVE ( 'NONE', #18800, #16080, #31154, .T. ) ;
#37535 = FACE_OUTER_BOUND ( 'NONE', #12312, .T. ) ;
#37536 = ORIENTED_EDGE ( 'NONE', *, *, #394, .T. ) ;
#37537 = EDGE_CURVE ( 'NONE', #27045, #8870, #31022, .T. ) ;
#37538 = VERTEX_POINT ( 'NONE', #42736 ) ;
#37539 = DIRECTION ( 'NONE',  ( 0.000000000000000000, 0.5000000000000013323, -0.8660254037844380415 ) ) ;
#37540 = VECTOR ( 'NONE', #19033, 1000.000000000000000 ) ;
#37541 = LINE ( 'NONE', #32814, #24766 ) ;
#37542 = ADVANCED_FACE ( 'NONE', ( #22516 ), #46423, .T. ) ;
#37543 = VECTOR ( 'NONE', #11318, 1000.000000000000000 ) ;
#37544 = PLANE ( 'NONE',  #49879 ) ;
#37545 = DIRECTION ( 'NONE',  ( 0.000000000000000000, -1.000000000000000000, 0.000000000000000000 ) ) ;
#37546 = ORIENTED_EDGE ( 'NONE', *, *, #16170, .T. ) ;
#37547 = AXIS2_PLACEMENT_3D ( 'NONE', #22548, #22011, #38031 ) ;
#37548 = DIRECTION ( 'NONE',  ( 0.000000000000000000, 1.000000000000000000, 0.000000000000000000 ) ) ;
#37549 = DIRECTION ( 'NONE',  ( -0.000000000000000000, 1.000000000000000000, 0.000000000000000000 ) ) ;
#37550 = EDGE_CURVE ( 'NONE', #28018, #14212, #18809, .T. ) ;
#37551 = CARTESIAN_POINT ( 'NONE',  ( -114.9600645115007040, -177.1207230881787780, 105.8550183720738573 ) ) ;
#37552 = LINE ( 'NONE', #18094, #33765 ) ;
#37553 = AXIS2_PLACEMENT_3D ( 'NONE', #32903, #41055, #25049 ) ;
#37554 = ORIENTED_EDGE ( 'NONE', *, *, #51138, .T. ) ;
#37555 = CARTESIAN_POINT ( 'NONE',  ( -166.6807411098556031, -183.6283474603465606, 37.47770156625504256 ) ) ;
#37556 = DIRECTION ( 'NONE',  ( 0.000000000000000000, 1.000000000000000000, -0.000000000000000000 ) ) ;
#37557 = EDGE_CURVE ( 'NONE', #5101, #17733, #46678, .T. ) ;
#37558 = VECTOR ( 'NONE', #51759, 1000.000000000000114 ) ;
#37559 = CARTESIAN_POINT ( 'NONE',  ( -164.2512865680372727, -193.5000000000000000, -47.13604789772046644 ) ) ;
#37560 = VERTEX_POINT ( 'NONE', #27470 ) ;
#37561 = FACE_BOUND ( 'NONE', #9268, .T. ) ;
#37562 = DIRECTION ( 'NONE',  ( 0.9995608365087942371, 0.000000000000000000, 0.02963332782256331357 ) ) ;
#37563 = ORIENTED_EDGE ( 'NONE', *, *, #25655, .T. ) ;
#37564 = CARTESIAN_POINT ( 'NONE',  ( -305.0000000000000568, -74.40671499923421095, -34.49419324804659936 ) ) ;
#37565 = ORIENTED_EDGE ( 'NONE', *, *, #51891, .F. ) ;
#37566 = EDGE_CURVE ( 'NONE', #21356, #39530, #14620, .T. ) ;
#37567 = VECTOR ( 'NONE', #48468, 1000.000000000000000 ) ;
#37568 = DIRECTION ( 'NONE',  ( -0.000000000000000000, 1.000000000000000000, -0.000000000000000000 ) ) ;
#37569 = AXIS2_PLACEMENT_3D ( 'NONE', #10498, #13421, #29968 ) ;
#37570 = DIRECTION ( 'NONE',  ( -0.000000000000000000, 1.000000000000000000, -0.000000000000000000 ) ) ;
#37571 = DIRECTION ( 'NONE',  ( 0.000000000000000000, -0.8229838658936494689, 0.5680647467311658039 ) ) ;
#37572 = LINE ( 'NONE', #49660, #6938 ) ;
#37573 = AXIS2_PLACEMENT_3D ( 'NONE', #40583, #20630, #36665 ) ;
#37574 = FACE_OUTER_BOUND ( 'NONE', #46984, .T. ) ;
#37575 = CARTESIAN_POINT ( 'NONE',  ( 63.31225588004632243, -183.6283474603465606, 55.92572546981597981 ) ) ;
#37576 = VERTEX_POINT ( 'NONE', #26431 ) ;
#37577 = LINE ( 'NONE', #33627, #24823 ) ;
#37578 = EDGE_LOOP ( 'NONE', ( #47053, #3431, #47752, #28619 ) ) ;
#37579 = LINE ( 'NONE', #13657, #50239 ) ;
#37580 = CIRCLE ( 'NONE', #9072, 5.000000000000001776 ) ;
#37581 = EDGE_LOOP ( 'NONE', ( #30777, #8172, #28216, #51377 ) ) ;
#37582 = DIRECTION ( 'NONE',  ( -0.000000000000000000, 1.000000000000000000, -0.000000000000000000 ) ) ;
#37583 = VECTOR ( 'NONE', #23507, 1000.000000000000000 ) ;
#37584 = ADVANCED_FACE ( 'NONE', ( #7248 ), #42463, .F. ) ;
#37585 = EDGE_LOOP ( 'NONE', ( #45872, #7272, #45405, #38751 ) ) ;
#37586 = EDGE_CURVE ( 'NONE', #3837, #21231, #47455, .T. ) ;
#37587 = ADVANCED_FACE ( 'NONE', ( #39304 ), #3306, .F. ) ;
#37588 = AXIS2_PLACEMENT_3D ( 'NONE', #33406, #13419, #8694 ) ;
#37589 = EDGE_CURVE ( 'NONE', #19021, #29776, #38571, .T. ) ;
#37590 = CARTESIAN_POINT ( 'NONE',  ( 57.31108707223381060, -175.3837268820161057, -66.58401203837753712 ) ) ;
#37591 = DIRECTION ( 'NONE',  ( -0.000000000000000000, 1.000000000000000000, 0.000000000000000000 ) ) ;
#37592 = VERTEX_POINT ( 'NONE', #30371 ) ;
#37595 = EDGE_LOOP ( 'NONE', ( #27461, #14645, #52033, #680 ) ) ;
#37594 = CARTESIAN_POINT ( 'NONE',  ( -238.7407812814481076, -213.5000000000000000, 41.45482488023466772 ) ) ;
#37593 = DIRECTION ( 'NONE',  ( 0.000000000000000000, -0.000000000000000000, -1.000000000000000000 ) ) ;
#37596 = CARTESIAN_POINT ( 'NONE',  ( -31.30262293407085039, -193.5000000000000000, -123.8142468240611294 ) ) ;
#37597 = ORIENTED_EDGE ( 'NONE', *, *, #25078, .F. ) ;
#37598 = FACE_OUTER_BOUND ( 'NONE', #18082, .T. ) ;
#37599 = VERTEX_POINT ( 'NONE', #24312 ) ;
#37600 = DIRECTION ( 'NONE',  ( 1.000000000000000000, -0.000000000000000000, 0.000000000000000000 ) ) ;
#37603 = ORIENTED_EDGE ( 'NONE', *, *, #6699, .T. ) ;
#37602 = DIRECTION ( 'NONE',  ( -0.4566292373937200777, 0.000000000000000000, 0.8896570909947436601 ) ) ;
#37601 = DIRECTION ( 'NONE',  ( -0.000000000000000000, 1.000000000000000000, -0.000000000000000000 ) ) ;
#37604 = EDGE_LOOP ( 'NONE', ( #33990, #23760, #24557, #41598 ) ) ;
#37605 = PLANE ( 'NONE',  #45023 ) ;
#37606 = CARTESIAN_POINT ( 'NONE',  ( -160.0000000000000284, -123.5000000000000284, 41.63467731922665394 ) ) ;
#37607 = AXIS2_PLACEMENT_3D ( 'NONE', #43546, #14654, #23566 ) ;
#37608 = LINE ( 'NONE', #21052, #8078 ) ;
#37609 = EDGE_CURVE ( 'NONE', #36764, #36384, #16439, .T. ) ;
#37610 = EDGE_LOOP ( 'NONE', ( #21908, #32804, #28907, #34638 ) ) ;
#37611 = DIRECTION ( 'NONE',  ( -0.9785564922995032555, 0.000000000000000000, -0.2059786187411021818 ) ) ;
#37612 = CARTESIAN_POINT ( 'NONE',  ( -48.47912675150885065, -177.1207230881787780, 6.938893903907228378E-15 ) ) ;
#37613 = CARTESIAN_POINT ( 'NONE',  ( -170.0000000000000284, -123.5000000000000284, 45.63467731922665394 ) ) ;
#37614 = AXIS2_PLACEMENT_3D ( 'NONE', #8224, #8471, #4277 ) ;
#37615 = PLANE ( 'NONE',  #37487 ) ;
#37616 = ORIENTED_EDGE ( 'NONE', *, *, #15846, .T. ) ;
#37617 = CARTESIAN_POINT ( 'NONE',  ( -2.429962845726266397E-15, 20.00000000000000355, 0.000000000000000000 ) ) ;
#37618 = CARTESIAN_POINT ( 'NONE',  ( -365.0000000000001137, -78.50000000000002842, -10.00000000000000711 ) ) ;
#37619 = EDGE_CURVE ( 'NONE', #39147, #12949, #44544, .T. ) ;
#37620 = DIRECTION ( 'NONE',  ( -1.000000000000000000, 0.000000000000000000, 0.000000000000000000 ) ) ;
#37621 = VERTEX_POINT ( 'NONE', #44804 ) ;
#37622 = VECTOR ( 'NONE', #7947, 1000.000000000000000 ) ;
#37623 = CARTESIAN_POINT ( 'NONE',  ( 60.00000000000001421, -63.50000000000000000, -60.00000000000000711 ) ) ;
#37624 = DIRECTION ( 'NONE',  ( 0.000000000000000000, 1.000000000000000000, 0.000000000000000000 ) ) ;
#37625 = CARTESIAN_POINT ( 'NONE',  ( -149.5539421794694022, -189.7472609257535510, 73.54509967498655953 ) ) ;
#37626 = PLANE ( 'NONE',  #51792 ) ;
#37628 = AXIS2_PLACEMENT_3D ( 'NONE', #20724, #16261, #24660 ) ;
#37627 = LINE ( 'NONE', #13968, #38855 ) ;
#37629 = CARTESIAN_POINT ( 'NONE',  ( 21.49274850782854074, -189.7472609257535510, -103.5805805771126415 ) ) ;
#37630 = DIRECTION ( 'NONE',  ( 0.000000000000000000, 0.000000000000000000, 1.000000000000000000 ) ) ;
#37632 = ORIENTED_EDGE ( 'NONE', *, *, #44097, .T. ) ;
#37631 = CARTESIAN_POINT ( 'NONE',  ( 75.37518750349086361, -177.1207230881787780, 6.025661128238926523 ) ) ;
#37633 = ORIENTED_EDGE ( 'NONE', *, *, #41356, .T. ) ;
#37634 = DIRECTION ( 'NONE',  ( -1.000000000000000000, 0.000000000000000000, 0.000000000000000000 ) ) ;
#37635 = EDGE_CURVE ( 'NONE', #29101, #34495, #42776, .T. ) ;
#37636 = DIRECTION ( 'NONE',  ( -0.000000000000000000, 1.000000000000000000, -0.000000000000000000 ) ) ;
#37638 = EDGE_LOOP ( 'NONE', ( #26261, #28316, #47335, #49771 ) ) ;
#37637 = LINE ( 'NONE', #13717, #26170 ) ;
#37639 = VECTOR ( 'NONE', #37138, 1000.000000000000114 ) ;
#37640 = ORIENTED_EDGE ( 'NONE', *, *, #18949, .F. ) ;
#37641 = AXIS2_PLACEMENT_3D ( 'NONE', #46259, #10755, #22593 ) ;
#37642 = ORIENTED_EDGE ( 'NONE', *, *, #11551, .F. ) ;
#37643 = FACE_OUTER_BOUND ( 'NONE', #10966, .T. ) ;
#37644 = EDGE_CURVE ( 'NONE', #49035, #1773, #20107, .T. ) ;
#37645 = ADVANCED_FACE ( 'NONE', ( #27725 ), #47970, .T. ) ;
#37646 = CARTESIAN_POINT ( 'NONE',  ( -83.89965873179625078, -189.7472609257535510, 118.8334608768482354 ) ) ;
#37647 = DIRECTION ( 'NONE',  ( 0.05924062789370748011, 0.000000000000000000, 0.9982437317643217956 ) ) ;
#37648 = EDGE_LOOP ( 'NONE', ( #29076, #7643, #36262, #11332 ) ) ;
#37649 = DIRECTION ( 'NONE',  ( 0.000000000000000000, 0.000000000000000000, 1.000000000000000000 ) ) ;
#37650 = CIRCLE ( 'NONE', #31803, 125.0000000000000000 ) ;
#37652 = ORIENTED_EDGE ( 'NONE', *, *, #32952, .F. ) ;
#37651 = CYLINDRICAL_SURFACE ( 'NONE', #43436, 125.0000000000000000 ) ;
#37653 = DIRECTION ( 'NONE',  ( -0.000000000000000000, 1.000000000000000000, -0.000000000000000000 ) ) ;
#37654 = EDGE_LOOP ( 'NONE', ( #45607, #4811 ) ) ;
#37655 = FACE_OUTER_BOUND ( 'NONE', #26125, .T. ) ;
#37656 = VERTEX_POINT ( 'NONE', #128 ) ;
#37657 = DIRECTION ( 'NONE',  ( 0.000000000000000000, 1.000000000000000000, 0.000000000000000000 ) ) ;
#37658 = DIRECTION ( 'NONE',  ( -0.7948544414133523750, 0.000000000000000000, -0.6068001458185945385 ) ) ;
#37659 = DIRECTION ( 'NONE',  ( -0.9982437317643222396, 0.000000000000000000, 0.05924062789370006937 ) ) ;
#37660 = AXIS2_PLACEMENT_3D ( 'NONE', #47239, #7792, #35917 ) ;
#37661 = ORIENTED_EDGE ( 'NONE', *, *, #625, .T. ) ;
#37662 = EDGE_LOOP ( 'NONE', ( #49376, #37417, #27948, #28240 ) ) ;
#37663 = DIRECTION ( 'NONE',  ( -0.9266896074318317078, 0.000000000000000000, -0.3758275821142421647 ) ) ;
#37664 = CARTESIAN_POINT ( 'NONE',  ( -170.7514454179067513, -177.1207230881787780, -20.63201007055403480 ) ) ;
#37665 = ORIENTED_EDGE ( 'NONE', *, *, #18568, .F. ) ;
#37666 = EDGE_CURVE ( 'NONE', #13356, #5376, #40317, .T. ) ;
#37667 = FACE_OUTER_BOUND ( 'NONE', #36410, .T. ) ;
#37668 = ORIENTED_EDGE ( 'NONE', *, *, #42632, .T. ) ;
#37669 = LINE ( 'NONE', #33478, #8257 ) ;
#37670 = CARTESIAN_POINT ( 'NONE',  ( -165.8930023212105596, -193.5000000000000000, -39.87457906003682950 ) ) ;
#37671 = EDGE_CURVE ( 'NONE', #31250, #21618, #16173, .T. ) ;
#37672 = EDGE_LOOP ( 'NONE', ( #43996, #38841, #15068, #19710 ) ) ;
#37673 = CARTESIAN_POINT ( 'NONE',  ( -339.1964088526558498, -115.8919814278871598, -58.50955523165758621 ) ) ;
#37674 = VERTEX_POINT ( 'NONE', #7761 ) ;
#37675 = AXIS2_PLACEMENT_3D ( 'NONE', #20272, #44194, #36047 ) ;
#37676 = DIRECTION ( 'NONE',  ( 0.000000000000000000, 1.000000000000000000, -0.000000000000000000 ) ) ;
#37677 = AXIS2_PLACEMENT_3D ( 'NONE', #3953, #19977, #36010 ) ;
#37678 = LINE ( 'NONE', #49774, #8000 ) ;
#37679 = LINE ( 'NONE', #2455, #20196 ) ;
#37680 = EDGE_LOOP ( 'NONE', ( #41425, #27088, #14981, #31106 ) ) ;
#37681 = CIRCLE ( 'NONE', #41006, 125.0000000000000000 ) ;
#37682 = DIRECTION ( 'NONE',  ( 0.000000000000000000, 0.000000000000000000, -1.000000000000000000 ) ) ;
#37683 = CARTESIAN_POINT ( 'NONE',  ( -339.1964088526558498, -123.5000000000000284, 0.000000000000000000 ) ) ;
#37684 = FACE_OUTER_BOUND ( 'NONE', #40738, .T. ) ;
#37685 = EDGE_CURVE ( 'NONE', #16176, #44109, #23791, .T. ) ;
#37686 = CARTESIAN_POINT ( 'NONE',  ( -213.8817838414232426, -193.5000000000000000, -10.00000000000000000 ) ) ;
#37687 = ORIENTED_EDGE ( 'NONE', *, *, #45900, .F. ) ;
#37688 = LINE ( 'NONE', #10090, #1046 ) ;
#37689 = ORIENTED_EDGE ( 'NONE', *, *, #44672, .T. ) ;
#37690 = AXIS2_PLACEMENT_3D ( 'NONE', #29865, #13581, #29603 ) ;
#37691 = DIRECTION ( 'NONE',  ( 0.000000000000000000, -1.000000000000000000, 0.000000000000000000 ) ) ;
#37693 = ORIENTED_EDGE ( 'NONE', *, *, #9263, .F. ) ;
#37692 = PLANE ( 'NONE',  #16134 ) ;
#37694 = ORIENTED_EDGE ( 'NONE', *, *, #44001, .T. ) ;
#37695 = CARTESIAN_POINT ( 'NONE',  ( 47.28479244271900939, -189.7472609257535510, -78.77358243914883928 ) ) ;
#37696 = AXIS2_PLACEMENT_3D ( 'NONE', #34545, #50598, #46656 ) ;
#37697 = EDGE_CURVE ( 'NONE', #4360, #9774, #17623, .T. ) ;
#37698 = DIRECTION ( 'NONE',  ( -0.000000000000000000, -0.1205366802553268363, -0.9927088740980534176 ) ) ;
#37699 = ORIENTED_EDGE ( 'NONE', *, *, #1257, .T. ) ;
#37700 = DIRECTION ( 'NONE',  ( 0.000000000000000000, 0.000000000000000000, 1.000000000000000000 ) ) ;
#37701 = ORIENTED_EDGE ( 'NONE', *, *, #13788, .F. ) ;
#37702 = FACE_OUTER_BOUND ( 'NONE', #43023, .T. ) ;
#37703 = CARTESIAN_POINT ( 'NONE',  ( 48.66843973345087448, 30.00000000000000355, -40.95752564483601788 ) ) ;
#37704 = EDGE_CURVE ( 'NONE', #36128, #41126, #20359, .T. ) ;
#37705 = EDGE_CURVE ( 'NONE', #45751, #47856, #32712, .T. ) ;
#37706 = CARTESIAN_POINT ( 'NONE',  ( 76.28370911321322012, -193.5000000000000000, -7.696413904697510411 ) ) ;
#37707 = PLANE ( 'NONE',  #46749 ) ;
#37708 = ORIENTED_EDGE ( 'NONE', *, *, #26891, .T. ) ;
#37709 = ORIENTED_EDGE ( 'NONE', *, *, #9888, .F. ) ;
#37710 = ORIENTED_EDGE ( 'NONE', *, *, #14268, .F. ) ;
#37711 = DIRECTION ( 'NONE',  ( 1.000000000000000000, -0.000000000000000000, -0.000000000000000000 ) ) ;
#37712 = LINE ( 'NONE', #45354, #25990 ) ;
#37713 = EDGE_CURVE ( 'NONE', #34468, #33439, #32454, .T. ) ;
#37714 = VECTOR ( 'NONE', #48822, 1000.000000000000000 ) ;
#37715 = DIRECTION ( 'NONE',  ( -0.000000000000000000, 1.000000000000000000, -0.000000000000000000 ) ) ;
#37716 = CARTESIAN_POINT ( 'NONE',  ( -77.67449977936060179, -189.7472609257535510, -121.5427093402339267 ) ) ;
#37717 = ORIENTED_EDGE ( 'NONE', *, *, #44513, .F. ) ;
#37718 = VECTOR ( 'NONE', #9923, 1000.000000000000000 ) ;
#37719 = VERTEX_POINT ( 'NONE', #12480 ) ;
#37721 = ORIENTED_EDGE ( 'NONE', *, *, #9872, .F. ) ;
#37720 = FACE_OUTER_BOUND ( 'NONE', #4394, .T. ) ;
#37722 = ORIENTED_EDGE ( 'NONE', *, *, #4594, .T. ) ;
#37723 = FACE_OUTER_BOUND ( 'NONE', #27751, .T. ) ;
#37724 = ADVANCED_FACE ( 'NONE', ( #35609 ), #40845, .F. ) ;
#37725 = CARTESIAN_POINT ( 'NONE',  ( 0.000000000000000000, -144.4216883355098844, -55.16595831843940090 ) ) ;
#37726 = DIRECTION ( 'NONE',  ( 0.000000000000000000, 1.669960466207006380E-13, -1.000000000000000000 ) ) ;
#37727 = CARTESIAN_POINT ( 'NONE',  ( -159.5526844214375899, -183.6283474603465606, 57.33816169485221081 ) ) ;
#37728 = ORIENTED_EDGE ( 'NONE', *, *, #8929, .T. ) ;
#37729 = CARTESIAN_POINT ( 'NONE',  ( 50.08808042611237710, -193.5000000000000000, -76.87330921200083367 ) ) ;
#37730 = VERTEX_POINT ( 'NONE', #39798 ) ;
#37731 = VECTOR ( 'NONE', #50135, 1000.000000000000227 ) ;
#37732 = VERTEX_POINT ( 'NONE', #3823 ) ;
#37733 = CYLINDRICAL_SURFACE ( 'NONE', #2750, 125.0000000000000000 ) ;
#37734 = DIRECTION ( 'NONE',  ( 0.000000000000000000, 0.000000000000000000, -1.000000000000000000 ) ) ;
#37735 = VERTEX_POINT ( 'NONE', #24056 ) ;
#37736 = CARTESIAN_POINT ( 'NONE',  ( -37.08895481556041318, -177.1207230881787780, 124.4799742258550310 ) ) ;
#37737 = PLANE ( 'NONE',  #43117 ) ;
#37738 = CARTESIAN_POINT ( 'NONE',  ( -339.1964088526558498, -178.8432607619606358, 20.45418021416736565 ) ) ;
#37739 = CARTESIAN_POINT ( 'NONE',  ( -48.47912675150885065, -120.5000000000000284, 6.938893903907228378E-15 ) ) ;
#37740 = DIRECTION ( 'NONE',  ( 0.000000000000000000, -1.000000000000000000, 0.000000000000000000 ) ) ;
#37741 = FACE_BOUND ( 'NONE', #45053, .T. ) ;
#37742 = ORIENTED_EDGE ( 'NONE', *, *, #7285, .F. ) ;
#37743 = VECTOR ( 'NONE', #21731, 1000.000000000000000 ) ;
#37744 = DIRECTION ( 'NONE',  ( 1.000000000000000000, -0.000000000000000000, -0.000000000000000000 ) ) ;
#37745 = ORIENTED_EDGE ( 'NONE', *, *, #42332, .T. ) ;
#37746 = ADVANCED_FACE ( 'NONE', ( #19846 ), #35879, .F. ) ;
#37747 = EDGE_LOOP ( 'NONE', ( #28444, #10757, #9345, #51862 ) ) ;
#37748 = ADVANCED_FACE ( 'NONE', ( #40071 ), #20105, .T. ) ;
#37749 = DIRECTION ( 'NONE',  ( 0.2348860457809775482, 0.000000000000000000, 0.9720229140804121926 ) ) ;
#37750 = VERTEX_POINT ( 'NONE', #15661 ) ;
#37751 = CARTESIAN_POINT ( 'NONE',  ( 59.00260725618640123, -177.1207230881787780, -63.81752780152988436 ) ) ;
#37752 = CARTESIAN_POINT ( 'NONE',  ( -336.3521761649653854, -125.1322888500942554, -59.97779283292990016 ) ) ;
#37754 = ORIENTED_EDGE ( 'NONE', *, *, #22522, .F. ) ;
#37753 = DIRECTION ( 'NONE',  ( 0.6965510290629932655, 0.000000000000000000, 0.7175072570443347120 ) ) ;
#37755 = EDGE_CURVE ( 'NONE', #3016, #37183, #51932, .T. ) ;
#37756 = CARTESIAN_POINT ( 'NONE',  ( -305.0000000000000568, -163.6602333390099773, -44.57752413667984825 ) ) ;
#37757 = VERTEX_POINT ( 'NONE', #38652 ) ;
#37758 = VERTEX_POINT ( 'NONE', #42339 ) ;
#37759 = EDGE_CURVE ( 'NONE', #50461, #16663, #32961, .T. ) ;
#37760 = VECTOR ( 'NONE', #23548, 1000.000000000000000 ) ;
#37762 = EDGE_LOOP ( 'NONE', ( #1397, #14672, #6584, #3076 ) ) ;
#37761 = CIRCLE ( 'NONE', #20128, 60.00000000000000000 ) ;
#37763 = DIRECTION ( 'NONE',  ( -0.000000000000000000, -0.2393156642875615969, -0.9709418174260511236 ) ) ;
#37764 = DIRECTION ( 'NONE',  ( -0.000000000000000000, 0.6631226582407863113, -0.7485107481711089639 ) ) ;
#37765 = EDGE_CURVE ( 'NONE', #3689, #29108, #10290, .T. ) ;
#37766 = LINE ( 'NONE', #46698, #15076 ) ;
#37767 = CARTESIAN_POINT ( 'NONE',  ( -332.3517673607765914, -65.82380048139334860, 12.53476669029061519 ) ) ;
#37768 = DIRECTION ( 'NONE',  ( 0.2059786187410889424, 0.000000000000000000, 0.9785564922995060311 ) ) ;
#37769 = ORIENTED_EDGE ( 'NONE', *, *, #36602, .F. ) ;
#37770 = CARTESIAN_POINT ( 'NONE',  ( -165.8930023212105596, -175.3837268820161057, -39.87457906003687214 ) ) ;
#37771 = PLANE ( 'NONE',  #9717 ) ;
#37772 = ORIENTED_EDGE ( 'NONE', *, *, #24077, .F. ) ;
#37774 = VERTEX_POINT ( 'NONE', #25106 ) ;
#37773 = CARTESIAN_POINT ( 'NONE',  ( -159.3947744408687868, -183.6283474603465606, -55.44293326708444880 ) ) ;
#37775 = EDGE_LOOP ( 'NONE', ( #46356, #5908, #38399, #24070 ) ) ;
#37776 = VECTOR ( 'NONE', #44150, 1000.000000000000000 ) ;
#37777 = ORIENTED_EDGE ( 'NONE', *, *, #24305, .F. ) ;
#37778 = DIRECTION ( 'NONE',  ( -1.000000000000000000, 0.000000000000000000, 0.000000000000000000 ) ) ;
#37779 = DIRECTION ( 'NONE',  ( -1.000000000000000000, 0.000000000000000000, 0.000000000000000000 ) ) ;
#37780 = ORIENTED_EDGE ( 'NONE', *, *, #6379, .F. ) ;
#37781 = DIRECTION ( 'NONE',  ( -1.000000000000000000, 0.000000000000000000, 0.000000000000000000 ) ) ;
#37782 = DIRECTION ( 'NONE',  ( 0.000000000000000000, 0.000000000000000000, -1.000000000000000000 ) ) ;
#37783 = ORIENTED_EDGE ( 'NONE', *, *, #10514, .F. ) ;
#37784 = CARTESIAN_POINT ( 'NONE',  ( 1.755575411425465360, -175.3837268820161057, 114.4616734920527392 ) ) ;
#37785 = ORIENTED_EDGE ( 'NONE', *, *, #20745, .F. ) ;
#37786 = ORIENTED_EDGE ( 'NONE', *, *, #2656, .F. ) ;
#37787 = CARTESIAN_POINT ( 'NONE',  ( 0.000000000000000000, 106.9200652401092526, -109.8944711476178213 ) ) ;
#37788 = CARTESIAN_POINT ( 'NONE',  ( -339.1964088526558498, -123.0000000000002700, -59.00000000000002132 ) ) ;
#37789 = LINE ( 'NONE', #41469, #17997 ) ;
#37790 = CARTESIAN_POINT ( 'NONE',  ( 73.87536152799695799, -175.3837268820161057, -25.58083653558413317 ) ) ;
#37791 = ORIENTED_EDGE ( 'NONE', *, *, #28771, .F. ) ;
#37792 = DIRECTION ( 'NONE',  ( 1.000000000000000000, -0.000000000000000000, -0.000000000000000000 ) ) ;
#37793 = DIRECTION ( 'NONE',  ( -0.000000000000000000, 1.000000000000000000, -0.000000000000000000 ) ) ;
#37794 = DIRECTION ( 'NONE',  ( 0.000000000000000000, -0.000000000000000000, 1.000000000000000000 ) ) ;
#37795 = CARTESIAN_POINT ( 'NONE',  ( 75.12566530717464275, -189.7472609257535510, 18.62405380494842433 ) ) ;
#37796 = ORIENTED_EDGE ( 'NONE', *, *, #50629, .T. ) ;
#37797 = CARTESIAN_POINT ( 'NONE',  ( -48.47912675150885065, -132.5479369270331915, 6.938893903907228378E-15 ) ) ;
#37798 = CARTESIAN_POINT ( 'NONE',  ( 73.80528149577284580, -175.3837268820161057, 25.91377046305969145 ) ) ;
#37799 = AXIS2_PLACEMENT_3D ( 'NONE', #13730, #13997, #37649 ) ;
#37800 = AXIS2_PLACEMENT_3D ( 'NONE', #16626, #49471, #32634 ) ;
#37801 = LINE ( 'NONE', #22290, #530 ) ;
#37802 = VERTEX_POINT ( 'NONE', #46559 ) ;
#37803 = EDGE_LOOP ( 'NONE', ( #25466, #30385, #10835, #7002 ) ) ;
#37804 = LINE ( 'NONE', #50179, #1243 ) ;
#37805 = ADVANCED_FACE ( 'NONE', ( #49276 ), #14243, .T. ) ;
#37806 = DIRECTION ( 'NONE',  ( -1.000000000000000000, -0.000000000000000000, -0.000000000000000000 ) ) ;
#37807 = CARTESIAN_POINT ( 'NONE',  ( -136.5246168469702468, -183.6283474603465606, 87.31661597576147926 ) ) ;
#37808 = ADVANCED_FACE ( 'NONE', ( #41117 ), #38403, .T. ) ;
#37809 = ORIENTED_EDGE ( 'NONE', *, *, #37297, .T. ) ;
#37810 = EDGE_CURVE ( 'NONE', #7741, #12493, #22641, .T. ) ;
#37811 = ORIENTED_EDGE ( 'NONE', *, *, #45245, .T. ) ;
#37812 = ORIENTED_EDGE ( 'NONE', *, *, #48467, .F. ) ;
#37813 = EDGE_CURVE ( 'NONE', #27207, #29743, #49011, .T. ) ;
#37814 = CARTESIAN_POINT ( 'NONE',  ( 22.73247662810271308, -183.6283474603465606, -101.5140743725395254 ) ) ;
#37815 = AXIS2_PLACEMENT_3D ( 'NONE', #24631, #48037, #24379 ) ;
#37816 = EDGE_CURVE ( 'NONE', #10170, #29823, #42804, .T. ) ;
#37817 = DIRECTION ( 'NONE',  ( -0.000000000000000000, -0.9709418174260534551, -0.2393156642875516327 ) ) ;
#37818 = DIRECTION ( 'NONE',  ( 0.000000000000000000, 0.000000000000000000, 1.000000000000000000 ) ) ;
#37819 = EDGE_CURVE ( 'NONE', #2485, #34006, #34709, .T. ) ;
#37820 = CARTESIAN_POINT ( 'NONE',  ( -170.6250538923603131, -175.3837268820161057, 26.55884942729648657 ) ) ;
#37821 = EDGE_CURVE ( 'NONE', #7849, #46212, #1162, .T. ) ;
#37822 = CARTESIAN_POINT ( 'NONE',  ( 0.000000000000000000, -63.50000000000000000, 0.000000000000000000 ) ) ;
#37823 = ORIENTED_EDGE ( 'NONE', *, *, #10451, .F. ) ;
#37824 = EDGE_CURVE ( 'NONE', #2312, #32293, #20903, .T. ) ;
#37825 = CARTESIAN_POINT ( 'NONE',  ( -339.1964088526558498, -182.0095552316575152, 7.608018572113563138 ) ) ;
#37826 = EDGE_LOOP ( 'NONE', ( #43581, #3532, #49988, #50254 ) ) ;
#37827 = EDGE_CURVE ( 'NONE', #6051, #14309, #33229, .T. ) ;
#37828 = DIRECTION ( 'NONE',  ( 0.2348860457809842095, 0.000000000000000000, -0.9720229140804107493 ) ) ;
#37829 = EDGE_CURVE ( 'NONE', #17151, #27986, #26569, .T. ) ;
#37830 = ORIENTED_EDGE ( 'NONE', *, *, #32708, .F. ) ;
#37831 = PLANE ( 'NONE',  #47706 ) ;
#37832 = AXIS2_PLACEMENT_3D ( 'NONE', #17468, #21911, #38696 ) ;
#37833 = EDGE_CURVE ( 'NONE', #21855, #10851, #18697, .T. ) ;
#37834 = VERTEX_POINT ( 'NONE', #10043 ) ;
#37835 = VECTOR ( 'NONE', #33087, 1000.000000000000000 ) ;
#37836 = DIRECTION ( 'NONE',  ( -0.7378332790417189146, 0.000000000000000000, -0.6749830015182196608 ) ) ;
#37837 = DIRECTION ( 'NONE',  ( -0.000000000000000000, -1.000000000000000000, 0.000000000000000000 ) ) ;
#37838 = VERTEX_POINT ( 'NONE', #50760 ) ;
#37841 = ORIENTED_EDGE ( 'NONE', *, *, #9974, .T. ) ;
#37840 = DIRECTION ( 'NONE',  ( 1.000000000000000000, -0.000000000000000000, -0.000000000000000000 ) ) ;
#37839 = DIRECTION ( 'NONE',  ( -0.8470055835512244613, 0.000000000000000000, -0.5315839928299663786 ) ) ;
#37842 = CARTESIAN_POINT ( 'NONE',  ( -339.1964088526558498, -66.33409060400650503, 14.60509510167813474 ) ) ;
#37843 = ORIENTED_EDGE ( 'NONE', *, *, #21576, .F. ) ;
#37844 = CARTESIAN_POINT ( 'NONE',  ( -48.47912675150885065, -175.3837268820161057, 6.938893903907228378E-15 ) ) ;
#37845 = DIRECTION ( 'NONE',  ( 1.000000000000000000, 0.000000000000000000, 0.000000000000000000 ) ) ;
#37848 = ORIENTED_EDGE ( 'NONE', *, *, #22689, .T. ) ;
#37847 = DIRECTION ( 'NONE',  ( -0.000000000000000000, 1.000000000000000000, -0.000000000000000000 ) ) ;
#37846 = DIRECTION ( 'NONE',  ( 1.000000000000000000, 0.000000000000000000, -0.000000000000000000 ) ) ;
#37849 = EDGE_CURVE ( 'NONE', #43466, #29051, #30775, .T. ) ;
#37850 = ORIENTED_EDGE ( 'NONE', *, *, #13204, .T. ) ;
#37851 = CARTESIAN_POINT ( 'NONE',  ( -339.1964088526558498, -145.2430625708868206, 55.92172413327848801 ) ) ;
#37852 = CARTESIAN_POINT ( 'NONE',  ( -49.35486169370449971, -183.6283474603465606, 0.4827922027307437469 ) ) ;
#37854 = AXIS2_PLACEMENT_3D ( 'NONE', #25359, #26122, #41124 ) ;
#37853 = CARTESIAN_POINT ( 'NONE',  ( -150.5816505765687907, -183.6283474603465606, 70.36529243996407956 ) ) ;
#37855 = VERTEX_POINT ( 'NONE', #46822 ) ;
#37856 = DIRECTION ( 'NONE',  ( 0.000000000000000000, 0.000000000000000000, -1.000000000000000000 ) ) ;
#37857 = DIRECTION ( 'NONE',  ( -0.000000000000000000, 1.000000000000000000, 0.000000000000000000 ) ) ;
#37858 = CARTESIAN_POINT ( 'NONE',  ( -336.3521761649654422, -65.12692710742291524, -8.732051761643681687 ) ) ;
#37859 = DIRECTION ( 'NONE',  ( 0.000000000000000000, 0.000000000000000000, 1.000000000000000000 ) ) ;
#37860 = ORIENTED_EDGE ( 'NONE', *, *, #11232, .T. ) ;
#37861 = CARTESIAN_POINT ( 'NONE',  ( -305.0000000000000568, -176.8578783931339444, -27.43969411971521666 ) ) ;
#37862 = CARTESIAN_POINT ( 'NONE',  ( 69.88207517204678254, -175.3837268820161057, 40.19484891390058579 ) ) ;
#37863 = EDGE_CURVE ( 'NONE', #35288, #12660, #46305, .T. ) ;
#37864 = CARTESIAN_POINT ( 'NONE',  ( 5.542374969221969039, -177.1207230881787780, 112.7238987608088365 ) ) ;
#37865 = VERTEX_POINT ( 'NONE', #22121 ) ;
#37866 = DIRECTION ( 'NONE',  ( -0.9646355819083614058, 0.000000000000000000, 0.2635871660690581320 ) ) ;
#37867 = DIRECTION ( 'NONE',  ( 0.4639789333096864810, 0.000000000000000000, 0.8858462335218260097 ) ) ;
#37868 = AXIS2_PLACEMENT_3D ( 'NONE', #20815, #28935, #29210 ) ;
#37869 = EDGE_CURVE ( 'NONE', #5856, #20143, #26826, .T. ) ;
#37870 = DIRECTION ( 'NONE',  ( -0.000000000000000000, 0.9927088740980526405, -0.1205366802553337890 ) ) ;
#37871 = EDGE_CURVE ( 'NONE', #34577, #41267, #44015, .T. ) ;
#37872 = DIRECTION ( 'NONE',  ( -0.000000000000000000, 1.000000000000000000, -0.000000000000000000 ) ) ;
#37873 = ADVANCED_FACE ( 'NONE', ( #23655 ), #11050, .F. ) ;
#37874 = EDGE_CURVE ( 'NONE', #27204, #35357, #15268, .T. ) ;
#37875 = EDGE_CURVE ( 'NONE', #47506, #26396, #33581, .T. ) ;
#37876 = VECTOR ( 'NONE', #33024, 1000.000000000000000 ) ;
#37877 = FACE_OUTER_BOUND ( 'NONE', #47266, .T. ) ;
#37878 = AXIS2_PLACEMENT_3D ( 'NONE', #51333, #2712, #19279 ) ;
#37879 = EDGE_CURVE ( 'NONE', #22697, #51897, #42857, .T. ) ;
#37880 = FACE_OUTER_BOUND ( 'NONE', #14124, .T. ) ;
#37881 = CARTESIAN_POINT ( 'NONE',  ( -62.43888699632653783, -193.5000000000000000, 124.2180546213279371 ) ) ;
#37883 = VERTEX_POINT ( 'NONE', #6864 ) ;
#37882 = PLANE ( 'NONE',  #37958 ) ;
#37884 = VERTEX_POINT ( 'NONE', #31541 ) ;
#37885 = EDGE_CURVE ( 'NONE', #12335, #41587, #22894, .T. ) ;
#37886 = ADVANCED_FACE ( 'NONE', ( #38910 ), #47598, .T. ) ;
#37887 = LINE ( 'NONE', #33688, #29655 ) ;
#37889 = VERTEX_POINT ( 'NONE', #11306 ) ;
#37888 = CARTESIAN_POINT ( 'NONE',  ( -30.48891621885992365, -193.5000000000000000, -122.6885491605229959 ) ) ;
#37890 = ORIENTED_EDGE ( 'NONE', *, *, #48074, .F. ) ;
#37891 = VECTOR ( 'NONE', #23169, 1000.000000000000000 ) ;
#37892 = EDGE_CURVE ( 'NONE', #36591, #22171, #6731, .T. ) ;
#37893 = EDGE_LOOP ( 'NONE', ( #30366, #51663, #5720, #25315 ) ) ;
#37894 = DIRECTION ( 'NONE',  ( 0.000000000000000000, 1.000000000000000000, 0.000000000000000000 ) ) ;
#37895 = ADVANCED_FACE ( 'NONE', ( #3185 ), #15530, .F. ) ;
#37896 = CARTESIAN_POINT ( 'NONE',  ( 65.38692482895591240, -183.6283474603465606, -51.57055649762701677 ) ) ;
#37897 = PLANE ( 'NONE',  #32177 ) ;
#37898 = VERTEX_POINT ( 'NONE', #24193 ) ;
#37899 = ADVANCED_FACE ( 'NONE', ( #32313 ), #28376, .F. ) ;
#37900 = DIRECTION ( 'NONE',  ( 1.000000000000000000, 0.000000000000000000, -0.000000000000000000 ) ) ;
#37901 = DIRECTION ( 'NONE',  ( 0.000000000000000000, 0.000000000000000000, 1.000000000000000000 ) ) ;
#37903 = ORIENTED_EDGE ( 'NONE', *, *, #22420, .F. ) ;
#37902 = CARTESIAN_POINT ( 'NONE',  ( 70.19984492582109681, -189.7472609257535510, 39.24667733211968823 ) ) ;
#37904 = CARTESIAN_POINT ( 'NONE',  ( -47.48307690889363641, -183.6283474603465606, -0.08879589532292464504 ) ) ;
#37905 = ORIENTED_EDGE ( 'NONE', *, *, #43337, .T. ) ;
#37906 = DIRECTION ( 'NONE',  ( 0.000000000000000000, 0.000000000000000000, 1.000000000000000000 ) ) ;
#37907 = CIRCLE ( 'NONE', #47964, 125.0000000000000000 ) ;
#37908 = EDGE_LOOP ( 'NONE', ( #19885, #13921, #28635, #47278 ) ) ;
#37909 = CARTESIAN_POINT ( 'NONE',  ( -172.7479958471414250, -183.6283474603465606, -13.49993235881364129 ) ) ;
#37910 = DIRECTION ( 'NONE',  ( -0.4031234292879792847, 0.000000000000000000, 0.9151456172430153524 ) ) ;
#37911 = CIRCLE ( 'NONE', #49662, 125.0000000000000000 ) ;
#37912 = CARTESIAN_POINT ( 'NONE',  ( -173.3968853974275817, -175.3837268820161057, 4.533605064404172325 ) ) ;
#37913 = VECTOR ( 'NONE', #46818, 1000.000000000000000 ) ;
#37914 = EDGE_CURVE ( 'NONE', #33217, #49349, #8156, .T. ) ;
#37915 = ORIENTED_EDGE ( 'NONE', *, *, #9534, .F. ) ;
#37916 = ORIENTED_EDGE ( 'NONE', *, *, #12211, .T. ) ;
#37917 = DIRECTION ( 'NONE',  ( 1.000000000000000000, -0.000000000000000000, -0.000000000000000000 ) ) ;
#37918 = CARTESIAN_POINT ( 'NONE',  ( 22.03849146056077757, -189.7472609257535510, 103.2098131075567409 ) ) ;
#37919 = VERTEX_POINT ( 'NONE', #260 ) ;
#37920 = CARTESIAN_POINT ( 'NONE',  ( -131.8938452225253855, -193.5000000000000000, 93.09664195018558530 ) ) ;
#37921 = ORIENTED_EDGE ( 'NONE', *, *, #8216, .F. ) ;
#37922 = DIRECTION ( 'NONE',  ( -1.000000000000000000, -0.000000000000000000, -0.000000000000000000 ) ) ;
#37923 = AXIS2_PLACEMENT_3D ( 'NONE', #27137, #51581, #23474 ) ;
#37924 = CARTESIAN_POINT ( 'NONE',  ( 56.81546028627040101, -193.5000000000000000, 65.49088066501711580 ) ) ;
#37925 = ORIENTED_EDGE ( 'NONE', *, *, #36716, .T. ) ;
#37926 = DIRECTION ( 'NONE',  ( -0.000000000000000000, 1.000000000000000000, -0.000000000000000000 ) ) ;
#37927 = ORIENTED_EDGE ( 'NONE', *, *, #10537, .F. ) ;
#37928 = CIRCLE ( 'NONE', #37965, 125.0000000000000000 ) ;
#37929 = VECTOR ( 'NONE', #45938, 999.9999999999998863 ) ;
#37930 = LINE ( 'NONE', #1139, #11952 ) ;
#37931 = DIRECTION ( 'NONE',  ( 0.7378332790417239107, 0.000000000000000000, 0.6749830015182142207 ) ) ;
#37932 = DIRECTION ( 'NONE',  ( -1.000000000000000000, 0.000000000000000000, 0.000000000000000000 ) ) ;
#37933 = VERTEX_POINT ( 'NONE', #40988 ) ;
#37934 = EDGE_CURVE ( 'NONE', #41945, #47761, #47018, .T. ) ;
#37935 = CARTESIAN_POINT ( 'NONE',  ( -84.85683048652069260, -189.7472609257535510, 118.5439281552633446 ) ) ;
#37936 = FACE_OUTER_BOUND ( 'NONE', #19393, .T. ) ;
#37937 = LINE ( 'NONE', #13768, #17365 ) ;
#37938 = EDGE_CURVE ( 'NONE', #32555, #41322, #20238, .T. ) ;
#37939 = LINE ( 'NONE', #19203, #22410 ) ;
#37940 = VERTEX_POINT ( 'NONE', #12346 ) ;
#37941 = PLANE ( 'NONE',  #37996 ) ;
#37942 = ORIENTED_EDGE ( 'NONE', *, *, #15951, .F. ) ;
#37943 = DIRECTION ( 'NONE',  ( 1.000000000000000000, -0.000000000000000000, 0.000000000000000000 ) ) ;
#37945 = ORIENTED_EDGE ( 'NONE', *, *, #31115, .T. ) ;
#37944 = DIRECTION ( 'NONE',  ( 0.9960498426152158968, 0.000000000000000000, 0.08879589532294571153 ) ) ;
#37946 = ORIENTED_EDGE ( 'NONE', *, *, #45131, .T. ) ;
#37947 = AXIS2_PLACEMENT_3D ( 'NONE', #16930, #32938, #16688 ) ;
#37948 = VECTOR ( 'NONE', #50687, 1000.000000000000000 ) ;
#37949 = PLANE ( 'NONE',  #47270 ) ;
#37950 = PLANE ( 'NONE',  #36514 ) ;
#37951 = EDGE_CURVE ( 'NONE', #39518, #17967, #32840, .T. ) ;
#37952 = ORIENTED_EDGE ( 'NONE', *, *, #42081, .F. ) ;
#37953 = LINE ( 'NONE', #18508, #22509 ) ;
#37954 = PLANE ( 'NONE',  #39251 ) ;
#37955 = PLANE ( 'NONE',  #37854 ) ;
#37956 = LINE ( 'NONE', #10106, #7274 ) ;
#37957 = ORIENTED_EDGE ( 'NONE', *, *, #44534, .F. ) ;
#37958 = AXIS2_PLACEMENT_3D ( 'NONE', #1882, #33928, #30003 ) ;
#37959 = EDGE_LOOP ( 'NONE', ( #46477, #37109, #45571, #165 ) ) ;
#37960 = AXIS2_PLACEMENT_3D ( 'NONE', #2751, #47420, #18787 ) ;
#37961 = ADVANCED_FACE ( 'NONE', ( #48892 ), #28630, .T. ) ;
#37962 = ORIENTED_EDGE ( 'NONE', *, *, #14675, .F. ) ;
#37963 = PLANE ( 'NONE',  #39179 ) ;
#37964 = DIRECTION ( 'NONE',  ( 0.000000000000000000, -1.000000000000000000, 0.000000000000000000 ) ) ;
#37965 = AXIS2_PLACEMENT_3D ( 'NONE', #770, #25461, #15569 ) ;
#37966 = AXIS2_PLACEMENT_3D ( 'NONE', #51363, #22975, #31625 ) ;
#37967 = DIRECTION ( 'NONE',  ( 0.000000000000000000, 0.000000000000000000, 1.000000000000000000 ) ) ;
#37968 = CARTESIAN_POINT ( 'NONE',  ( -330.4913330509368166, -181.6348283828470755, 14.84391218301019677 ) ) ;
#37969 = ORIENTED_EDGE ( 'NONE', *, *, #28632, .F. ) ;
#37970 = ORIENTED_EDGE ( 'NONE', *, *, #25103, .T. ) ;
#37972 = VERTEX_POINT ( 'NONE', #1303 ) ;
#37971 = CARTESIAN_POINT ( 'NONE',  ( -332.3517673607765914, -125.1322888500942270, -59.00000000000002132 ) ) ;
#37973 = CYLINDRICAL_SURFACE ( 'NONE', #25818, 125.0000000000000000 ) ;
#37974 = CARTESIAN_POINT ( 'NONE',  ( 50.08808042611237710, -183.6283474603465606, -76.87330921200083367 ) ) ;
#37975 = AXIS2_PLACEMENT_3D ( 'NONE', #37275, #33848, #13619 ) ;
#37976 = FACE_OUTER_BOUND ( 'NONE', #20700, .T. ) ;
#37977 = CARTESIAN_POINT ( 'NONE',  ( 76.09804998693969935, -189.7472609257535510, 10.27263529369908746 ) ) ;
#37978 = ORIENTED_EDGE ( 'NONE', *, *, #30753, .F. ) ;
#37979 = CARTESIAN_POINT ( 'NONE',  ( -55.65514169787633847, -189.7472609257535510, -123.7921848946937331 ) ) ;
#37980 = EDGE_LOOP ( 'NONE', ( #50213, #8791, #36072, #37546 ) ) ;
#37981 = VECTOR ( 'NONE', #14239, 1000.000000000000000 ) ;
#37982 = VERTEX_POINT ( 'NONE', #21023 ) ;
#37983 = DIRECTION ( 'NONE',  ( 0.8124868780056783146, 0.000000000000000000, 0.5829794791144762289 ) ) ;
#37984 = CARTESIAN_POINT ( 'NONE',  ( 0.000000000000000000, -123.5000000000002416, -59.00000000000002132 ) ) ;
#37985 = ORIENTED_EDGE ( 'NONE', *, *, #29141, .T. ) ;
#37986 = DIRECTION ( 'NONE',  ( 0.000000000000000000, -1.000000000000000000, 0.000000000000000000 ) ) ;
#37987 = DIRECTION ( 'NONE',  ( 0.000000000000000000, -0.000000000000000000, -1.000000000000000000 ) ) ;
#37988 = CARTESIAN_POINT ( 'NONE',  ( -48.47912675150885065, -189.7472609257535510, 6.938893903907228378E-15 ) ) ;
#37989 = ADVANCED_FACE ( 'NONE', ( #37043 ), #24975, .T. ) ;
#37990 = FACE_OUTER_BOUND ( 'NONE', #32983, .T. ) ;
#37991 = CIRCLE ( 'NONE', #6130, 125.0000000000000000 ) ;
#37992 = DIRECTION ( 'NONE',  ( 0.000000000000000000, 0.000000000000000000, 1.000000000000000000 ) ) ;
#37993 = DIRECTION ( 'NONE',  ( 0.000000000000000000, 0.000000000000000000, -1.000000000000000000 ) ) ;
#37994 = ORIENTED_EDGE ( 'NONE', *, *, #25974, .F. ) ;
#37995 = CIRCLE ( 'NONE', #45027, 125.0000000000000000 ) ;
#37996 = AXIS2_PLACEMENT_3D ( 'NONE', #50305, #46357, #49786 ) ;
#37997 = PLANE ( 'NONE',  #26349 ) ;
#37998 = ORIENTED_EDGE ( 'NONE', *, *, #16338, .F. ) ;
#37999 = ORIENTED_EDGE ( 'NONE', *, *, #41933, .F. ) ;
#38000 = PLANE ( 'NONE',  #22110 ) ;
#38001 = AXIS2_PLACEMENT_3D ( 'NONE', #49655, #25218, #41227 ) ;
#38002 = ORIENTED_EDGE ( 'NONE', *, *, #35486, .T. ) ;
#38003 = CYLINDRICAL_SURFACE ( 'NONE', #51163, 125.0000000000000000 ) ;
#38004 = CARTESIAN_POINT ( 'NONE',  ( 60.58466639580034041, -175.3837268820161057, -61.07445476073405644 ) ) ;
#38006 = VERTEX_POINT ( 'NONE', #1037 ) ;
#38005 = LINE ( 'NONE', #2007, #12860 ) ;
#38007 = ADVANCED_FACE ( 'NONE', ( #40716 ), #12870, .T. ) ;
#38008 = AXIS2_PLACEMENT_3D ( 'NONE', #50866, #14088, #26683 ) ;
#38009 = PLANE ( 'NONE',  #21886 ) ;
#38010 = DIRECTION ( 'NONE',  ( 1.000000000000000000, -0.000000000000000000, -0.000000000000000000 ) ) ;
#38011 = VERTEX_POINT ( 'NONE', #5265 ) ;
#38012 = ORIENTED_EDGE ( 'NONE', *, *, #50589, .T. ) ;
#38013 = AXIS2_PLACEMENT_3D ( 'NONE', #26114, #32960, #45594 ) ;
#38014 = ORIENTED_EDGE ( 'NONE', *, *, #264, .F. ) ;
#38015 = CARTESIAN_POINT ( 'NONE',  ( -330.4913330509368166, -150.4759391377553186, 52.47426709956150859 ) ) ;
#38016 = PLANE ( 'NONE',  #19286 ) ;
#38017 = DIRECTION ( 'NONE',  ( 0.000000000000000000, -0.8229838658936596829, -0.5680647467311510379 ) ) ;
#38018 = DIRECTION ( 'NONE',  ( 0.000000000000000000, 0.2393156642875516049, -0.9709418174260534551 ) ) ;
#38019 = DIRECTION ( 'NONE',  ( 0.000000000000000000, -1.000000000000000000, 0.000000000000000000 ) ) ;
#38020 = ORIENTED_EDGE ( 'NONE', *, *, #31386, .F. ) ;
#38021 = AXIS2_PLACEMENT_3D ( 'NONE', #16819, #35998, #3943 ) ;
#38022 = AXIS2_PLACEMENT_3D ( 'NONE', #47210, #30909, #27206 ) ;
#38023 = FACE_OUTER_BOUND ( 'NONE', #6575, .T. ) ;
#38024 = EDGE_LOOP ( 'NONE', ( #12518, #13755, #38238, #28304 ) ) ;
#38026 = ORIENTED_EDGE ( 'NONE', *, *, #12004, .F. ) ;
#38025 = DIRECTION ( 'NONE',  ( -0.9720229140804107493, 0.000000000000000000, -0.2348860457809842095 ) ) ;
#38027 = AXIS2_PLACEMENT_3D ( 'NONE', #42908, #47381, #51090 ) ;
#38028 = ORIENTED_EDGE ( 'NONE', *, *, #34025, .F. ) ;
#38029 = CARTESIAN_POINT ( 'NONE',  ( -8.169009709621407822, -183.6283474603465606, 118.3219948448695504 ) ) ;
#38030 = ORIENTED_EDGE ( 'NONE', *, *, #13150, .T. ) ;
#38031 = DIRECTION ( 'NONE',  ( 0.000000000000000000, -0.000000000000000000, -1.000000000000000000 ) ) ;
#38032 = VERTEX_POINT ( 'NONE', #28890 ) ;
#38033 = ADVANCED_FACE ( 'NONE', ( #36260 ), #25227, .F. ) ;
#38034 = CARTESIAN_POINT ( 'NONE',  ( -170.0000000000000284, -113.5000000000000000, 60.00000000000000711 ) ) ;
#38035 = VECTOR ( 'NONE', #48289, 1000.000000000000114 ) ;
#38036 = LINE ( 'NONE', #5752, #21722 ) ;
#38037 = VERTEX_POINT ( 'NONE', #36796 ) ;
#38038 = CARTESIAN_POINT ( 'NONE',  ( 66.03142248012328253, -177.1207230881787780, 50.12318939044040889 ) ) ;
#38039 = EDGE_LOOP ( 'NONE', ( #9990, #49370, #22938, #29140 ) ) ;
#38040 = EDGE_CURVE ( 'NONE', #33847, #728, #49149, .T. ) ;
#38041 = ORIENTED_EDGE ( 'NONE', *, *, #11714, .T. ) ;
#38042 = CARTESIAN_POINT ( 'NONE',  ( -332.3517673607765914, -152.8183901354257159, -52.34913561719022113 ) ) ;
#38043 = LINE ( 'NONE', #38816, #43218 ) ;
#38044 = PLANE ( 'NONE',  #4556 ) ;
#38045 = FACE_OUTER_BOUND ( 'NONE', #38567, .T. ) ;
#38046 = ORIENTED_EDGE ( 'NONE', *, *, #5523, .T. ) ;
#38047 = LINE ( 'NONE', #42512, #12266 ) ;
#38048 = LINE ( 'NONE', #35144, #28092 ) ;
#38049 = DIRECTION ( 'NONE',  ( 0.000000000000000000, -1.000000000000000000, 0.000000000000000000 ) ) ;
#38050 = DIRECTION ( 'NONE',  ( -1.000000000000000000, 0.000000000000000000, 0.000000000000000000 ) ) ;
#38051 = EDGE_CURVE ( 'NONE', #21480, #13363, #10070, .T. ) ;
#38052 = EDGE_LOOP ( 'NONE', ( #14918, #16670, #3749, #5583 ) ) ;
#38053 = CARTESIAN_POINT ( 'NONE',  ( 46.00000000000000711, 20.00000000000000000, -35.00000000000000000 ) ) ;
#38054 = CARTESIAN_POINT ( 'NONE',  ( -173.1763543514842070, -183.6283474603465606, 8.694908215728892387 ) ) ;
#38055 = EDGE_CURVE ( 'NONE', #7798, #41514, #44680, .T. ) ;
#38056 = VECTOR ( 'NONE', #21079, 1000.000000000000000 ) ;
#38057 = DIRECTION ( 'NONE',  ( 0.000000000000000000, -0.4647231720437695057, -0.8854560256532093554 ) ) ;
#38058 = ORIENTED_EDGE ( 'NONE', *, *, #40118, .T. ) ;
#38059 = EDGE_LOOP ( 'NONE', ( #24262, #28326, #24778, #18661 ) ) ;
#38060 = EDGE_CURVE ( 'NONE', #34311, #23737, #36519, .T. ) ;
#38061 = DIRECTION ( 'NONE',  ( 0.000000000000000000, -1.000000000000000000, 0.000000000000000000 ) ) ;
#38062 = FACE_OUTER_BOUND ( 'NONE', #50919, .T. ) ;
#38063 = ORIENTED_EDGE ( 'NONE', *, *, #47787, .T. ) ;
#38064 = ORIENTED_EDGE ( 'NONE', *, *, #33618, .F. ) ;
#38065 = AXIS2_PLACEMENT_3D ( 'NONE', #22146, #38157, #38931 ) ;
#38066 = ORIENTED_EDGE ( 'NONE', *, *, #23584, .T. ) ;
#38067 = CARTESIAN_POINT ( 'NONE',  ( -305.0000000000000568, -63.76276212672765809, 5.609136410542458151 ) ) ;
#38068 = VECTOR ( 'NONE', #41731, 1000.000000000000000 ) ;
#38069 = LINE ( 'NONE', #6805, #10272 ) ;
#38070 = CARTESIAN_POINT ( 'NONE',  ( 12.00000000000000000, 65.00000000000000000, 0.000000000000000000 ) ) ;
#38071 = EDGE_CURVE ( 'NONE', #38337, #40712, #9205, .T. ) ;
#38072 = DIRECTION ( 'NONE',  ( -8.718379230999705894E-17, -0.6631226582407863113, 0.7485107481711089639 ) ) ;
#38073 = CARTESIAN_POINT ( 'NONE',  ( -336.3521761649654422, -183.3224719910990643, -4.612141029301911388 ) ) ;
#38074 = ORIENTED_EDGE ( 'NONE', *, *, #35255, .T. ) ;
#38075 = CARTESIAN_POINT ( 'NONE',  ( 52.59568867645217694, -189.7472609257535510, -73.54509967498590584 ) ) ;
#38076 = ORIENTED_EDGE ( 'NONE', *, *, #7791, .F. ) ;
#38077 = DIRECTION ( 'NONE',  ( -0.000000000000000000, 1.000000000000000000, -0.000000000000000000 ) ) ;
#38078 = VERTEX_POINT ( 'NONE', #33378 ) ;
#38079 = CARTESIAN_POINT ( 'NONE',  ( -18.31235070009513421, -189.7472609257535510, 121.3052580173829966 ) ) ;
#38080 = VECTOR ( 'NONE', #7558, 1000.000000000000000 ) ;
#38081 = CIRCLE ( 'NONE', #4527, 125.0000000000000000 ) ;
#38082 = DIRECTION ( 'NONE',  ( 0.000000000000000000, 0.000000000000000000, -1.000000000000000000 ) ) ;
#38083 = PLANE ( 'NONE',  #28236 ) ;
#38084 = EDGE_LOOP ( 'NONE', ( #18583, #31437, #11237, #2276 ) ) ;
#38087 = VERTEX_POINT ( 'NONE', #24701 ) ;
#38086 = CARTESIAN_POINT ( 'NONE',  ( -48.47912675150885065, -183.6283474603465606, 6.938893903907228378E-15 ) ) ;
#38085 = DIRECTION ( 'NONE',  ( 0.000000000000000000, 0.000000000000000000, 1.000000000000000000 ) ) ;
#38088 = DIRECTION ( 'NONE',  ( -0.000000000000000000, -0.7485107481711046340, -0.6631226582407911962 ) ) ;
#38089 = VERTEX_POINT ( 'NONE', #26242 ) ;
#38090 = DIRECTION ( 'NONE',  ( -0.000000000000000000, 1.000000000000000000, -0.000000000000000000 ) ) ;
#38091 = ORIENTED_EDGE ( 'NONE', *, *, #19669, .T. ) ;
#38092 = EDGE_CURVE ( 'NONE', #27177, #7546, #6034, .T. ) ;
#38093 = EDGE_CURVE ( 'NONE', #4695, #12964, #22585, .T. ) ;
#38094 = CARTESIAN_POINT ( 'NONE',  ( -332.3517673607765914, -82.40546666720629787, 42.41660376256258047 ) ) ;
#38097 = VERTEX_POINT ( 'NONE', #46245 ) ;
#38096 = LINE ( 'NONE', #50216, #38241 ) ;
#38095 = DIRECTION ( 'NONE',  ( -0.000000000000000000, -0.7485107481711024136, -0.6631226582407937498 ) ) ;
#38098 = VECTOR ( 'NONE', #18705, 1000.000000000000000 ) ;
#38099 = ORIENTED_EDGE ( 'NONE', *, *, #18495, .T. ) ;
#38100 = CARTESIAN_POINT ( 'NONE',  ( 73.80528149577284580, -193.5000000000000000, 25.91377046305969145 ) ) ;
#38101 = VERTEX_POINT ( 'NONE', #38073 ) ;
#38102 = DIRECTION ( 'NONE',  ( -0.000000000000000000, 0.9350162426854146114, -0.3546048870425363986 ) ) ;
#38103 = DIRECTION ( 'NONE',  ( -0.000000000000000000, 1.000000000000000000, -0.000000000000000000 ) ) ;
#38104 = ORIENTED_EDGE ( 'NONE', *, *, #20828, .T. ) ;
#38105 = CARTESIAN_POINT ( 'NONE',  ( -167.1580984288391107, -175.3837268820161057, -39.24667733211878584 ) ) ;
#38106 = PLANE ( 'NONE',  #9043 ) ;
#38107 = CARTESIAN_POINT ( 'NONE',  ( -305.0000000000000568, -135.2893155068536828, 58.83036664750492406 ) ) ;
#38108 = CARTESIAN_POINT ( 'NONE',  ( -336.3521761649654422, -64.61288906875131488, 4.498567634385603142 ) ) ;
#38109 = ORIENTED_EDGE ( 'NONE', *, *, #96, .T. ) ;
#38110 = EDGE_CURVE ( 'NONE', #21416, #37933, #19303, .T. ) ;
#38111 = PLANE ( 'NONE',  #6998 ) ;
#38112 = LINE ( 'NONE', #10789, #18916 ) ;
#38113 = EDGE_CURVE ( 'NONE', #30709, #5333, #15139, .T. ) ;
#38114 = DIRECTION ( 'NONE',  ( 0.000000000000000000, -0.000000000000000000, -1.000000000000000000 ) ) ;
#38115 = ORIENTED_EDGE ( 'NONE', *, *, #9446, .F. ) ;
#38116 = ADVANCED_FACE ( 'NONE', ( #10475 ), #14437, .F. ) ;
#38117 = LINE ( 'NONE', #37623, #28994 ) ;
#38118 = LINE ( 'NONE', #41823, #39509 ) ;
#38119 = AXIS2_PLACEMENT_3D ( 'NONE', #33464, #49504, #16907 ) ;
#38120 = ADVANCED_FACE ( 'NONE', ( #41497 ), #49663, .F. ) ;
#38121 = VECTOR ( 'NONE', #6594, 1000.000000000000000 ) ;
#38122 = CARTESIAN_POINT ( 'NONE',  ( -132.6364218684650211, -177.1207230881787780, 92.42591454022807795 ) ) ;
#38123 = FACE_OUTER_BOUND ( 'NONE', #33215, .T. ) ;
#38124 = AXIS2_PLACEMENT_3D ( 'NONE', #39782, #48488, #32173 ) ;
#38125 = CARTESIAN_POINT ( 'NONE',  ( -336.3521761649654422, -81.08339623743702873, -41.09453333279329712 ) ) ;
#38126 = CARTESIAN_POINT ( 'NONE',  ( 30.67449672666758431, -183.6283474603465606, 95.45105364470144593 ) ) ;
#38127 = LINE ( 'NONE', #14499, #32947 ) ;
#38128 = CARTESIAN_POINT ( 'NONE',  ( 46.00000000000000711, 20.00000000000000000, -46.00000000000000000 ) ) ;
#38129 = ORIENTED_EDGE ( 'NONE', *, *, #37103, .T. ) ;
#38130 = AXIS2_PLACEMENT_3D ( 'NONE', #7779, #3845, #8307 ) ;
#38131 = DIRECTION ( 'NONE',  ( 0.6965510290629982615, 0.000000000000000000, -0.7175072570443298270 ) ) ;
#38132 = DIRECTION ( 'NONE',  ( 0.000000000000000000, 0.000000000000000000, 1.000000000000000000 ) ) ;
#38134 = ORIENTED_EDGE ( 'NONE', *, *, #8623, .T. ) ;
#38133 = PLANE ( 'NONE',  #22846 ) ;
#38135 = EDGE_LOOP ( 'NONE', ( #22663, #13099, #33034, #5810 ) ) ;
#38136 = VERTEX_POINT ( 'NONE', #50194 ) ;
#38137 = CARTESIAN_POINT ( 'NONE',  ( -26.37732090265851070, -193.5000000000000000, -122.0143860769387203 ) ) ;
#38138 = DIRECTION ( 'NONE',  ( 0.000000000000000000, -1.000000000000000000, 0.000000000000000000 ) ) ;
#38139 = LINE ( 'NONE', #38412, #22170 ) ;
#38140 = EDGE_LOOP ( 'NONE', ( #26941, #29788, #17817, #46626 ) ) ;
#38141 = ADVANCED_FACE ( 'NONE', ( #38596 ), #5527, .T. ) ;
#38142 = DIRECTION ( 'NONE',  ( -0.000000000000000000, 1.000000000000000000, -0.000000000000000000 ) ) ;
#38143 = DIRECTION ( 'NONE',  ( -0.000000000000000000, 1.000000000000000000, -0.000000000000000000 ) ) ;
#38146 = EDGE_LOOP ( 'NONE', ( #14180, #48244, #51310, #28331, #24803, #27439, #25326, #29054 ) ) ;
#38145 = DIRECTION ( 'NONE',  ( 0.000000000000000000, 0.000000000000000000, -1.000000000000000000 ) ) ;
#38144 = DIRECTION ( 'NONE',  ( -0.9960498426152158968, 0.000000000000000000, -0.08879589532294571153 ) ) ;
#38147 = LINE ( 'NONE', #26845, #28071 ) ;
#38148 = AXIS2_PLACEMENT_3D ( 'NONE', #46842, #3206, #15288 ) ;
#38149 = VERTEX_POINT ( 'NONE', #38336 ) ;
#38150 = CARTESIAN_POINT ( 'NONE',  ( -81.70897914701302511, -183.6283474603465606, -120.5021863277716676 ) ) ;
#38151 = ORIENTED_EDGE ( 'NONE', *, *, #22408, .T. ) ;
#38152 = AXIS2_PLACEMENT_3D ( 'NONE', #12585, #40429, #43862 ) ;
#38153 = EDGE_CURVE ( 'NONE', #9556, #49683, #41777, .T. ) ;
#38154 = EDGE_CURVE ( 'NONE', #38337, #42669, #2599, .T. ) ;
#38155 = EDGE_CURVE ( 'NONE', #27449, #2933, #51225, .T. ) ;
#38156 = DIRECTION ( 'NONE',  ( 0.000000000000000000, 1.000000000000000000, 0.000000000000000000 ) ) ;
#38157 = DIRECTION ( 'NONE',  ( 1.000000000000000000, -0.000000000000000000, 0.000000000000000000 ) ) ;
#38158 = FACE_OUTER_BOUND ( 'NONE', #34977, .T. ) ;
#38159 = AXIS2_PLACEMENT_3D ( 'NONE', #12126, #39718, #43685 ) ;
#38160 = ADVANCED_FACE ( 'NONE', ( #42537 ), #22308, .F. ) ;
#38161 = ORIENTED_EDGE ( 'NONE', *, *, #23614, .T. ) ;
#38162 = DIRECTION ( 'NONE',  ( -1.000000000000000000, 0.000000000000000000, 0.000000000000000000 ) ) ;
#38163 = LINE ( 'NONE', #14533, #38456 ) ;
#38164 = ORIENTED_EDGE ( 'NONE', *, *, #10466, .T. ) ;
#38165 = EDGE_CURVE ( 'NONE', #38873, #19813, #830, .T. ) ;
#38166 = CARTESIAN_POINT ( 'NONE',  ( 12.12533326292402514, -183.6283474603465606, 109.3256576763158847 ) ) ;
#38167 = ORIENTED_EDGE ( 'NONE', *, *, #19315, .T. ) ;
#38168 = FACE_BOUND ( 'NONE', #23823, .T. ) ;
#38169 = ADVANCED_FACE ( 'NONE', ( #13400 ), #41153, .T. ) ;
#38170 = VECTOR ( 'NONE', #2433, 1000.000000000000114 ) ;
#38171 = CARTESIAN_POINT ( 'NONE',  ( -170.5806857741408180, -183.6283474603465606, -21.61797988633148648 ) ) ;
#38172 = ADVANCED_FACE ( 'NONE', ( #21807 ), #17858, .F. ) ;
#38173 = PRODUCT_DEFINITION_SHAPE ( 'NONE', 'NONE',  #52051 ) ;
#38174 = VERTEX_POINT ( 'NONE', #6559 ) ;
#38175 = CARTESIAN_POINT ( 'NONE',  ( -134.7293151056888973, -175.3837268820161057, -89.08931047202572984 ) ) ;
#38176 = ORIENTED_EDGE ( 'NONE', *, *, #32348, .F. ) ;
#38177 = EDGE_CURVE ( 'NONE', #6993, #31627, #31922, .T. ) ;
#38178 = DIRECTION ( 'NONE',  ( -0.000000000000000000, 1.000000000000000000, -0.000000000000000000 ) ) ;
#38179 = CARTESIAN_POINT ( 'NONE',  ( -339.1964088526558498, -123.5000000000000284, 0.000000000000000000 ) ) ;
#38180 = VERTEX_POINT ( 'NONE', #45464 ) ;
#38181 = EDGE_CURVE ( 'NONE', #31995, #34413, #25480, .T. ) ;
#38182 = CARTESIAN_POINT ( 'NONE',  ( -126.2322430781613889, -183.6283474603465606, 97.87467957288052389 ) ) ;
#38183 = CARTESIAN_POINT ( 'NONE',  ( -150.1390659022305840, -189.7472609257535510, 72.73415134496008250 ) ) ;
#38184 = DIRECTION ( 'NONE',  ( -0.000000000000000000, 1.000000000000000000, -0.000000000000000000 ) ) ;
#38185 = ADVANCED_FACE ( 'NONE', ( #15208 ), #26768, .F. ) ;
#38186 = EDGE_LOOP ( 'NONE', ( #33815, #42907, #9068, #7755 ) ) ;
#38187 = DIRECTION ( 'NONE',  ( -0.000000000000000000, 1.000000000000000000, -0.000000000000000000 ) ) ;
#38188 = ORIENTED_EDGE ( 'NONE', *, *, #48940, .T. ) ;
#38189 = AXIS2_PLACEMENT_3D ( 'NONE', #9552, #49767, #25843 ) ;
#38190 = LINE ( 'NONE', #9383, #21937 ) ;
#38191 = DIRECTION ( 'NONE',  ( 1.000000000000000000, 0.000000000000000000, 0.000000000000000000 ) ) ;
#38193 = ORIENTED_EDGE ( 'NONE', *, *, #43336, .T. ) ;
#38192 = DIRECTION ( 'NONE',  ( -0.000000000000000000, 1.000000000000000000, -0.000000000000000000 ) ) ;
#38194 = VECTOR ( 'NONE', #5749, 1000.000000000000114 ) ;
#38195 = VECTOR ( 'NONE', #41603, 1000.000000000000000 ) ;
#38196 = ORIENTED_EDGE ( 'NONE', *, *, #30478, .F. ) ;
#38197 = CARTESIAN_POINT ( 'NONE',  ( -156.2577088867455473, -193.5000000000000000, -63.31490529818420754 ) ) ;
#38198 = EDGE_CURVE ( 'NONE', #4562, #3, #23852, .T. ) ;
#38199 = AXIS2_PLACEMENT_3D ( 'NONE', #13572, #29339, #33801 ) ;
#38200 = DIRECTION ( 'NONE',  ( -1.000000000000000000, 0.000000000000000000, 0.000000000000000000 ) ) ;
#38201 = VERTEX_POINT ( 'NONE', #2849 ) ;
#38202 = CARTESIAN_POINT ( 'NONE',  ( -47.60339180931321579, -183.6283474603465606, 0.4827922027307559594 ) ) ;
#38203 = AXIS2_PLACEMENT_3D ( 'NONE', #15691, #11976, #7785 ) ;
#38204 = VERTEX_POINT ( 'NONE', #31222 ) ;
#38205 = CARTESIAN_POINT ( 'NONE',  ( 46.00000000000000711, 0.000000000000000000, -46.00000000000000000 ) ) ;
#38206 = CARTESIAN_POINT ( 'NONE',  ( -47.66663987350317200, -189.7472609257535510, -0.5829794791144634614 ) ) ;
#38207 = CIRCLE ( 'NONE', #14699, 125.0000000000000000 ) ;
#38209 = AXIS2_PLACEMENT_3D ( 'NONE', #19236, #35243, #51294 ) ;
#38208 = DIRECTION ( 'NONE',  ( 0.000000000000000000, 1.000000000000000000, 0.000000000000000000 ) ) ;
#38210 = CARTESIAN_POINT ( 'NONE',  ( 39.18328161278952138, -175.3837268820161057, 89.10837311819237527 ) ) ;
#38211 = ORIENTED_EDGE ( 'NONE', *, *, #13327, .F. ) ;
#38212 = ORIENTED_EDGE ( 'NONE', *, *, #6717, .T. ) ;
#38213 = ORIENTED_EDGE ( 'NONE', *, *, #24342, .F. ) ;
#38214 = CIRCLE ( 'NONE', #21545, 125.0000000000000000 ) ;
#38215 = DIRECTION ( 'NONE',  ( 0.000000000000000000, 1.000000000000000000, -0.000000000000000000 ) ) ;
#38216 = LINE ( 'NONE', #22716, #9264 ) ;
#38217 = DIRECTION ( 'NONE',  ( 1.000000000000000000, -0.000000000000000000, -0.000000000000000000 ) ) ;
#38218 = DIRECTION ( 'NONE',  ( 0.000000000000000000, 1.000000000000000000, 0.000000000000000000 ) ) ;
#38219 = ORIENTED_EDGE ( 'NONE', *, *, #2099, .T. ) ;
#38220 = ADVANCED_FACE ( 'NONE', ( #42799 ), #18879, .T. ) ;
#38221 = ADVANCED_FACE ( 'NONE', ( #3897 ), #47789, .T. ) ;
#38222 = CARTESIAN_POINT ( 'NONE',  ( -332.3517673607765914, -135.0638248728647852, 57.91551518289418254 ) ) ;
#38223 = EDGE_CURVE ( 'NONE', #44250, #16764, #10744, .T. ) ;
#38224 = EDGE_CURVE ( 'NONE', #33858, #28909, #14964, .T. ) ;
#38225 = EDGE_LOOP ( 'NONE', ( #51610, #33900, #43584, #30455 ) ) ;
#38227 = ORIENTED_EDGE ( 'NONE', *, *, #32422, .T. ) ;
#38226 = DIRECTION ( 'NONE',  ( 1.000000000000000000, 0.000000000000000000, 0.000000000000000000 ) ) ;
#38228 = VECTOR ( 'NONE', #49463, 1000.000000000000227 ) ;
#38229 = CARTESIAN_POINT ( 'NONE',  ( -45.06671089634843952, -177.1207230881787780, -124.9534129907280402 ) ) ;
#38230 = LINE ( 'NONE', #46652, #17421 ) ;
#38231 = AXIS2_PLACEMENT_3D ( 'NONE', #6136, #17705, #29762 ) ;
#38232 = AXIS2_PLACEMENT_3D ( 'NONE', #18933, #14740, #30249 ) ;
#38233 = DIRECTION ( 'NONE',  ( -0.000000000000000000, 0.000000000000000000, 1.000000000000000000 ) ) ;
#38234 = FACE_OUTER_BOUND ( 'NONE', #20559, .T. ) ;
#38235 = ORIENTED_EDGE ( 'NONE', *, *, #14542, .F. ) ;
#38236 = DIRECTION ( 'NONE',  ( 0.000000000000000000, 0.000000000000000000, -1.000000000000000000 ) ) ;
#38237 = VERTEX_POINT ( 'NONE', #30969 ) ;
#38238 = ORIENTED_EDGE ( 'NONE', *, *, #30513, .F. ) ;
#38239 = PLANE ( 'NONE',  #17027 ) ;
#38240 = EDGE_CURVE ( 'NONE', #34311, #18605, #48707, .T. ) ;
#38241 = VECTOR ( 'NONE', #29439, 1000.000000000000000 ) ;
#38242 = CARTESIAN_POINT ( 'NONE',  ( -55.05561436132770581, -189.7472609257535510, 124.8268793598474105 ) ) ;
#38243 = ORIENTED_EDGE ( 'NONE', *, *, #38071, .F. ) ;
#38244 = VECTOR ( 'NONE', #38245, 1000.000000000000114 ) ;
#38245 = DIRECTION ( 'NONE',  ( -0.5085311186492094127, 0.000000000000000000, -0.8610436117673619938 ) ) ;
#38246 = DIRECTION ( 'NONE',  ( 0.000000000000000000, 0.000000000000000000, 1.000000000000000000 ) ) ;
#38247 = DIRECTION ( 'NONE',  ( 0.000000000000000000, 0.5680647467311485954, -0.8229838658936613482 ) ) ;
#38248 = CIRCLE ( 'NONE', #29012, 60.00000000000000000 ) ;
#38249 = DIRECTION ( 'NONE',  ( 0.000000000000000000, 0.9709418174260511236, -0.2393156642875615969 ) ) ;
#38250 = EDGE_CURVE ( 'NONE', #27224, #51897, #12602, .T. ) ;
#38252 = AXIS2_PLACEMENT_3D ( 'NONE', #39511, #16393, #31632 ) ;
#38251 = FACE_OUTER_BOUND ( 'NONE', #28387, .T. ) ;
#38253 = ORIENTED_EDGE ( 'NONE', *, *, #12827, .F. ) ;
#38254 = DIRECTION ( 'NONE',  ( -0.000000000000000000, 1.000000000000000000, -0.000000000000000000 ) ) ;
#38255 = VERTEX_POINT ( 'NONE', #47013 ) ;
#38256 = ORIENTED_EDGE ( 'NONE', *, *, #25017, .F. ) ;
#38257 = DIRECTION ( 'NONE',  ( -1.000000000000000000, 0.000000000000000000, 0.000000000000000000 ) ) ;
#38258 = ORIENTED_EDGE ( 'NONE', *, *, #27828, .F. ) ;
#38259 = DIRECTION ( 'NONE',  ( 1.000000000000000000, -0.000000000000000000, -0.000000000000000000 ) ) ;
#38260 = VECTOR ( 'NONE', #27001, 1000.000000000000000 ) ;
#38261 = VECTOR ( 'NONE', #50420, 1000.000000000000000 ) ;
#38262 = DIRECTION ( 'NONE',  ( 0.000000000000000000, -1.000000000000000000, -0.000000000000000000 ) ) ;
#38263 = DIRECTION ( 'NONE',  ( 0.000000000000000000, -1.000000000000000000, 0.000000000000000000 ) ) ;
#38264 = ORIENTED_EDGE ( 'NONE', *, *, #13077, .F. ) ;
#38265 = PLANE ( 'NONE',  #39221 ) ;
#38266 = CIRCLE ( 'NONE', #45008, 125.0000000000000000 ) ;
#38267 = AXIS2_PLACEMENT_3D ( 'NONE', #36780, #24682, #36001 ) ;
#38268 = DIRECTION ( 'NONE',  ( 0.4827922027307490205, 0.000000000000000000, -0.8757349421956345248 ) ) ;
#38269 = DIRECTION ( 'NONE',  ( -0.4031234292879792847, 0.000000000000000000, 0.9151456172430153524 ) ) ;
#38270 = EDGE_LOOP ( 'NONE', ( #2797, #19579, #35734, #13924 ) ) ;
#38271 = ORIENTED_EDGE ( 'NONE', *, *, #11888, .T. ) ;
#38272 = ORIENTED_EDGE ( 'NONE', *, *, #12642, .T. ) ;
#38273 = CARTESIAN_POINT ( 'NONE',  ( -7.223120065443615623, -177.1207230881787780, 117.9955164924470523 ) ) ;
#38274 = DIRECTION ( 'NONE',  ( 0.000000000000000000, -1.000000000000000000, -0.000000000000000000 ) ) ;
#38275 = VECTOR ( 'NONE', #660, 1000.000000000000000 ) ;
#38276 = FILL_AREA_STYLE ('',( #6234 ) ) ;
#38277 = AXIS2_PLACEMENT_3D ( 'NONE', #9826, #42389, #22434 ) ;
#38279 = COLOUR_RGB ( '', 0.72549020, 0.75294118, 0.79215686) ;
#38278 = CARTESIAN_POINT ( 'NONE',  ( -165.8930023212105596, -189.7472609257535510, -39.87457906003690766 ) ) ;
#38280 = LINE ( 'NONE', #34089, #7057 ) ;
#38281 = ORIENTED_EDGE ( 'NONE', *, *, #13687, .T. ) ;
#38282 = EDGE_CURVE ( 'NONE', #25951, #51005, #41975, .T. ) ;
#38283 = VECTOR ( 'NONE', #11547, 1000.000000000000000 ) ;
#38284 = AXIS2_PLACEMENT_3D ( 'NONE', #51392, #26934, #51919 ) ;
#38285 = FACE_OUTER_BOUND ( 'NONE', #7913, .T. ) ;
#38286 = VERTEX_POINT ( 'NONE', #39609 ) ;
#38288 = VERTEX_POINT ( 'NONE', #43056 ) ;
#38287 = CARTESIAN_POINT ( 'NONE',  ( -48.47912675150885065, -183.6283474603465606, 6.938893903907228378E-15 ) ) ;
#38289 = ORIENTED_EDGE ( 'NONE', *, *, #28231, .T. ) ;
#38290 = DIRECTION ( 'NONE',  ( 0.000000000000000000, -0.000000000000000000, 1.000000000000000000 ) ) ;
#38291 = ORIENTED_EDGE ( 'NONE', *, *, #11182, .T. ) ;
#38292 = PLANE ( 'NONE',  #37547 ) ;
#38293 = ORIENTED_EDGE ( 'NONE', *, *, #37513, .F. ) ;
#38294 = DIRECTION ( 'NONE',  ( 0.000000000000000000, -0.9927088740980553050, -0.1205366802553130001 ) ) ;
#38295 = CARTESIAN_POINT ( 'NONE',  ( -47.60339180931321579, -193.5000000000000000, -0.4827922027307358088 ) ) ;
#38296 = ORIENTED_EDGE ( 'NONE', *, *, #11614, .F. ) ;
#38297 = FACE_OUTER_BOUND ( 'NONE', #3651, .T. ) ;
#38298 = ORIENTED_EDGE ( 'NONE', *, *, #19282, .F. ) ;
#38299 = PRODUCT_DEFINITION ( 'UNKNOWN', '', #3242, #19544 ) ;
#38300 = ORIENTED_EDGE ( 'NONE', *, *, #50605, .F. ) ;
#38301 = CARTESIAN_POINT ( 'NONE',  ( 70.98542830588607444, -183.6283474603465606, -36.78613984829962646 ) ) ;
#38302 = AXIS2_PLACEMENT_3D ( 'NONE', #39349, #36178, #51206 ) ;
#38303 = DIRECTION ( 'NONE',  ( -0.000000000000000000, 1.047444401652940007E-14, 1.000000000000000000 ) ) ;
#38304 = CIRCLE ( 'NONE', #49239, 125.0000000000000000 ) ;
#38305 = EDGE_CURVE ( 'NONE', #48694, #16051, #3622, .T. ) ;
#38306 = DIRECTION ( 'NONE',  ( -0.9473263538541946138, 0.000000000000000000, 0.3202698538628279690 ) ) ;
#38307 = DIRECTION ( 'NONE',  ( 0.000000000000000000, 0.000000000000000000, 1.000000000000000000 ) ) ;
#38308 = VERTEX_POINT ( 'NONE', #7063 ) ;
#38309 = DIRECTION ( 'NONE',  ( 1.000000000000000000, 0.000000000000000000, -0.000000000000000000 ) ) ;
#38310 = LINE ( 'NONE', #50421, #5472 ) ;
#38311 = VECTOR ( 'NONE', #42490, 1000.000000000000000 ) ;
#38312 = CONTEXT_DEPENDENT_SHAPE_REPRESENTATION ( #26368, #38173 ) ;
#38313 = PLANE ( 'NONE',  #28855 ) ;
#38314 = DIRECTION ( 'NONE',  ( 0.000000000000000000, -0.8229838658936494689, 0.5680647467311658039 ) ) ;
#38315 = VERTEX_POINT ( 'NONE', #51734 ) ;
#38316 = CARTESIAN_POINT ( 'NONE',  ( -160.9694636715425702, -193.5000000000000000, 54.50618404931040573 ) ) ;
#38317 = LINE ( 'NONE', #18097, #35787 ) ;
#38318 = DIRECTION ( 'NONE',  ( 0.000000000000000000, 0.8854560256532093554, -0.4647231720437695057 ) ) ;
#38319 = ORIENTED_EDGE ( 'NONE', *, *, #902, .F. ) ;
#38320 = AXIS2_PLACEMENT_3D ( 'NONE', #7775, #3838, #7527 ) ;
#38321 = AXIS2_PLACEMENT_3D ( 'NONE', #23888, #36234, #32561 ) ;
#38322 = DIRECTION ( 'NONE',  ( 0.000000000000000000, -1.000000000000000000, 0.000000000000000000 ) ) ;
#38323 = AXIS2_PLACEMENT_3D ( 'NONE', #16910, #8238, #31891 ) ;
#38324 = VECTOR ( 'NONE', #46726, 1000.000000000000000 ) ;
#38325 = DIRECTION ( 'NONE',  ( 0.000000000000000000, -0.000000000000000000, -1.000000000000000000 ) ) ;
#38326 = VERTEX_POINT ( 'NONE', #35680 ) ;
#38327 = CARTESIAN_POINT ( 'NONE',  ( -48.53836737940257251, -193.5000000000000000, 0.9982437317643279018 ) ) ;
#38328 = EDGE_CURVE ( 'NONE', #24446, #5479, #39867, .T. ) ;
#38329 = VECTOR ( 'NONE', #32971, 1000.000000000000000 ) ;
#38330 = ORIENTED_EDGE ( 'NONE', *, *, #5070, .F. ) ;
#38331 = VECTOR ( 'NONE', #35768, 1000.000000000000000 ) ;
#38332 = CARTESIAN_POINT ( 'NONE',  ( -330.4913330509368166, -124.0000000000001990, -59.00000000000002132 ) ) ;
#38333 = DIRECTION ( 'NONE',  ( 0.1768902751225733261, 0.000000000000000000, -0.9842305779475966077 ) ) ;
#38334 = CARTESIAN_POINT ( 'NONE',  ( 75.21854001195777073, -183.6283474603465606, -8.665274887905439982 ) ) ;
#38335 = FACE_OUTER_BOUND ( 'NONE', #30177, .T. ) ;
#38336 = CARTESIAN_POINT ( 'NONE',  ( -159.8192355313504720, -177.1207230881787780, -56.81883646197830018 ) ) ;
#38337 = VERTEX_POINT ( 'NONE', #14688 ) ;
#38338 = CARTESIAN_POINT ( 'NONE',  ( 59.70893145360469845, -193.5000000000000000, -60.59166255800332124 ) ) ;
#38339 = EDGE_CURVE ( 'NONE', #19412, #30840, #15740, .T. ) ;
#38340 = ORIENTED_EDGE ( 'NONE', *, *, #51713, .T. ) ;
#38341 = CARTESIAN_POINT ( 'NONE',  ( -332.3517673607765914, -86.34605966037949543, -45.90766452162698386 ) ) ;
#38342 = VECTOR ( 'NONE', #5116, 1000.000000000000227 ) ;
#38343 = VECTOR ( 'NONE', #19698, 1000.000000000000000 ) ;
#38344 = ORIENTED_EDGE ( 'NONE', *, *, #31761, .T. ) ;
#38345 = CARTESIAN_POINT ( 'NONE',  ( 44.30815888362531041, -193.5000000000000000, 83.75869879877569701 ) ) ;
#38346 = VECTOR ( 'NONE', #39727, 1000.000000000000114 ) ;
#38347 = ADVANCED_FACE ( 'NONE', ( #7326 ), #3113, .T. ) ;
#38348 = CARTESIAN_POINT ( 'NONE',  ( -332.3517673607765914, -136.0347666902908372, 57.67619951860663718 ) ) ;
#38349 = DIRECTION ( 'NONE',  ( 0.3482016354343928088, 0.000000000000000000, 0.9374196611341231167 ) ) ;
#38350 = EDGE_LOOP ( 'NONE', ( #10447, #35325, #36215, #4210 ) ) ;
#38353 = ORIENTED_EDGE ( 'NONE', *, *, #24088, .T. ) ;
#38352 = DIRECTION ( 'NONE',  ( 0.000000000000000000, 1.000000000000000000, -0.000000000000000000 ) ) ;
#38351 = CARTESIAN_POINT ( 'NONE',  ( -305.0000000000000568, -95.17484985463120495, 52.89315522108991985 ) ) ;
#38354 = VECTOR ( 'NONE', #50578, 1000.000000000000000 ) ;
#38355 = EDGE_CURVE ( 'NONE', #5823, #37898, #46756, .T. ) ;
#38356 = VECTOR ( 'NONE', #33707, 1000.000000000000114 ) ;
#38357 = CARTESIAN_POINT ( 'NONE',  ( 59.29945538372744807, -193.5000000000000000, 63.31490529818492519 ) ) ;
#38359 = ORIENTED_EDGE ( 'NONE', *, *, #46613, .T. ) ;
#38358 = CIRCLE ( 'NONE', #23261, 125.0000000000000000 ) ;
#38360 = CARTESIAN_POINT ( 'NONE',  ( -154.2693405752510500, -175.3837268820161057, 66.58401203837831872 ) ) ;
#38361 = EDGE_LOOP ( 'NONE', ( #6949, #50090, #50017, #41970 ) ) ;
#38362 = AXIS2_PLACEMENT_3D ( 'NONE', #33455, #8227, #25295 ) ;
#38363 = CARTESIAN_POINT ( 'NONE',  ( 67.29469129333651267, -193.5000000000000000, -44.41421852208627286 ) ) ;
#38366 = EDGE_LOOP ( 'NONE', ( #38537, #34856, #1896, #46059 ) ) ;
#38365 = FACE_OUTER_BOUND ( 'NONE', #38361, .T. ) ;
#38364 = FACE_OUTER_BOUND ( 'NONE', #32361, .T. ) ;
#38367 = ORIENTED_EDGE ( 'NONE', *, *, #39404, .F. ) ;
#38368 = VECTOR ( 'NONE', #25769, 1000.000000000000114 ) ;
#38369 = CARTESIAN_POINT ( 'NONE',  ( -144.6608085595393902, -175.3837268820161057, -78.26291788638665992 ) ) ;
#38370 = EDGE_LOOP ( 'NONE', ( #2302, #29632, #43877, #22544 ) ) ;
#38371 = FACE_OUTER_BOUND ( 'NONE', #31570, .T. ) ;
#38372 = CARTESIAN_POINT ( 'NONE',  ( -52.47502265695602119, -193.5000000000000000, -123.9361149384469485 ) ) ;
#38373 = EDGE_LOOP ( 'NONE', ( #22863, #35823, #41588, #13045 ) ) ;
#38374 = EDGE_CURVE ( 'NONE', #15492, #37383, #47275, .T. ) ;
#38375 = CARTESIAN_POINT ( 'NONE',  ( -332.3517673607765914, -180.1556192733800117, 16.67542351306693149 ) ) ;
#38376 = DIRECTION ( 'NONE',  ( -0.000000000000000000, 1.000000000000000000, -0.000000000000000000 ) ) ;
#38377 = DIRECTION ( 'NONE',  ( 0.6300878435817038881, 0.000000000000000000, 0.7765238627180482966 ) ) ;
#38378 = LINE ( 'NONE', #18672, #49498 ) ;
#38379 = FACE_OUTER_BOUND ( 'NONE', #1943, .T. ) ;
#38380 = VERTEX_POINT ( 'NONE', #20428 ) ;
#38381 =( LENGTH_UNIT ( ) NAMED_UNIT ( * ) SI_UNIT ( .MILLI., .METRE. ) );
#38382 = PLANE ( 'NONE',  #11187 ) ;
#38383 = CARTESIAN_POINT ( 'NONE',  ( -332.3517673607765914, -159.1821513111375452, -47.06073758877369073 ) ) ;
#38384 = DIRECTION ( 'NONE',  ( 0.000000000000000000, -1.000000000000000000, 0.000000000000000000 ) ) ;
#38385 = EDGE_LOOP ( 'NONE', ( #50283, #19636, #51562, #49806 ) ) ;
#38386 = AXIS2_PLACEMENT_3D ( 'NONE', #40877, #4900, #12750 ) ;
#38387 = VECTOR ( 'NONE', #37872, 1000.000000000000000 ) ;
#38388 = LINE ( 'NONE', #39156, #15589 ) ;
#38389 = PLANE ( 'NONE',  #31149 ) ;
#38390 = VECTOR ( 'NONE', #40323, 1000.000000000000000 ) ;
#38391 = DIRECTION ( 'NONE',  ( -0.000000000000000000, 1.000000000000000000, -0.000000000000000000 ) ) ;
#38392 = DIRECTION ( 'NONE',  ( -0.000000000000000000, 1.000000000000000000, -0.000000000000000000 ) ) ;
#38393 = ORIENTED_EDGE ( 'NONE', *, *, #20745, .T. ) ;
#38394 = CARTESIAN_POINT ( 'NONE',  ( 43.18784210722336070, -189.7472609257535510, -84.98333260264753619 ) ) ;
#38395 = AXIS2_PLACEMENT_3D ( 'NONE', #7255, #10680, #50124 ) ;
#38396 = CARTESIAN_POINT ( 'NONE',  ( -336.3521761649654422, -106.8245764869328980, 56.65561927337994064 ) ) ;
#38397 = CARTESIAN_POINT ( 'NONE',  ( -339.1964088526558498, -182.0095552316576573, -7.608018572112655420 ) ) ;
#38398 = DIRECTION ( 'NONE',  ( -0.4566292373937140270, 0.000000000000000000, 0.8896570909947467687 ) ) ;
#38399 = ORIENTED_EDGE ( 'NONE', *, *, #31335, .F. ) ;
#38400 = EDGE_CURVE ( 'NONE', #30050, #38380, #40644, .T. ) ;
#38401 = EDGE_CURVE ( 'NONE', #48252, #22804, #31994, .T. ) ;
#38402 = AXIS2_PLACEMENT_3D ( 'NONE', #21845, #38376, #5831 ) ;
#38403 = CYLINDRICAL_SURFACE ( 'NONE', #1698, 125.0000000000000000 ) ;
#38404 = VECTOR ( 'NONE', #36529, 1000.000000000000000 ) ;
#38405 = CARTESIAN_POINT ( 'NONE',  ( 46.00000000000000711, 0.000000000000000000, -51.00000000000000000 ) ) ;
#38406 = ORIENTED_EDGE ( 'NONE', *, *, #33392, .F. ) ;
#38407 = EDGE_LOOP ( 'NONE', ( #27191, #37311, #15960, #43835 ) ) ;
#38408 = ORIENTED_EDGE ( 'NONE', *, *, #51229, .F. ) ;
#38409 = PLANE ( 'NONE',  #18335 ) ;
#38410 = EDGE_CURVE ( 'NONE', #41514, #21292, #33619, .T. ) ;
#38411 = DIRECTION ( 'NONE',  ( 0.4300652022765115712, 0.000000000000000000, 0.9027978299657477557 ) ) ;
#38412 = CARTESIAN_POINT ( 'NONE',  ( -148.6149069237406195, -193.5000000000000000, -74.81861753132355375 ) ) ;
#38413 = EDGE_LOOP ( 'NONE', ( #39246, #8723, #37058, #4208 ) ) ;
#38414 = EDGE_CURVE ( 'NONE', #2676, #8596, #12550, .T. ) ;
#38415 = PLANE ( 'NONE',  #20834 ) ;
#38416 = APPLICATION_CONTEXT ( 'automotive_design' ) ;
#38417 = LINE ( 'NONE', #50000, #36144 ) ;
#38418 = AXIS2_PLACEMENT_3D ( 'NONE', #11145, #22487, #3278 ) ;
#38421 = EDGE_LOOP ( 'NONE', ( #20614, #17755, #12697, #7130 ) ) ;
#38420 = DIRECTION ( 'NONE',  ( -8.718379230999705894E-17, 0.6631226582407911962, -0.7485107481711046340 ) ) ;
#38419 = CARTESIAN_POINT ( 'NONE',  ( 69.88207517204678254, -193.5000000000000000, 40.19484891390058579 ) ) ;
#38422 = CIRCLE ( 'NONE', #15790, 125.0000000000000000 ) ;
#38423 = ADVANCED_FACE ( 'NONE', ( #28045 ), #49074, .F. ) ;
#38424 = LINE ( 'NONE', #34228, #11305 ) ;
#38425 = ORIENTED_EDGE ( 'NONE', *, *, #36090, .F. ) ;
#38426 = DIRECTION ( 'NONE',  ( 0.000000000000000000, 0.000000000000000000, 1.000000000000000000 ) ) ;
#38427 = VECTOR ( 'NONE', #18509, 1000.000000000000000 ) ;
#38428 = EDGE_CURVE ( 'NONE', #14578, #16046, #36450, .T. ) ;
#38429 = ORIENTED_EDGE ( 'NONE', *, *, #38055, .T. ) ;
#38430 = FACE_OUTER_BOUND ( 'NONE', #41399, .T. ) ;
#38431 = DIRECTION ( 'NONE',  ( -0.000000000000000000, 1.000000000000000000, -0.000000000000000000 ) ) ;
#38432 = PLANE ( 'NONE',  #23225 ) ;
#38433 = AXIS2_PLACEMENT_3D ( 'NONE', #1166, #37433, #13784 ) ;
#38434 = VERTEX_POINT ( 'NONE', #44367 ) ;
#38435 = LINE ( 'NONE', #31058, #23972 ) ;
#38436 = CARTESIAN_POINT ( 'NONE',  ( -11.47118876952528765, -175.3837268820161057, 118.3487137068149053 ) ) ;
#38437 = VERTEX_POINT ( 'NONE', #5200 ) ;
#38438 = FACE_OUTER_BOUND ( 'NONE', #30606, .T. ) ;
#38439 = LINE ( 'NONE', #30543, #50859 ) ;
#38440 = ORIENTED_EDGE ( 'NONE', *, *, #27890, .F. ) ;
#38441 = FACE_BOUND ( 'NONE', #48092, .T. ) ;
#38442 = CARTESIAN_POINT ( 'NONE',  ( 45.66222513722992460, -177.1207230881787780, 80.70646587903453906 ) ) ;
#38443 = AXIS2_PLACEMENT_3D ( 'NONE', #42045, #5820, #46017 ) ;
#38444 = EDGE_LOOP ( 'NONE', ( #37721, #43393, #16379, #41404 ) ) ;
#38445 = DIRECTION ( 'NONE',  ( 0.000000000000000000, 0.000000000000000000, 1.000000000000000000 ) ) ;
#38446 = ORIENTED_EDGE ( 'NONE', *, *, #35267, .F. ) ;
#38447 = DIRECTION ( 'NONE',  ( 0.000000000000000000, 0.000000000000000000, 1.000000000000000000 ) ) ;
#38448 = DIRECTION ( 'NONE',  ( -0.000000000000000000, -0.8229838658936596829, -0.5680647467311510379 ) ) ;
#38449 = ORIENTED_EDGE ( 'NONE', *, *, #34946, .F. ) ;
#38450 = LINE ( 'NONE', #38953, #43313 ) ;
#38451 = DIRECTION ( 'NONE',  ( 0.000000000000000000, 1.000000000000000000, 0.000000000000000000 ) ) ;
#38452 = DIRECTION ( 'NONE',  ( 0.000000000000000000, 0.000000000000000000, -1.000000000000000000 ) ) ;
#38453 = VERTEX_POINT ( 'NONE', #36984 ) ;
#38454 = CARTESIAN_POINT ( 'NONE',  ( -102.5006284722404502, -193.5000000000000000, -112.7238987608084386 ) ) ;
#38455 = ORIENTED_EDGE ( 'NONE', *, *, #30458, .T. ) ;
#38456 = VECTOR ( 'NONE', #31060, 1000.000000000000000 ) ;
#38457 = AXIS2_PLACEMENT_3D ( 'NONE', #16744, #944, #31717 ) ;
#38458 =( GEOMETRIC_REPRESENTATION_CONTEXT ( 3 ) GLOBAL_UNCERTAINTY_ASSIGNED_CONTEXT ( ( #35314 ) ) GLOBAL_UNIT_ASSIGNED_CONTEXT ( ( #5277, #41789, #21561 ) ) REPRESENTATION_CONTEXT ( 'NONE', 'WORKASPACE' ) );
#38459 = LINE ( 'NONE', #18749, #1784 ) ;
#38460 = PLANE ( 'NONE',  #22653 ) ;
#38462 = ORIENTED_EDGE ( 'NONE', *, *, #10752, .T. ) ;
#38461 = LINE ( 'NONE', #46113, #22059 ) ;
#38463 = VECTOR ( 'NONE', #47859, 1000.000000000000000 ) ;
#38464 = EDGE_CURVE ( 'NONE', #45486, #34708, #5080, .T. ) ;
#38465 = VERTEX_POINT ( 'NONE', #8355 ) ;
#38466 = EDGE_CURVE ( 'NONE', #46293, #4438, #32523, .T. ) ;
#38467 = ADVANCED_FACE ( 'NONE', ( #193 ), #9140, .T. ) ;
#38468 = CARTESIAN_POINT ( 'NONE',  ( -47.49008656418669005, -183.6283474603465606, -0.1476465640024710591 ) ) ;
#38469 = EDGE_CURVE ( 'NONE', #38948, #6177, #51999, .T. ) ;
#38470 = CARTESIAN_POINT ( 'NONE',  ( 60.00000000000001421, 20.00000000000000000, 60.00000000000000711 ) ) ;
#38471 = AXIS2_PLACEMENT_3D ( 'NONE', #14967, #22590, #47537 ) ;
#38472 = VERTEX_POINT ( 'NONE', #29089 ) ;
#38473 = CARTESIAN_POINT ( 'NONE',  ( -99.62791064391784346, -189.7472609257535510, -114.0561348912352173 ) ) ;
#38474 = EDGE_CURVE ( 'NONE', #23514, #22228, #16776, .T. ) ;
#38475 = EDGE_LOOP ( 'NONE', ( #6487, #17536, #4885, #39139 ) ) ;
#38476 = CARTESIAN_POINT ( 'NONE',  ( -339.1964088526558498, -71.02573290043838483, 26.97593913775504504 ) ) ;
#38477 = CARTESIAN_POINT ( 'NONE',  ( -336.3521761649653854, -182.1255794688777314, -12.76876783163924323 ) ) ;
#38478 = EDGE_CURVE ( 'NONE', #16432, #44450, #32783, .T. ) ;
#38479 = ADVANCED_FACE ( 'NONE', ( #32252 ), #24905, .F. ) ;
#38480 = DIRECTION ( 'NONE',  ( -0.4300652022765304450, 0.000000000000000000, 0.9027978299657387629 ) ) ;
#38481 = DIRECTION ( 'NONE',  ( 0.000000000000000000, 0.000000000000000000, -1.000000000000000000 ) ) ;
#38482 = VERTEX_POINT ( 'NONE', #44872 ) ;
#38483 = ORIENTED_EDGE ( 'NONE', *, *, #51228, .T. ) ;
#38484 = EDGE_CURVE ( 'NONE', #18044, #33115, #51265, .T. ) ;
#38485 = EDGE_LOOP ( 'NONE', ( #6399, #33362, #10860, #30516 ) ) ;
#38486 = AXIS2_PLACEMENT_3D ( 'NONE', #47815, #50987, #2873 ) ;
#38487 = DIRECTION ( 'NONE',  ( 0.000000000000000000, 0.000000000000000000, 1.000000000000000000 ) ) ;
#38488 = PLANE ( 'NONE',  #5061 ) ;
#38489 = EDGE_CURVE ( 'NONE', #23416, #46482, #15987, .T. ) ;
#38490 = PLANE ( 'NONE',  #25369 ) ;
#38491 = DIRECTION ( 'NONE',  ( 0.000000000000000000, 0.000000000000000000, 1.000000000000000000 ) ) ;
#38492 = ORIENTED_EDGE ( 'NONE', *, *, #26836, .F. ) ;
#38493 = EDGE_CURVE ( 'NONE', #40406, #9307, #976, .T. ) ;
#38494 = UNCERTAINTY_MEASURE_WITH_UNIT (LENGTH_MEASURE( 1.000000000000000082E-05 ), #51007, 'distance_accuracy_value', 'NONE');
#38495 = LINE ( 'NONE', #32150, #40793 ) ;
#38496 = EDGE_CURVE ( 'NONE', #2507, #26071, #13062, .T. ) ;
#38497 = ORIENTED_EDGE ( 'NONE', *, *, #22700, .F. ) ;
#38498 = ORIENTED_EDGE ( 'NONE', *, *, #9284, .F. ) ;
#38499 = AXIS2_PLACEMENT_3D ( 'NONE', #23383, #35456, #23632 ) ;
#38500 = AXIS2_PLACEMENT_3D ( 'NONE', #19319, #35330, #43488 ) ;
#38501 = CARTESIAN_POINT ( 'NONE',  ( -330.4913330509368166, -79.00630452878473875, -38.74998146212148953 ) ) ;
#38502 = PLANE ( 'NONE',  #40925 ) ;
#38503 = LINE ( 'NONE', #33530, #22475 ) ;
#38504 = VECTOR ( 'NONE', #16248, 1000.000000000000000 ) ;
#38505 = PLANE ( 'NONE',  #32099 ) ;
#38506 = FACE_OUTER_BOUND ( 'NONE', #6216, .T. ) ;
#38507 = EDGE_LOOP ( 'NONE', ( #21980, #12885, #16113, #30522 ) ) ;
#38508 = CARTESIAN_POINT ( 'NONE',  ( -59.86929868745821182, -193.5000000000000000, -124.4799742258549600 ) ) ;
#38509 = ADVANCED_FACE ( 'NONE', ( #34339 ), #38009, .F. ) ;
#38510 = ORIENTED_EDGE ( 'NONE', *, *, #47048, .F. ) ;
#38511 = PLANE ( 'NONE',  #38008 ) ;
#38512 = AXIS2_PLACEMENT_3D ( 'NONE', #17799, #25934, #41710 ) ;
#38513 = DIRECTION ( 'NONE',  ( 0.000000000000000000, 0.000000000000000000, 1.000000000000000000 ) ) ;
#38514 = ORIENTED_EDGE ( 'NONE', *, *, #24633, .F. ) ;
#38515 = LINE ( 'NONE', #10657, #13119 ) ;
#38516 = FACE_OUTER_BOUND ( 'NONE', #10669, .T. ) ;
#38517 = PLANE ( 'NONE',  #7238 ) ;
#38518 = DIRECTION ( 'NONE',  ( 0.000000000000000000, 0.000000000000000000, -1.000000000000000000 ) ) ;
#38519 = CIRCLE ( 'NONE', #48584, 125.0000000000000000 ) ;
#38520 = DIRECTION ( 'NONE',  ( 0.000000000000000000, 1.000000000000000000, 0.000000000000000000 ) ) ;
#38521 = EDGE_CURVE ( 'NONE', #20194, #24508, #45377, .T. ) ;
#38522 = ORIENTED_EDGE ( 'NONE', *, *, #29205, .T. ) ;
#38523 = DIRECTION ( 'NONE',  ( 0.000000000000000000, -0.6631226582408016323, -0.7485107481710953081 ) ) ;
#38524 = ORIENTED_EDGE ( 'NONE', *, *, #38040, .T. ) ;
#38525 = EDGE_CURVE ( 'NONE', #49884, #18723, #50128, .T. ) ;
#38526 = ORIENTED_EDGE ( 'NONE', *, *, #10421, .T. ) ;
#38527 = ADVANCED_FACE ( 'NONE', ( #45403 ), #33564, .T. ) ;
#38528 = LINE ( 'NONE', #18557, #40538 ) ;
#38529 = EDGE_CURVE ( 'NONE', #51567, #30637, #29870, .T. ) ;
#38530 = VERTEX_POINT ( 'NONE', #30381 ) ;
#38531 = EDGE_CURVE ( 'NONE', #138, #26111, #14121, .T. ) ;
#38532 = DIRECTION ( 'NONE',  ( 0.7378332790417333475, 0.000000000000000000, -0.6749830015182038956 ) ) ;
#38533 = ORIENTED_EDGE ( 'NONE', *, *, #29837, .F. ) ;
#38534 = AXIS2_PLACEMENT_3D ( 'NONE', #16041, #49657, #9449 ) ;
#38535 = CYLINDRICAL_SURFACE ( 'NONE', #42719, 125.0000000000000000 ) ;
#38536 = CARTESIAN_POINT ( 'NONE',  ( -44.48323084606168720, -193.5000000000000000, 124.9361149384469769 ) ) ;
#38537 = ORIENTED_EDGE ( 'NONE', *, *, #48165, .F. ) ;
#38538 = CARTESIAN_POINT ( 'NONE',  ( -124.4642912599203584, -189.7472609257535510, 99.25348746834863789 ) ) ;
#38539 = VECTOR ( 'NONE', #22780, 1000.000000000000000 ) ;
#38540 = CARTESIAN_POINT ( 'NONE',  ( -339.1964088526558498, -157.4273119900853146, -48.27201571435997352 ) ) ;
#38541 = DIRECTION ( 'NONE',  ( 0.000000000000000000, -1.000000000000000000, 0.000000000000000000 ) ) ;
#38542 = ORIENTED_EDGE ( 'NONE', *, *, #3446, .T. ) ;
#38543 = ORIENTED_EDGE ( 'NONE', *, *, #245, .F. ) ;
#38544 = ORIENTED_EDGE ( 'NONE', *, *, #32751, .T. ) ;
#38545 = FACE_OUTER_BOUND ( 'NONE', #25956, .T. ) ;
#38546 = CARTESIAN_POINT ( 'NONE',  ( -50.89116676070551648, -183.6283474603465606, 124.9767260852757147 ) ) ;
#38547 = ADVANCED_FACE ( 'NONE', ( #30135 ), #42473, .T. ) ;
#38548 = CARTESIAN_POINT ( 'NONE',  ( -114.4014177456970458, -193.5000000000000000, 105.0256126866236457 ) ) ;
#38549 = CARTESIAN_POINT ( 'NONE',  ( -8.721998590732194856, -177.1207230881787780, -118.5089480183145270 ) ) ;
#38550 = CARTESIAN_POINT ( 'NONE',  ( -332.3517673607765914, -75.06648993880729392, -35.41461708323759439 ) ) ;
#38551 = ORIENTED_EDGE ( 'NONE', *, *, #24584, .F. ) ;
#38552 = EDGE_CURVE ( 'NONE', #43478, #12206, #40311, .T. ) ;
#38553 = EDGE_CURVE ( 'NONE', #19199, #30881, #5946, .T. ) ;
#38554 = VECTOR ( 'NONE', #31903, 1000.000000000000000 ) ;
#38555 = LINE ( 'NONE', #30926, #50076 ) ;
#38556 = EDGE_LOOP ( 'NONE', ( #15070, #17673, #21220, #6899 ) ) ;
#38558 = ORIENTED_EDGE ( 'NONE', *, *, #48747, .T. ) ;
#38557 = CARTESIAN_POINT ( 'NONE',  ( -330.4913330509368166, -84.75001853787810546, 44.49369547121489887 ) ) ;
#38559 = ORIENTED_EDGE ( 'NONE', *, *, #14771, .T. ) ;
#38560 = DIRECTION ( 'NONE',  ( 0.000000000000000000, 0.000000000000000000, 1.000000000000000000 ) ) ;
#38561 = ORIENTED_EDGE ( 'NONE', *, *, #42350, .T. ) ;
#38562 = DIRECTION ( 'NONE',  ( 0.000000000000000000, -0.9350162426854146114, 0.3546048870425363986 ) ) ;
#38563 = CARTESIAN_POINT ( 'NONE',  ( -336.3521761649654422, -64.50000000000000000, -2.632288850093980503 ) ) ;
#38564 = LINE ( 'NONE', #34607, #18385 ) ;
#38565 = EDGE_LOOP ( 'NONE', ( #33642, #16318, #28510, #4028 ) ) ;
#38566 = DIRECTION ( 'NONE',  ( -0.000000000000000000, 1.000000000000000000, -0.000000000000000000 ) ) ;
#38567 = EDGE_LOOP ( 'NONE', ( #46497, #8444, #261, #35375 ) ) ;
#38568 = ORIENTED_EDGE ( 'NONE', *, *, #45312, .F. ) ;
#38569 = CARTESIAN_POINT ( 'NONE',  ( -305.0000000000000568, -63.67752800890095699, 4.612141029301498385 ) ) ;
#38570 = LINE ( 'NONE', #41988, #30604 ) ;
#38571 = CIRCLE ( 'NONE', #13405, 125.0000000000000000 ) ;
#38572 = DIRECTION ( 'NONE',  ( -0.000000000000000000, 1.000000000000000000, -0.000000000000000000 ) ) ;
#38573 = VERTEX_POINT ( 'NONE', #21990 ) ;
#38574 = CARTESIAN_POINT ( 'NONE',  ( 69.25251857196690253, -189.7472609257535510, 38.92640747825683434 ) ) ;
#38575 = CIRCLE ( 'NONE', #18440, 125.0000000000000000 ) ;
#38576 = PLANE ( 'NONE',  #18063 ) ;
#38577 = CARTESIAN_POINT ( 'NONE',  ( 53.62339707355158680, -183.6283474603465606, -70.36529243996334060 ) ) ;
#38578 = FACE_OUTER_BOUND ( 'NONE', #17929, .T. ) ;
#38579 = ORIENTED_EDGE ( 'NONE', *, *, #12967, .T. ) ;
#38580 = CARTESIAN_POINT ( 'NONE',  ( 0.000000000000000000, -102.5783116644897888, 55.16595831843925879 ) ) ;
#38581 = LINE ( 'NONE', #33860, #22323 ) ;
#38582 = CARTESIAN_POINT ( 'NONE',  ( -339.1964088526558498, -123.9999999999993747, 59.99791663049644086 ) ) ;
#38583 = EDGE_LOOP ( 'NONE', ( #47563, #42190, #40589, #30924 ) ) ;
#38584 = CARTESIAN_POINT ( 'NONE',  ( 60.00000000000001421, -43.50000000000000000, 60.00000000000000711 ) ) ;
#38585 = FACE_BOUND ( 'NONE', #43516, .T. ) ;
#38586 = ORIENTED_EDGE ( 'NONE', *, *, #21026, .T. ) ;
#38587 = EDGE_CURVE ( 'NONE', #33386, #16397, #35260, .T. ) ;
#38588 = ADVANCED_FACE ( 'NONE', ( #1502 ), #37243, .T. ) ;
#38589 = FACE_OUTER_BOUND ( 'NONE', #10711, .T. ) ;
#38590 = VERTEX_POINT ( 'NONE', #42208 ) ;
#38591 = VECTOR ( 'NONE', #23029, 1000.000000000000000 ) ;
#38592 = PLANE ( 'NONE',  #31819 ) ;
#38593 = DIRECTION ( 'NONE',  ( 1.000000000000000000, -0.000000000000000000, -0.000000000000000000 ) ) ;
#38594 = CARTESIAN_POINT ( 'NONE',  ( 53.56330073376472001, -189.7472609257535510, 72.19655804062048787 ) ) ;
#38595 = DIRECTION ( 'NONE',  ( -0.000000000000000000, -1.000000000000000000, -0.000000000000000000 ) ) ;
#38596 = FACE_OUTER_BOUND ( 'NONE', #25694, .T. ) ;
#38597 = ORIENTED_EDGE ( 'NONE', *, *, #44786, .T. ) ;
#38598 = LINE ( 'NONE', #25998, #28143 ) ;
#38599 = ORIENTED_EDGE ( 'NONE', *, *, #11223, .F. ) ;
#38600 = CARTESIAN_POINT ( 'NONE',  ( -365.0000000000001137, -78.50000000000002842, 0.000000000000000000 ) ) ;
#38601 = AXIS2_PLACEMENT_3D ( 'NONE', #51279, #36015, #51799 ) ;
#38602 = ORIENTED_EDGE ( 'NONE', *, *, #48348, .T. ) ;
#38603 = EDGE_CURVE ( 'NONE', #24136, #41591, #22242, .T. ) ;
#38604 = LINE ( 'NONE', #38345, #29271 ) ;
#38605 = ADVANCED_FACE ( 'NONE', ( #5721 ), #29607, .T. ) ;
#38606 = PLANE ( 'NONE',  #27578 ) ;
#38607 = CARTESIAN_POINT ( 'NONE',  ( -48.47912675150885065, -177.1207230881787780, 6.938893903907228378E-15 ) ) ;
#38608 = ORIENTED_EDGE ( 'NONE', *, *, #3369, .F. ) ;
#38611 = ORIENTED_EDGE ( 'NONE', *, *, #30104, .F. ) ;
#38610 = CARTESIAN_POINT ( 'NONE',  ( -26.37732090265849294, -189.7472609257535510, -122.0143860769386919 ) ) ;
#38609 = CARTESIAN_POINT ( 'NONE',  ( -2.733443440668967384, 57.27004613166161562, -16.80698578740291538 ) ) ;
#38612 = PLANE ( 'NONE',  #23101 ) ;
#38613 = ORIENTED_EDGE ( 'NONE', *, *, #40633, .F. ) ;
#38614 = LINE ( 'NONE', #10494, #20525 ) ;
#38615 = ORIENTED_EDGE ( 'NONE', *, *, #42202, .T. ) ;
#38616 = CARTESIAN_POINT ( 'NONE',  ( -260.0000000000000000, -63.50000000000000000, -60.00000000000000711 ) ) ;
#38619 = ORIENTED_EDGE ( 'NONE', *, *, #43261, .F. ) ;
#38618 = LINE ( 'NONE', #30994, #40927 ) ;
#38617 = DIRECTION ( 'NONE',  ( 0.000000000000000000, 0.000000000000000000, -1.000000000000000000 ) ) ;
#38620 = EDGE_LOOP ( 'NONE', ( #6880, #7197, #25573, #35521 ) ) ;
#38621 = VECTOR ( 'NONE', #18516, 1000.000000000000000 ) ;
#38622 = AXIS2_PLACEMENT_3D ( 'NONE', #47121, #3235, #3730 ) ;
#38623 = PLANE ( 'NONE',  #43314 ) ;
#38624 = ORIENTED_EDGE ( 'NONE', *, *, #17702, .F. ) ;
#38625 = DIRECTION ( 'NONE',  ( 0.000000000000000000, 0.000000000000000000, 1.000000000000000000 ) ) ;
#38626 = CARTESIAN_POINT ( 'NONE',  ( -31.30262293407085039, -177.1207230881787780, -123.8142468240611294 ) ) ;
#38627 = VERTEX_POINT ( 'NONE', #50378 ) ;
#38628 = FACE_OUTER_BOUND ( 'NONE', #21635, .T. ) ;
#38629 = CARTESIAN_POINT ( 'NONE',  ( -336.3521761649654422, -65.24746378767824240, -9.724760635741734660 ) ) ;
#38630 = DIRECTION ( 'NONE',  ( 0.7765238627180482966, 0.000000000000000000, -0.6300878435817038881 ) ) ;
#38631 = FACE_OUTER_BOUND ( 'NONE', #24397, .T. ) ;
#38632 = DIRECTION ( 'NONE',  ( 0.000000000000000000, 1.000000000000000000, 0.000000000000000000 ) ) ;
#38633 = VERTEX_POINT ( 'NONE', #14366 ) ;
#38634 = DIRECTION ( 'NONE',  ( -0.000000000000000000, 1.000000000000000000, -0.000000000000000000 ) ) ;
#38635 = CARTESIAN_POINT ( 'NONE',  ( -33.86391487983341619, -175.3837268820161057, 124.1426420773540542 ) ) ;
#38636 = ADVANCED_FACE ( 'NONE', ( #1229, #49347 ), #10413, .F. ) ;
#38637 = CARTESIAN_POINT ( 'NONE',  ( -46.06708674231131084, -193.5000000000000000, -124.9767260852756863 ) ) ;
#38638 = VERTEX_POINT ( 'NONE', #33813 ) ;
#38639 = AXIS2_PLACEMENT_3D ( 'NONE', #3370, #51471, #34900 ) ;
#38640 = PLANE ( 'NONE',  #47474 ) ;
#38641 = PLANE ( 'NONE',  #25273 ) ;
#38642 = LINE ( 'NONE', #34699, #8457 ) ;
#38643 = CARTESIAN_POINT ( 'NONE',  ( -330.4913330509368166, -66.33409060400650503, 14.60509510167813474 ) ) ;
#38644 = EDGE_CURVE ( 'NONE', #36738, #35874, #49856, .T. ) ;
#38645 = VERTEX_POINT ( 'NONE', #10938 ) ;
#38646 = ADVANCED_FACE ( 'NONE', ( #27482 ), #35618, .F. ) ;
#38647 = CYLINDRICAL_SURFACE ( 'NONE', #49665, 125.0000000000000000 ) ;
#38648 = DIRECTION ( 'NONE',  ( 0.000000000000000000, 1.385465816146810017E-13, 1.000000000000000000 ) ) ;
#38649 = CARTESIAN_POINT ( 'NONE',  ( -330.4913330509368166, -95.17484985463094915, 52.89315522108979906 ) ) ;
#38650 = EDGE_CURVE ( 'NONE', #44477, #7058, #35359, .T. ) ;
#38651 = ORIENTED_EDGE ( 'NONE', *, *, #51660, .F. ) ;
#38652 = CARTESIAN_POINT ( 'NONE',  ( -153.4237445717492392, -175.3837268820161057, 66.05018866041349668 ) ) ;
#38653 = CIRCLE ( 'NONE', #7599, 10.99999999999999645 ) ;
#38654 = VECTOR ( 'NONE', #7112, 1000.000000000000000 ) ;
#38655 = CARTESIAN_POINT ( 'NONE',  ( -47.87232660569025455, -193.5000000000000000, -0.7948544414133454916 ) ) ;
#38656 = ORIENTED_EDGE ( 'NONE', *, *, #28920, .T. ) ;
#38657 = EDGE_LOOP ( 'NONE', ( #10429, #40912, #7998, #5571 ) ) ;
#38658 = ORIENTED_EDGE ( 'NONE', *, *, #26972, .T. ) ;
#38659 = EDGE_CURVE ( 'NONE', #36957, #16290, #51671, .T. ) ;
#38660 = CARTESIAN_POINT ( 'NONE',  ( -23.25236516653336594, -183.6283474603465606, -121.4073237908566654 ) ) ;
#38661 = DIRECTION ( 'NONE',  ( -0.000000000000000000, 1.000000000000000000, -0.000000000000000000 ) ) ;
#38662 = CARTESIAN_POINT ( 'NONE',  ( 141.7825277784304205, -213.5000000000000000, -41.45482488023466061 ) ) ;
#38663 = ORIENTED_EDGE ( 'NONE', *, *, #6087, .T. ) ;
#38664 = LINE ( 'NONE', #34221, #5014 ) ;
#38665 = CARTESIAN_POINT ( 'NONE',  ( -180.0000000000000568, -123.5000000000000284, -15.24495751795538290 ) ) ;
#38668 = VERTEX_POINT ( 'NONE', #11189 ) ;
#38667 = DIRECTION ( 'NONE',  ( -0.000000000000000000, 1.000000000000000000, -0.000000000000000000 ) ) ;
#38666 = CARTESIAN_POINT ( 'NONE',  ( 76.01188277843577623, -189.7472609257535510, 11.26891947860283061 ) ) ;
#38669 = VECTOR ( 'NONE', #48765, 1000.000000000000000 ) ;
#38670 = EDGE_CURVE ( 'NONE', #22921, #19768, #34579, .T. ) ;
#38671 = PLANE ( 'NONE',  #44028 ) ;
#38672 = EDGE_LOOP ( 'NONE', ( #4063, #4751, #51921, #32948 ) ) ;
#38673 = CARTESIAN_POINT ( 'NONE',  ( -330.4913330509368166, -176.8578783931336602, 27.43969411971572470 ) ) ;
#38674 = ORIENTED_EDGE ( 'NONE', *, *, #843, .T. ) ;
#38675 = CARTESIAN_POINT ( 'NONE',  ( -336.3521761649654422, -64.61288906875131488, 4.498567634385603142 ) ) ;
#38676 = DIRECTION ( 'NONE',  ( 0.000000000000000000, 0.000000000000000000, 1.000000000000000000 ) ) ;
#38677 = PLANE ( 'NONE',  #45887 ) ;
#38678 = ORIENTED_EDGE ( 'NONE', *, *, #11182, .F. ) ;
#38679 = ORIENTED_EDGE ( 'NONE', *, *, #29092, .T. ) ;
#38680 = DIRECTION ( 'NONE',  ( 0.8757349421956379665, 0.000000000000000000, -0.4827922027307427477 ) ) ;
#38681 = CARTESIAN_POINT ( 'NONE',  ( -48.47912675150885065, -189.7472609257535510, 6.938893903907228378E-15 ) ) ;
#38682 = ORIENTED_EDGE ( 'NONE', *, *, #1875, .T. ) ;
#38683 = DIRECTION ( 'NONE',  ( -0.000000000000000000, 1.000000000000000000, 0.000000000000000000 ) ) ;
#38684 = VECTOR ( 'NONE', #7379, 1000.000000000000227 ) ;
#38685 = DIRECTION ( 'NONE',  ( -0.000000000000000000, 1.000000000000000000, -0.000000000000000000 ) ) ;
#38686 = EDGE_CURVE ( 'NONE', #14634, #23542, #15671, .T. ) ;
#38687 = ORIENTED_EDGE ( 'NONE', *, *, #35291, .T. ) ;
#38688 = FACE_BOUND ( 'NONE', #50465, .T. ) ;
#38689 = CARTESIAN_POINT ( 'NONE',  ( -159.0901268547125653, -183.6283474603465606, 58.22548115875958530 ) ) ;
#38690 = AXIS2_PLACEMENT_3D ( 'NONE', #51991, #41168, #12270 ) ;
#38691 = EDGE_CURVE ( 'NONE', #45141, #26421, #14902, .T. ) ;
#38692 = ORIENTED_EDGE ( 'NONE', *, *, #18836, .T. ) ;
#38693 = DIRECTION ( 'NONE',  ( -0.000000000000000000, -1.346129392433909288E-16, 1.000000000000000000 ) ) ;
#38694 = ORIENTED_EDGE ( 'NONE', *, *, #25022, .F. ) ;
#38695 = CARTESIAN_POINT ( 'NONE',  ( 71.97629403264902237, -177.1207230881787780, -29.43839964798648623 ) ) ;
#38696 = DIRECTION ( 'NONE',  ( 0.000000000000000000, 0.000000000000000000, 1.000000000000000000 ) ) ;
#38697 = ORIENTED_EDGE ( 'NONE', *, *, #7675, .T. ) ;
#38698 = LINE ( 'NONE', #2704, #47042 ) ;
#38699 = CARTESIAN_POINT ( 'NONE',  ( -305.0000000000000568, -168.7406467949202806, 39.41172259083927543 ) ) ;
#38700 = DIRECTION ( 'NONE',  ( -1.000000000000000000, -0.000000000000000000, -0.000000000000000000 ) ) ;
#38701 = EDGE_CURVE ( 'NONE', #38482, #30451, #19597, .T. ) ;
#38702 = EDGE_CURVE ( 'NONE', #15571, #45713, #19094, .T. ) ;
#38703 = EDGE_CURVE ( 'NONE', #34512, #47944, #6748, .T. ) ;
#38704 = EDGE_LOOP ( 'NONE', ( #41056, #16792, #31152, #30779 ) ) ;
#38705 = DIRECTION ( 'NONE',  ( 0.6965510290629882695, 0.000000000000000000, 0.7175072570443395970 ) ) ;
#38706 = EDGE_CURVE ( 'NONE', #31601, #42139, #39311, .T. ) ;
#38707 = CIRCLE ( 'NONE', #11020, 125.0000000000000000 ) ;
#38708 = LINE ( 'NONE', #42664, #42074 ) ;
#38709 = CARTESIAN_POINT ( 'NONE',  ( -48.47912675150885065, -183.6283474603465606, 6.938893903907228378E-15 ) ) ;
#38711 = VERTEX_POINT ( 'NONE', #26959 ) ;
#38710 = CARTESIAN_POINT ( 'NONE',  ( -48.47912675150885065, -189.7472609257535510, 6.938893903907228378E-15 ) ) ;
#38712 = EDGE_LOOP ( 'NONE', ( #50195, #51116, #26698, #41913 ) ) ;
#38713 = CARTESIAN_POINT ( 'NONE',  ( -336.3521761649654422, -68.91285928486892942, -22.44790492310182017 ) ) ;
#38714 = DIRECTION ( 'NONE',  ( 0.000000000000000000, 0.000000000000000000, -1.000000000000000000 ) ) ;
#38715 = ORIENTED_EDGE ( 'NONE', *, *, #44227, .T. ) ;
#38716 = DIRECTION ( 'NONE',  ( -1.000000000000000000, -0.000000000000000000, 0.000000000000000000 ) ) ;
#38717 = VERTEX_POINT ( 'NONE', #19347 ) ;
#38718 = DIRECTION ( 'NONE',  ( -0.000000000000000000, 0.8854560256532157947, 0.4647231720437573488 ) ) ;
#38719 = DIRECTION ( 'NONE',  ( -0.000000000000000000, 1.000000000000000000, -0.000000000000000000 ) ) ;
#38720 = CYLINDRICAL_SURFACE ( 'NONE', #19430, 125.0000000000000000 ) ;
#38721 = DIRECTION ( 'NONE',  ( -0.000000000000000000, -0.9927088740980530845, 0.1205366802553303057 ) ) ;
#38722 = VECTOR ( 'NONE', #43552, 1000.000000000000227 ) ;
#38723 = VERTEX_POINT ( 'NONE', #27733 ) ;
#38724 = ORIENTED_EDGE ( 'NONE', *, *, #45313, .F. ) ;
#38726 = ORIENTED_EDGE ( 'NONE', *, *, #20996, .T. ) ;
#38725 = CIRCLE ( 'NONE', #16089, 125.0000000000000000 ) ;
#38727 = CARTESIAN_POINT ( 'NONE',  ( -238.7407812814481076, -213.5000000000000000, -9.999999999999987566 ) ) ;
#38728 = CARTESIAN_POINT ( 'NONE',  ( -122.3978016498073345, -183.6283474603465606, -100.8019320314827070 ) ) ;
#38729 = LINE ( 'NONE', #47160, #27034 ) ;
#38730 = DIRECTION ( 'NONE',  ( 0.000000000000000000, -1.000000000000000000, 0.000000000000000000 ) ) ;
#38731 = ORIENTED_EDGE ( 'NONE', *, *, #38644, .F. ) ;
#38732 = DIRECTION ( 'NONE',  ( 0.000000000000000000, -1.000000000000000000, -0.000000000000000000 ) ) ;
#38733 = AXIS2_PLACEMENT_3D ( 'NONE', #17848, #41225, #17082 ) ;
#38734 = ORIENTED_EDGE ( 'NONE', *, *, #27907, .F. ) ;
#38735 = ORIENTED_EDGE ( 'NONE', *, *, #633, .T. ) ;
#38736 = PLANE ( 'NONE',  #22307 ) ;
#38737 = AXIS2_PLACEMENT_3D ( 'NONE', #22903, #38138, #2146 ) ;
#38738 = CARTESIAN_POINT ( 'NONE',  ( -26.20043062753592977, -175.3837268820161057, -122.9986166548863196 ) ) ;
#38739 = CARTESIAN_POINT ( 'NONE',  ( -48.47912675150885065, -189.7472609257535510, 6.938893903907228378E-15 ) ) ;
#38740 = PLANE ( 'NONE',  #3182 ) ;
#38741 = EDGE_CURVE ( 'NONE', #4396, #13063, #2538, .T. ) ;
#38742 = LINE ( 'NONE', #50860, #12777 ) ;
#38743 = ADVANCED_FACE ( 'NONE', ( #10682 ), #7522, .F. ) ;
#38744 = ADVANCED_FACE ( 'NONE', ( #22771 ), #40343, .T. ) ;
#38745 = CARTESIAN_POINT ( 'NONE',  ( 15.80042947435468470, -189.7472609257535510, 107.2060569716377927 ) ) ;
#38746 = VERTEX_POINT ( 'NONE', #18817 ) ;
#38747 = LINE ( 'NONE', #27178, #25082 ) ;
#38748 = ORIENTED_EDGE ( 'NONE', *, *, #40051, .T. ) ;
#38749 = DIRECTION ( 'NONE',  ( 0.000000000000000000, -0.000000000000000000, 1.000000000000000000 ) ) ;
#38750 = DIRECTION ( 'NONE',  ( 0.000000000000000000, -1.000000000000000000, 0.000000000000000000 ) ) ;
#38751 = ORIENTED_EDGE ( 'NONE', *, *, #26166, .F. ) ;
#38752 = EDGE_CURVE ( 'NONE', #17498, #33612, #31419, .T. ) ;
#38753 = VECTOR ( 'NONE', #46276, 1000.000000000000000 ) ;
#38754 = PLANE ( 'NONE',  #29009 ) ;
#38755 = CARTESIAN_POINT ( 'NONE',  ( -48.47912675150885065, -183.6283474603465606, 6.938893903907228378E-15 ) ) ;
#38756 = CYLINDRICAL_SURFACE ( 'NONE', #3866, 125.0000000000000000 ) ;
#38757 = EDGE_CURVE ( 'NONE', #14148, #3147, #50898, .T. ) ;
#38758 = CARTESIAN_POINT ( 'NONE',  ( -108.4791267515088435, -132.5479369270331915, -186.7953921478704729 ) ) ;
#38759 = EDGE_CURVE ( 'NONE', #3318, #43850, #42994, .T. ) ;
#38760 = AXIS2_PLACEMENT_3D ( 'NONE', #49913, #38593, #6283 ) ;
#38761 = CARTESIAN_POINT ( 'NONE',  ( 71.15591247552653442, -183.6283474603465606, 36.22785377504035154 ) ) ;
#38762 = VERTEX_POINT ( 'NONE', #23022 ) ;
#38763 = ADVANCED_FACE ( 'NONE', ( #51169 ), #3564, .T. ) ;
#38764 = CARTESIAN_POINT ( 'NONE',  ( -48.59739992243022755, -183.6283474603465606, 0.9929810960135230236 ) ) ;
#38766 = EDGE_LOOP ( 'NONE', ( #47842, #27433, #17507, #6501 ) ) ;
#38765 = DIRECTION ( 'NONE',  ( 0.000000000000000000, 1.000000000000000000, 0.000000000000000000 ) ) ;
#38767 = EDGE_CURVE ( 'NONE', #27923, #32981, #36161, .T. ) ;
#38768 = ORIENTED_EDGE ( 'NONE', *, *, #45193, .T. ) ;
#38769 = CARTESIAN_POINT ( 'NONE',  ( -172.2424017797220870, -193.5000000000000000, 7.666780576875859232 ) ) ;
#38770 = EDGE_LOOP ( 'NONE', ( #20386, #42885, #11913, #6795 ) ) ;
#38771 = VECTOR ( 'NONE', #26109, 999.9999999999998863 ) ;
#38772 = CARTESIAN_POINT ( 'NONE',  ( -172.9089226952081617, -193.5000000000000000, 11.92584929509620117 ) ) ;
#38773 = AXIS2_PLACEMENT_3D ( 'NONE', #12586, #40961, #5245 ) ;
#38774 = CIRCLE ( 'NONE', #37966, 125.0000000000000000 ) ;
#38775 = VERTEX_POINT ( 'NONE', #36140 ) ;
#38776 = FACE_BOUND ( 'NONE', #45232, .T. ) ;
#38777 = DIRECTION ( 'NONE',  ( -0.4677363560876381388, 0.000000000000000000, -0.8838680338115288970 ) ) ;
#38778 = VERTEX_POINT ( 'NONE', #24320 ) ;
#38779 = LINE ( 'NONE', #2784, #19904 ) ;
#38780 = CARTESIAN_POINT ( 'NONE',  ( 46.00000000000000711, -43.50000000000000000, -46.00000000000000000 ) ) ;
#38781 = CARTESIAN_POINT ( 'NONE',  ( -172.1341525481709880, -189.7472609257535510, 18.28755301364335750 ) ) ;
#38782 = EDGE_CURVE ( 'NONE', #14631, #34611, #8295, .T. ) ;
#38783 = ORIENTED_EDGE ( 'NONE', *, *, #22816, .F. ) ;
#38784 = ORIENTED_EDGE ( 'NONE', *, *, #23099, .F. ) ;
#38785 = EDGE_LOOP ( 'NONE', ( #38542, #26440, #17732, #36358 ) ) ;
#38786 = DIRECTION ( 'NONE',  ( 0.000000000000000000, -0.000000000000000000, -1.000000000000000000 ) ) ;
#38787 = LINE ( 'NONE', #10420, #51180 ) ;
#38788 = LINE ( 'NONE', #38548, #37718 ) ;
#38789 = CARTESIAN_POINT ( 'NONE',  ( -48.47912675150885065, -189.7472609257535510, 6.938893903907228378E-15 ) ) ;
#38790 = PLANE ( 'NONE',  #1181 ) ;
#38791 = VECTOR ( 'NONE', #9950, 1000.000000000000000 ) ;
#38792 = VERTEX_POINT ( 'NONE', #47978 ) ;
#38793 = AXIS2_PLACEMENT_3D ( 'NONE', #19216, #27603, #17091 ) ;
#38794 = CARTESIAN_POINT ( 'NONE',  ( -339.1964088526558498, -123.5000000000000284, -60.00000000000000000 ) ) ;
#38795 = EDGE_CURVE ( 'NONE', #4839, #24818, #39807, .T. ) ;
#38796 = ORIENTED_EDGE ( 'NONE', *, *, #42271, .F. ) ;
#38798 = ORIENTED_EDGE ( 'NONE', *, *, #35262, .T. ) ;
#38797 = CARTESIAN_POINT ( 'NONE',  ( -84.82349129030166068, -193.5000000000000000, -119.5996955107802222 ) ) ;
#38799 = VERTEX_POINT ( 'NONE', #669 ) ;
#38800 = CARTESIAN_POINT ( 'NONE',  ( -332.3517673607765914, -159.7173995167596274, -47.83617848703448772 ) ) ;
#38801 = CARTESIAN_POINT ( 'NONE',  ( -94.78385179329471555, -177.1207230881787780, 115.0304316645283080 ) ) ;
#38802 = EDGE_CURVE ( 'NONE', #46508, #29853, #44812, .T. ) ;
#38803 = EDGE_CURVE ( 'NONE', #50020, #42079, #4345, .T. ) ;
#38804 = DIRECTION ( 'NONE',  ( -0.000000000000000000, 1.000000000000000000, -0.000000000000000000 ) ) ;
#38805 = EDGE_CURVE ( 'NONE', #42455, #31317, #12996, .T. ) ;
#38806 = EDGE_CURVE ( 'NONE', #21836, #40165, #51293, .T. ) ;
#38807 = CARTESIAN_POINT ( 'NONE',  ( 20.65191334053708161, -193.5000000000000000, 102.9412430821799802 ) ) ;
#38808 = VERTEX_POINT ( 'NONE', #40325 ) ;
#38809 = DIRECTION ( 'NONE',  ( 0.000000000000000000, 0.3546048870425331234, -0.9350162426854158326 ) ) ;
#38810 = ORIENTED_EDGE ( 'NONE', *, *, #41764, .F. ) ;
#38811 = VECTOR ( 'NONE', #19560, 1000.000000000000000 ) ;
#38812 = EDGE_CURVE ( 'NONE', #42898, #3693, #12488, .T. ) ;
#38813 = ORIENTED_EDGE ( 'NONE', *, *, #39112, .T. ) ;
#38814 = DIRECTION ( 'NONE',  ( -0.000000000000000000, 1.000000000000000000, -0.000000000000000000 ) ) ;
#38815 = VECTOR ( 'NONE', #27520, 1000.000000000000114 ) ;
#38817 = AXIS2_PLACEMENT_3D ( 'NONE', #16659, #44759, #39750 ) ;
#38816 = CARTESIAN_POINT ( 'NONE',  ( -339.1964088526558498, -109.8658467157464571, 57.40522506028071348 ) ) ;
#38818 = EDGE_CURVE ( 'NONE', #23565, #50532, #136, .T. ) ;
#38819 = DIRECTION ( 'NONE',  ( 0.000000000000000000, -1.000000000000000000, 0.000000000000000000 ) ) ;
#38820 = DIRECTION ( 'NONE',  ( 0.000000000000000000, 0.000000000000000000, 1.000000000000000000 ) ) ;
#38821 = EDGE_LOOP ( 'NONE', ( #35583, #11400, #46720, #20106 ) ) ;
#38822 = FACE_OUTER_BOUND ( 'NONE', #31966, .T. ) ;
#38823 = DIRECTION ( 'NONE',  ( -8.718379230999705894E-17, 0.9350162426854132791, -0.3546048870425396182 ) ) ;
#38824 = CARTESIAN_POINT ( 'NONE',  ( -21.46839590530488451, -193.5000000000000000, 122.0467960216650738 ) ) ;
#38825 = CARTESIAN_POINT ( 'NONE',  ( -149.9407190013151592, -189.7472609257535510, -73.01058346660460074 ) ) ;
#38826 = VECTOR ( 'NONE', #47520, 1000.000000000000000 ) ;
#38827 = EDGE_CURVE ( 'NONE', #10779, #18318, #8797, .T. ) ;
#38828 = VERTEX_POINT ( 'NONE', #15931 ) ;
#38829 = CARTESIAN_POINT ( 'NONE',  ( -65.65563056894596627, -193.5000000000000000, 123.8142468240612999 ) ) ;
#38830 = DIRECTION ( 'NONE',  ( -0.000000000000000000, 1.000000000000000000, -0.000000000000000000 ) ) ;
#38831 = EDGE_CURVE ( 'NONE', #21117, #664, #19857, .T. ) ;
#38832 = LINE ( 'NONE', #15456, #39144 ) ;
#38833 = ORIENTED_EDGE ( 'NONE', *, *, #17776, .F. ) ;
#38834 = EDGE_CURVE ( 'NONE', #35535, #15154, #24835, .T. ) ;
#38835 = LINE ( 'NONE', #39599, #4595 ) ;
#38836 = VECTOR ( 'NONE', #28019, 1000.000000000000114 ) ;
#38837 = CARTESIAN_POINT ( 'NONE',  ( -332.3517673607765914, -123.5000000000000284, 0.000000000000000000 ) ) ;
#38838 = EDGE_CURVE ( 'NONE', #16966, #17396, #42055, .T. ) ;
#38839 = VERTEX_POINT ( 'NONE', #32198 ) ;
#38840 = CARTESIAN_POINT ( 'NONE',  ( 40.71578595748727736, -177.1207230881787780, 86.14171647324927505 ) ) ;
#38841 = ORIENTED_EDGE ( 'NONE', *, *, #14442, .T. ) ;
#38842 = ADVANCED_FACE ( 'NONE', ( #40084 ), #4882, .T. ) ;
#38843 = CIRCLE ( 'NONE', #7782, 125.0000000000000000 ) ;
#38844 = CARTESIAN_POINT ( 'NONE',  ( -330.4913330509368166, -123.5000000000000284, 0.000000000000000000 ) ) ;
#38845 = FACE_BOUND ( 'NONE', #39315, .T. ) ;
#38846 = DIRECTION ( 'NONE',  ( 0.05924062789371441901, 0.000000000000000000, -0.9982437317643214625 ) ) ;
#38848 = AXIS2_PLACEMENT_3D ( 'NONE', #20747, #36776, #20472 ) ;
#38847 = DIRECTION ( 'NONE',  ( -0.000000000000000000, -0.8229838658936516893, 0.5680647467311626952 ) ) ;
#38849 = VECTOR ( 'NONE', #29866, 1000.000000000000227 ) ;
#38850 = ADVANCED_FACE ( 'NONE', ( #917 ), #44551, .F. ) ;
#38851 = ORIENTED_EDGE ( 'NONE', *, *, #47245, .T. ) ;
#38852 = ADVANCED_FACE ( 'NONE', ( #20113 ), #48242, .T. ) ;
#38853 = EDGE_LOOP ( 'NONE', ( #36607, #46494, #44116, #38877 ) ) ;
#38854 = DIRECTION ( 'NONE',  ( 0.000000000000000000, 0.000000000000000000, 1.000000000000000000 ) ) ;
#38855 = VECTOR ( 'NONE', #10281, 1000.000000000000000 ) ;
#38856 = VERTEX_POINT ( 'NONE', #7770 ) ;
#38857 = DIRECTION ( 'NONE',  ( -1.000000000000000000, -0.000000000000000000, 0.000000000000000000 ) ) ;
#38858 = AXIS2_PLACEMENT_3D ( 'NONE', #25159, #4932, #21209 ) ;
#38859 = PLANE ( 'NONE',  #14176 ) ;
#38860 = DIRECTION ( 'NONE',  ( 0.000000000000000000, 0.000000000000000000, -1.000000000000000000 ) ) ;
#38861 = EDGE_LOOP ( 'NONE', ( #30205, #977, #23175, #16927 ) ) ;
#38864 = ORIENTED_EDGE ( 'NONE', *, *, #38529, .F. ) ;
#38863 = FILL_AREA_STYLE_COLOUR ( '', #39841 ) ;
#38862 = DIRECTION ( 'NONE',  ( 0.000000000000000000, -0.000000000000000000, 1.000000000000000000 ) ) ;
#38865 = DIRECTION ( 'NONE',  ( 0.6068001458185945385, 0.000000000000000000, -0.7948544414133523750 ) ) ;
#38866 = VERTEX_POINT ( 'NONE', #45605 ) ;
#38867 = LINE ( 'NONE', #6579, #42401 ) ;
#38868 = VECTOR ( 'NONE', #19195, 999.9999999999998863 ) ;
#38869 = ORIENTED_EDGE ( 'NONE', *, *, #10172, .F. ) ;
#38870 = EDGE_CURVE ( 'NONE', #3626, #809, #45090, .T. ) ;
#38871 = EDGE_CURVE ( 'NONE', #46522, #1772, #41902, .T. ) ;
#38872 = LINE ( 'NONE', #47035, #32589 ) ;
#38873 = VERTEX_POINT ( 'NONE', #21153 ) ;
#38876 = ORIENTED_EDGE ( 'NONE', *, *, #3598, .F. ) ;
#38875 = LINE ( 'NONE', #27303, #2347 ) ;
#38874 = CARTESIAN_POINT ( 'NONE',  ( -171.5592422664403216, -177.1207230881787780, -21.82395850507255375 ) ) ;
#38877 = ORIENTED_EDGE ( 'NONE', *, *, #48303, .F. ) ;
#38878 = VECTOR ( 'NONE', #31347, 1000.000000000000114 ) ;
#38879 = EDGE_CURVE ( 'NONE', #44102, #48867, #42875, .T. ) ;
#38880 = CARTESIAN_POINT ( 'NONE',  ( -336.3521761649654422, -154.8494888031386836, 50.05135858667791382 ) ) ;
#38881 = VERTEX_POINT ( 'NONE', #33756 ) ;
#38882 = LINE ( 'NONE', #34679, #1854 ) ;
#38883 = CARTESIAN_POINT ( 'NONE',  ( 32.99469856375238663, -175.3837268820161057, 94.79987230212020677 ) ) ;
#38884 = ORIENTED_EDGE ( 'NONE', *, *, #14054, .F. ) ;
#38885 = CARTESIAN_POINT ( 'NONE',  ( -238.7407812814481076, -193.5000000000000000, -9.999999999999987566 ) ) ;
#38886 = CARTESIAN_POINT ( 'NONE',  ( 0.000000000000000000, -175.7419055135395922, -27.41866715058203852 ) ) ;
#38887 = DIRECTION ( 'NONE',  ( 0.000000000000000000, 1.000000000000000000, 0.000000000000000000 ) ) ;
#38888 = FACE_OUTER_BOUND ( 'NONE', #37762, .T. ) ;
#38889 = ORIENTED_EDGE ( 'NONE', *, *, #30815, .F. ) ;
#38890 = AXIS2_PLACEMENT_3D ( 'NONE', #25547, #30016, #41570 ) ;
#38891 = FACE_OUTER_BOUND ( 'NONE', #14329, .T. ) ;
#38892 = DIRECTION ( 'NONE',  ( 0.8124868780056825335, 0.000000000000000000, -0.5829794791144703447 ) ) ;
#38893 = CARTESIAN_POINT ( 'NONE',  ( 20.66186849114819069, -193.5000000000000000, -104.1370384486465070 ) ) ;
#38894 = EDGE_LOOP ( 'NONE', ( #17793, #29365, #38455, #816 ) ) ;
#38895 = VECTOR ( 'NONE', #41402, 1000.000000000000114 ) ;
#38896 = DIRECTION ( 'NONE',  ( 0.000000000000000000, 0.000000000000000000, -1.000000000000000000 ) ) ;
#38897 = EDGE_CURVE ( 'NONE', #26043, #18024, #17998, .T. ) ;
#38898 = DIRECTION ( 'NONE',  ( 0.000000000000000000, 1.000000000000000000, 0.000000000000000000 ) ) ;
#38899 = CARTESIAN_POINT ( 'NONE',  ( -336.3521761649653854, -77.52356969168074841, 38.55084767037245541 ) ) ;
#38900 = LINE ( 'NONE', #3171, #28288 ) ;
#38901 = ORIENTED_EDGE ( 'NONE', *, *, #28532, .F. ) ;
#38902 = ADVANCED_FACE ( 'NONE', ( #45348 ), #1170, .F. ) ;
#38903 = DIRECTION ( 'NONE',  ( -1.000000000000000000, 0.000000000000000000, 0.000000000000000000 ) ) ;
#38904 = DIRECTION ( 'NONE',  ( 0.000000000000000000, 0.000000000000000000, -1.000000000000000000 ) ) ;
#38905 = DIRECTION ( 'NONE',  ( 1.000000000000000000, -5.781354811211920680E-17, -6.525800561034928863E-17 ) ) ;
#38906 = CARTESIAN_POINT ( 'NONE',  ( -48.07600332222087758, -189.7472609257535510, -0.9151456172430111335 ) ) ;
#38907 = DIRECTION ( 'NONE',  ( 0.000000000000000000, 0.5680647467311569221, 0.8229838658936556861 ) ) ;
#38908 = AXIS2_PLACEMENT_3D ( 'NONE', #5773, #41997, #29916 ) ;
#38909 = EDGE_LOOP ( 'NONE', ( #47131, #28472, #2979, #25679 ) ) ;
#38910 = FACE_OUTER_BOUND ( 'NONE', #27529, .T. ) ;
#38911 = VECTOR ( 'NONE', #50507, 999.9999999999998863 ) ;
#38912 = DIRECTION ( 'NONE',  ( 0.000000000000000000, -1.000000000000000000, -0.000000000000000000 ) ) ;
#38913 = VERTEX_POINT ( 'NONE', #22191 ) ;
#38914 = ORIENTED_EDGE ( 'NONE', *, *, #21395, .F. ) ;
#38915 = ORIENTED_EDGE ( 'NONE', *, *, #15429, .F. ) ;
#38916 = FACE_OUTER_BOUND ( 'NONE', #41485, .T. ) ;
#38917 = CARTESIAN_POINT ( 'NONE',  ( -107.6930423737362190, -183.6283474603465606, 110.0850225811110761 ) ) ;
#38919 = ORIENTED_EDGE ( 'NONE', *, *, #28771, .T. ) ;
#38918 = CIRCLE ( 'NONE', #37244, 60.00000000000000000 ) ;
#38920 = CARTESIAN_POINT ( 'NONE',  ( 24.15597040328004752, -193.5000000000000000, -101.7307360698543874 ) ) ;
#38921 = CARTESIAN_POINT ( 'NONE',  ( -48.47912675150885065, -177.1207230881787780, 6.938893903907228378E-15 ) ) ;
#38924 = VERTEX_POINT ( 'NONE', #13276 ) ;
#38923 = DIRECTION ( 'NONE',  ( -0.2348860457809707758, 0.000000000000000000, -0.9720229140804138579 ) ) ;
#38922 = CARTESIAN_POINT ( 'NONE',  ( -43.48323084606168720, -177.1207230881787780, 124.9001241957026167 ) ) ;
#38925 = CARTESIAN_POINT ( 'NONE',  ( -26.71218532227686637, -175.3837268820161057, 122.0745693923550732 ) ) ;
#38926 = ORIENTED_EDGE ( 'NONE', *, *, #24791, .T. ) ;
#38927 = DIRECTION ( 'NONE',  ( 0.000000000000000000, 0.000000000000000000, -1.000000000000000000 ) ) ;
#38928 = EDGE_LOOP ( 'NONE', ( #3711, #34599, #14111, #49396 ) ) ;
#38929 = EDGE_CURVE ( 'NONE', #20567, #33538, #41183, .T. ) ;
#38930 = CARTESIAN_POINT ( 'NONE',  ( -180.0000000000000568, -123.5000000000000284, 37.63467731922665394 ) ) ;
#38931 = DIRECTION ( 'NONE',  ( 0.000000000000000000, 0.000000000000000000, -1.000000000000000000 ) ) ;
#38932 = CARTESIAN_POINT ( 'NONE',  ( -156.9880281022168163, -189.7472609257535510, -60.01515274640939879 ) ) ;
#38933 = EDGE_LOOP ( 'NONE', ( #24907, #26220, #29628, #42226 ) ) ;
#38934 = VERTEX_POINT ( 'NONE', #29297 ) ;
#38935 = DIRECTION ( 'NONE',  ( -0.000000000000000000, 1.000000000000000000, -0.000000000000000000 ) ) ;
#38936 = CARTESIAN_POINT ( 'NONE',  ( -336.3521761649654422, -127.9985676343858501, 58.88711093124869222 ) ) ;
#38937 = EDGE_LOOP ( 'NONE', ( #25287, #22240, #30465, #32852 ) ) ;
#38938 = DIRECTION ( 'NONE',  ( -0.000000000000000000, 1.000000000000000000, -1.541976423090494894E-16 ) ) ;
#38939 = AXIS2_PLACEMENT_3D ( 'NONE', #4291, #28705, #40275 ) ;
#38940 = PLANE ( 'NONE',  #2190 ) ;
#38941 = VECTOR ( 'NONE', #12582, 1000.000000000000000 ) ;
#38942 = ORIENTED_EDGE ( 'NONE', *, *, #35247, .T. ) ;
#38943 = FACE_BOUND ( 'NONE', #7491, .T. ) ;
#38945 = AXIS2_PLACEMENT_3D ( 'NONE', #23273, #35088, #26415 ) ;
#38944 = CARTESIAN_POINT ( 'NONE',  ( 50.70030191143631271, -193.5000000000000000, -76.08180419845318454 ) ) ;
#38946 = ORIENTED_EDGE ( 'NONE', *, *, #39617, .T. ) ;
#38947 = DIRECTION ( 'NONE',  ( 0.8124868780056742068, 0.000000000000000000, 0.5829794791144820021 ) ) ;
#38948 = VERTEX_POINT ( 'NONE', #45857 ) ;
#38949 = CYLINDRICAL_SURFACE ( 'NONE', #39865, 125.0000000000000000 ) ;
#38950 = DIRECTION ( 'NONE',  ( 0.000000000000000000, 0.000000000000000000, -1.000000000000000000 ) ) ;
#38951 = EDGE_CURVE ( 'NONE', #4337, #34100, #5664, .T. ) ;
#38952 = ORIENTED_EDGE ( 'NONE', *, *, #36956, .F. ) ;
#38953 = CARTESIAN_POINT ( 'NONE',  ( -339.1964088526558498, -79.00630452878473875, -38.74998146212148953 ) ) ;
#38954 = PLANE ( 'NONE',  #9627 ) ;
#38955 = CARTESIAN_POINT ( 'NONE',  ( -60.00000000000000000, 20.00000000000000000, -60.00000000000000711 ) ) ;
#38956 = VECTOR ( 'NONE', #35631, 1000.000000000000000 ) ;
#38957 = ORIENTED_EDGE ( 'NONE', *, *, #19130, .F. ) ;
#38958 = CARTESIAN_POINT ( 'NONE',  ( 76.31829002442924548, -183.6283474603465606, 7.113702696402428138 ) ) ;
#38959 = ADVANCED_FACE ( 'NONE', ( #17220 ), #1703, .T. ) ;
#38960 = CARTESIAN_POINT ( 'NONE',  ( -48.47912675150885065, -175.3837268820161057, 6.938893903907228378E-15 ) ) ;
#38961 = CARTESIAN_POINT ( 'NONE',  ( -332.3517673607765914, -170.1129345408509153, -37.77875505479703122 ) ) ;
#38963 = ORIENTED_EDGE ( 'NONE', *, *, #45998, .F. ) ;
#38962 = CARTESIAN_POINT ( 'NONE',  ( -332.3517673607765914, -118.0087234915157381, -58.76657425099333665 ) ) ;
#38964 = ORIENTED_EDGE ( 'NONE', *, *, #44128, .T. ) ;
#38965 = DIRECTION ( 'NONE',  ( 0.9842305779475980509, 0.000000000000000000, -0.1768902751225666647 ) ) ;
#38966 = EDGE_CURVE ( 'NONE', #40042, #5249, #1763, .T. ) ;
#38967 = DIRECTION ( 'NONE',  ( 0.7948544414133565938, 0.000000000000000000, -0.6068001458185890984 ) ) ;
#38968 = EDGE_LOOP ( 'NONE', ( #27436, #42091, #27199, #1905 ) ) ;
#38969 = VERTEX_POINT ( 'NONE', #14061 ) ;
#38970 = PLANE ( 'NONE',  #20576 ) ;
#38971 = ORIENTED_EDGE ( 'NONE', *, *, #24358, .F. ) ;
#38972 = CARTESIAN_POINT ( 'NONE',  ( -130.7087404384255080, -175.3837268820161057, -94.14505102712755047 ) ) ;
#38973 = CARTESIAN_POINT ( 'NONE',  ( -68.21229068036655008, -183.6283474603465606, -123.4325817657429809 ) ) ;
#38974 = VECTOR ( 'NONE', #18460, 1000.000000000000000 ) ;
#38975 = VECTOR ( 'NONE', #23630, 1000.000000000000000 ) ;
#38976 = CARTESIAN_POINT ( 'NONE',  ( -336.3521761649654422, -182.2665742509934148, -5.491276508484069119 ) ) ;
#38977 = DIRECTION ( 'NONE',  ( -0.000000000000000000, 1.000000000000000000, -0.000000000000000000 ) ) ;
#38978 = VERTEX_POINT ( 'NONE', #42149 ) ;
#38979 = ORIENTED_EDGE ( 'NONE', *, *, #47029, .T. ) ;
#38980 = VECTOR ( 'NONE', #41349, 1000.000000000000114 ) ;
#38981 = ORIENTED_EDGE ( 'NONE', *, *, #32331, .T. ) ;
#38982 = ADVANCED_FACE ( 'NONE', ( #9335 ), #25874, .F. ) ;
#38983 = CARTESIAN_POINT ( 'NONE',  ( -108.5723883981723930, -177.1207230881787780, 109.6074810615846360 ) ) ;
#38984 = FACE_OUTER_BOUND ( 'NONE', #4616, .T. ) ;
#38985 = LINE ( 'NONE', #43716, #42523 ) ;
#38986 = CARTESIAN_POINT ( 'NONE',  ( -157.4685091425930636, -175.3837268820161057, -59.13814366165043168 ) ) ;
#38987 = DIRECTION ( 'NONE',  ( 0.000000000000000000, 0.000000000000000000, 1.000000000000000000 ) ) ;
#38988 = ORIENTED_EDGE ( 'NONE', *, *, #43380, .T. ) ;
#38989 = UNCERTAINTY_MEASURE_WITH_UNIT (LENGTH_MEASURE( 1.000000000000000082E-05 ), #28353, 'distance_accuracy_value', 'NONE');
#38990 = ADVANCED_FACE ( 'NONE', ( #49285 ), #37955, .T. ) ;
#38991 = CARTESIAN_POINT ( 'NONE',  ( -339.1964088526558498, -130.2355952558269507, -59.62073260661665586 ) ) ;
#38992 = CARTESIAN_POINT ( 'NONE',  ( -48.65601702663141737, -193.5000000000000000, -0.9842305779475923888 ) ) ;
#38993 = EDGE_CURVE ( 'NONE', #3778, #26482, #18539, .T. ) ;
#38994 = VERTEX_POINT ( 'NONE', #9079 ) ;
#38995 = ORIENTED_EDGE ( 'NONE', *, *, #41730, .T. ) ;
#38996 = EDGE_CURVE ( 'NONE', #33019, #34940, #50062, .T. ) ;
#38997 = DIRECTION ( 'NONE',  ( 0.000000000000000000, 0.000000000000000000, 1.000000000000000000 ) ) ;
#38998 = DIRECTION ( 'NONE',  ( -0.8757349421956412971, 0.000000000000000000, 0.4827922027307366970 ) ) ;
#38999 = LINE ( 'NONE', #35576, #5712 ) ;
#39000 = FACE_OUTER_BOUND ( 'NONE', #30286, .T. ) ;
#39001 = DIRECTION ( 'NONE',  ( -0.000000000000000000, -0.8229838658936596829, -0.5680647467311510379 ) ) ;
#39002 = ORIENTED_EDGE ( 'NONE', *, *, #27130, .T. ) ;
#39003 = PLANE ( 'NONE',  #38500 ) ;
#39004 = ORIENTED_EDGE ( 'NONE', *, *, #13584, .T. ) ;
#39005 = DIRECTION ( 'NONE',  ( 0.000000000000000000, 0.000000000000000000, 1.000000000000000000 ) ) ;
#39006 = CIRCLE ( 'NONE', #28209, 20.00000000000000000 ) ;
#39007 = CARTESIAN_POINT ( 'NONE',  ( -305.0000000000000568, -70.60684477890980304, -28.32515014536826214 ) ) ;
#39008 = EDGE_CURVE ( 'NONE', #33330, #41587, #10105, .T. ) ;
#39009 = ORIENTED_EDGE ( 'NONE', *, *, #23974, .F. ) ;
#39010 = CIRCLE ( 'NONE', #30644, 60.00000000000000000 ) ;
#39011 = VECTOR ( 'NONE', #21656, 1000.000000000000000 ) ;
#39012 = DIRECTION ( 'NONE',  ( 0.000000000000000000, -0.000000000000000000, -1.000000000000000000 ) ) ;
#39013 = DIRECTION ( 'NONE',  ( 0.000000000000000000, 0.000000000000000000, 1.000000000000000000 ) ) ;
#39014 = PLANE ( 'NONE',  #42454 ) ;
#39015 = DIRECTION ( 'NONE',  ( 0.000000000000000000, 0.000000000000000000, 1.000000000000000000 ) ) ;
#39016 = VECTOR ( 'NONE', #43440, 1000.000000000000000 ) ;
#39017 = CARTESIAN_POINT ( 'NONE',  ( 3.686287386450715076E-15, 0.000000000000000000, -46.00000000000000711 ) ) ;
#39018 = EDGE_LOOP ( 'NONE', ( #8349, #35129, #12609, #24525 ) ) ;
#39019 = VECTOR ( 'NONE', #30464, 1000.000000000000114 ) ;
#39020 = DIRECTION ( 'NONE',  ( 0.3202698538628416247, 0.000000000000000000, -0.9473263538541900619 ) ) ;
#39022 = ORIENTED_EDGE ( 'NONE', *, *, #19277, .F. ) ;
#39021 = DIRECTION ( 'NONE',  ( -0.000000000000000000, 1.000000000000000000, -0.000000000000000000 ) ) ;
#39023 = VECTOR ( 'NONE', #4338, 1000.000000000000000 ) ;
#39024 = ORIENTED_EDGE ( 'NONE', *, *, #29275, .T. ) ;
#39025 = DIRECTION ( 'NONE',  ( -0.000000000000000000, 1.000000000000000000, -0.000000000000000000 ) ) ;
#39026 = VECTOR ( 'NONE', #43903, 1000.000000000000000 ) ;
#39027 = EDGE_LOOP ( 'NONE', ( #41170, #1706, #33527, #7786 ) ) ;
#39028 = VECTOR ( 'NONE', #28581, 1000.000000000000000 ) ;
#39029 = DIRECTION ( 'NONE',  ( -0.9266896074318370369, 0.000000000000000000, 0.3758275821142292306 ) ) ;
#39030 = ORIENTED_EDGE ( 'NONE', *, *, #17473, .F. ) ;
#39031 = FACE_BOUND ( 'NONE', #27560, .T. ) ;
#39032 = CARTESIAN_POINT ( 'NONE',  ( -48.47912675150885065, -175.3837268820161057, 6.938893903907228378E-15 ) ) ;
#39033 = ORIENTED_EDGE ( 'NONE', *, *, #33812, .T. ) ;
#39034 = CARTESIAN_POINT ( 'NONE',  ( -330.4913330509368166, -181.6348283828473029, -14.84391218300937609 ) ) ;
#39035 = EDGE_CURVE ( 'NONE', #40551, #23392, #5977, .T. ) ;
#39036 = ADVANCED_FACE ( 'NONE', ( #29549 ), #47399, .T. ) ;
#39037 = CARTESIAN_POINT ( 'NONE',  ( -69.77312546433407192, -193.5000000000000000, 123.1729094355500109 ) ) ;
#39038 = CARTESIAN_POINT ( 'NONE',  ( -170.0000000000000284, -155.0173647354142759, 14.76740078976490622 ) ) ;
#39039 = ORIENTED_EDGE ( 'NONE', *, *, #8681, .F. ) ;
#39040 = ORIENTED_EDGE ( 'NONE', *, *, #35269, .T. ) ;
#39041 = ORIENTED_EDGE ( 'NONE', *, *, #40962, .F. ) ;
#39042 = CARTESIAN_POINT ( 'NONE',  ( -147.2362428880188077, -193.5000000000000000, -74.98773087994455011 ) ) ;
#39043 = LINE ( 'NONE', #5975, #10053 ) ;
#39044 = VECTOR ( 'NONE', #12387, 1000.000000000000000 ) ;
#39045 = PLANE ( 'NONE',  #20921 ) ;
#39046 = AXIS2_PLACEMENT_3D ( 'NONE', #20323, #36356, #20588 ) ;
#39047 = LINE ( 'NONE', #15424, #12741 ) ;
#39048 = DIRECTION ( 'NONE',  ( 0.000000000000000000, 0.000000000000000000, 1.000000000000000000 ) ) ;
#39049 = ORIENTED_EDGE ( 'NONE', *, *, #38466, .F. ) ;
#39050 = VECTOR ( 'NONE', #32632, 1000.000000000000000 ) ;
#39051 = ADVANCED_FACE ( 'NONE', ( #27151 ), #26385, .F. ) ;
#39052 = ADVANCED_FACE ( 'NONE', ( #14839 ), #11378, .T. ) ;
#39053 = CARTESIAN_POINT ( 'NONE',  ( -88.23625491228469286, -177.1207230881787780, 118.5089480183148254 ) ) ;
#39054 = ORIENTED_EDGE ( 'NONE', *, *, #23639, .T. ) ;
#39056 = VERTEX_POINT ( 'NONE', #34522 ) ;
#39055 = LINE ( 'NONE', #43265, #39060 ) ;
#39057 = VERTEX_POINT ( 'NONE', #31358 ) ;
#39058 = EDGE_CURVE ( 'NONE', #34403, #45844, #35333, .T. ) ;
#39059 = CARTESIAN_POINT ( 'NONE',  ( 73.87536152799695799, -193.5000000000000000, -25.58083653558413317 ) ) ;
#39060 = VECTOR ( 'NONE', #23316, 1000.000000000000000 ) ;
#39061 = CARTESIAN_POINT ( 'NONE',  ( -330.4913330509368166, -162.9984922102926532, -43.83057281297441676 ) ) ;
#39062 = AXIS2_PLACEMENT_3D ( 'NONE', #22310, #10227, #6038 ) ;
#39063 = EDGE_CURVE ( 'NONE', #12404, #19021, #11125, .T. ) ;
#39064 = CARTESIAN_POINT ( 'NONE',  ( 74.61260187273140332, -183.6283474603465606, -14.98512977653174794 ) ) ;
#39065 = CARTESIAN_POINT ( 'NONE',  ( -148.6149069237406195, -193.5000000000000000, -74.81861753132355375 ) ) ;
#39066 = VERTEX_POINT ( 'NONE', #38976 ) ;
#39067 = DIRECTION ( 'NONE',  ( -0.000000000000000000, 1.000000000000000000, 0.000000000000000000 ) ) ;
#39068 = AXIS2_PLACEMENT_3D ( 'NONE', #19247, #35256, #43666 ) ;
#39069 = EDGE_LOOP ( 'NONE', ( #49332, #9520, #43389, #27038 ) ) ;
#39070 = CIRCLE ( 'NONE', #38252, 125.0000000000000000 ) ;
#39071 = ORIENTED_EDGE ( 'NONE', *, *, #32729, .T. ) ;
#39072 = LINE ( 'NONE', #2044, #34589 ) ;
#39073 = FACE_OUTER_BOUND ( 'NONE', #30197, .T. ) ;
#39074 = ORIENTED_EDGE ( 'NONE', *, *, #31100, .T. ) ;
#39075 = CARTESIAN_POINT ( 'NONE',  ( -49.30901192927175458, -193.5000000000000000, -123.9972451320097093 ) ) ;
#39076 = LINE ( 'NONE', #3087, #12144 ) ;
#39077 = FACE_OUTER_BOUND ( 'NONE', #24194, .T. ) ;
#39078 = DIRECTION ( 'NONE',  ( 0.000000000000000000, 0.000000000000000000, 1.000000000000000000 ) ) ;
#39079 = ORIENTED_EDGE ( 'NONE', *, *, #10466, .F. ) ;
#39080 = LINE ( 'NONE', #3092, #48152 ) ;
#39081 = DIRECTION ( 'NONE',  ( 0.000000000000000000, 0.000000000000000000, -1.000000000000000000 ) ) ;
#39082 = PLANE ( 'NONE',  #2247 ) ;
#39083 = ORIENTED_EDGE ( 'NONE', *, *, #16740, .T. ) ;
#39084 = AXIS2_PLACEMENT_3D ( 'NONE', #234, #40434, #48080 ) ;
#39085 = CARTESIAN_POINT ( 'NONE',  ( -19.51863976943889867, -175.3837268820161057, 120.5706864261537277 ) ) ;
#39086 = VECTOR ( 'NONE', #38103, 1000.000000000000000 ) ;
#39087 = VECTOR ( 'NONE', #48877, 1000.000000000000114 ) ;
#39088 = DIRECTION ( 'NONE',  ( 0.9374196611341231167, 0.000000000000000000, -0.3482016354343928088 ) ) ;
#39089 = EDGE_LOOP ( 'NONE', ( #38602, #4929, #33571, #10488 ) ) ;
#39090 = DIRECTION ( 'NONE',  ( 0.000000000000000000, 0.000000000000000000, 1.000000000000000000 ) ) ;
#39091 = VERTEX_POINT ( 'NONE', #10620 ) ;
#39092 = EDGE_CURVE ( 'NONE', #1503, #22453, #23234, .T. ) ;
#39093 = FACE_OUTER_BOUND ( 'NONE', #20993, .T. ) ;
#39094 = FACE_BOUND ( 'NONE', #3208, .T. ) ;
#39095 = AXIS2_PLACEMENT_3D ( 'NONE', #37452, #1717, #49821 ) ;
#39096 = CARTESIAN_POINT ( 'NONE',  ( 57.31108707223382481, -175.3837268820161057, -66.58401203837755133 ) ) ;
#39097 = AXIS2_PLACEMENT_3D ( 'NONE', #11417, #27454, #3539 ) ;
#39098 = EDGE_CURVE ( 'NONE', #51600, #18514, #19294, .T. ) ;
#39099 = EDGE_CURVE ( 'NONE', #27859, #11977, #30577, .T. ) ;
#39100 = EDGE_CURVE ( 'NONE', #31777, #27449, #22967, .T. ) ;
#39101 = AXIS2_PLACEMENT_3D ( 'NONE', #43350, #11791, #50994 ) ;
#39102 = DIRECTION ( 'NONE',  ( 1.000000000000000000, 8.654812430365579069E-17, 1.050884489711633576E-17 ) ) ;
#39103 = ORIENTED_EDGE ( 'NONE', *, *, #21450, .F. ) ;
#39104 = EDGE_CURVE ( 'NONE', #26723, #41529, #26652, .T. ) ;
#39105 = ORIENTED_EDGE ( 'NONE', *, *, #48032, .F. ) ;
#39106 = VECTOR ( 'NONE', #19548, 1000.000000000000000 ) ;
#39107 = DIRECTION ( 'NONE',  ( 0.000000000000000000, -0.000000000000000000, 1.000000000000000000 ) ) ;
#39108 = ORIENTED_EDGE ( 'NONE', *, *, #2155, .T. ) ;
#39109 = EDGE_CURVE ( 'NONE', #25612, #602, #42416, .T. ) ;
#39110 = CARTESIAN_POINT ( 'NONE',  ( -365.0000000000001137, -168.5000000000000284, -10.00000000000000711 ) ) ;
#39111 = EDGE_CURVE ( 'NONE', #10774, #12239, #15099, .T. ) ;
#39112 = EDGE_CURVE ( 'NONE', #3787, #42007, #42090, .T. ) ;
#39113 = FACE_OUTER_BOUND ( 'NONE', #36628, .T. ) ;
#39114 = DIRECTION ( 'NONE',  ( 0.000000000000000000, -1.000000000000000000, 0.000000000000000000 ) ) ;
#39115 = VERTEX_POINT ( 'NONE', #2725 ) ;
#39118 = ORIENTED_EDGE ( 'NONE', *, *, #30111, .T. ) ;
#39117 = DIRECTION ( 'NONE',  ( 1.000000000000000000, 8.151826190875887961E-17, -3.091579882402674147E-17 ) ) ;
#39116 = CARTESIAN_POINT ( 'NONE',  ( -4.431386850739163386, 53.64904251590335349, -18.86752773431649999 ) ) ;
#39119 = AXIS2_PLACEMENT_3D ( 'NONE', #30611, #14350, #18799 ) ;
#39120 = VECTOR ( 'NONE', #12255, 1000.000000000000000 ) ;
#39121 = EDGE_CURVE ( 'NONE', #14481, #38037, #20253, .T. ) ;
#39122 = CARTESIAN_POINT ( 'NONE',  ( -49.13194886969936448, -183.6283474603465606, -0.7575112421616214675 ) ) ;
#39123 = EDGE_LOOP ( 'NONE', ( #7969, #3440, #4845, #45179 ) ) ;
#39124 = DIRECTION ( 'NONE',  ( -0.000000000000000000, -0.5680647467311485954, 0.8229838658936613482 ) ) ;
#39125 = ORIENTED_EDGE ( 'NONE', *, *, #40046, .T. ) ;
#39126 = AXIS2_PLACEMENT_3D ( 'NONE', #49460, #46034, #42061 ) ;
#39127 = ADVANCED_FACE ( 'NONE', ( #10360 ), #38720, .T. ) ;
#39128 = DIRECTION ( 'NONE',  ( 0.000000000000000000, 1.000000000000000000, 0.000000000000000000 ) ) ;
#39129 = VERTEX_POINT ( 'NONE', #46899 ) ;
#39131 = DIRECTION ( 'NONE',  ( -0.000000000000000000, 0.3546048870425463906, 0.9350162426854107256 ) ) ;
#39130 = FACE_OUTER_BOUND ( 'NONE', #15246, .T. ) ;
#39132 = EDGE_LOOP ( 'NONE', ( #41398, #48518, #25486, #32250 ) ) ;
#39133 = EDGE_CURVE ( 'NONE', #26117, #13237, #10880, .T. ) ;
#39134 = DIRECTION ( 'NONE',  ( 1.000000000000000000, -0.000000000000000000, 0.000000000000000000 ) ) ;
#39135 = ORIENTED_EDGE ( 'NONE', *, *, #31656, .F. ) ;
#39136 = CARTESIAN_POINT ( 'NONE',  ( 8.750818922897904528, -189.7472609257535510, -111.1293539894138434 ) ) ;
#39137 = VECTOR ( 'NONE', #9297, 1000.000000000000000 ) ;
#39138 = CARTESIAN_POINT ( 'NONE',  ( 43.33156026654913262, 35.00000000000000000, -51.04247435516399634 ) ) ;
#39139 = ORIENTED_EDGE ( 'NONE', *, *, #48140, .T. ) ;
#39140 = AXIS2_PLACEMENT_3D ( 'NONE', #3717, #40489, #32624 ) ;
#39141 = DIRECTION ( 'NONE',  ( -0.000000000000000000, 1.000000000000000000, -0.000000000000000000 ) ) ;
#39142 = DIRECTION ( 'NONE',  ( -0.000000000000000000, 1.000000000000000000, -0.000000000000000000 ) ) ;
#39143 = CARTESIAN_POINT ( 'NONE',  ( -336.3521761649654422, -182.5000000000000568, 2.632288850093980503 ) ) ;
#39144 = VECTOR ( 'NONE', #27259, 1000.000000000000114 ) ;
#39145 = AXIS2_PLACEMENT_3D ( 'NONE', #10194, #9684, #29907 ) ;
#39146 = DIRECTION ( 'NONE',  ( 1.000000000000000000, -8.151826190875929870E-17, -3.091579882402562597E-17 ) ) ;
#39147 = VERTEX_POINT ( 'NONE', #23486 ) ;
#39148 = DIRECTION ( 'NONE',  ( 0.000000000000000000, 0.000000000000000000, 1.000000000000000000 ) ) ;
#39149 = AXIS2_PLACEMENT_3D ( 'NONE', #46126, #26123, #22192 ) ;
#39150 = LINE ( 'NONE', #26806, #9513 ) ;
#39151 = EDGE_CURVE ( 'NONE', #24942, #21292, #46374, .T. ) ;
#39152 = DIRECTION ( 'NONE',  ( 0.000000000000000000, 0.000000000000000000, 1.000000000000000000 ) ) ;
#39153 = AXIS2_PLACEMENT_3D ( 'NONE', #29758, #21365, #37389 ) ;
#39154 = FACE_OUTER_BOUND ( 'NONE', #47141, .T. ) ;
#39155 = VERTEX_POINT ( 'NONE', #11893 ) ;
#39156 = CARTESIAN_POINT ( 'NONE',  ( -336.3521761649654422, -64.50000000000000000, -1.632288850093980725 ) ) ;
#39157 = CIRCLE ( 'NONE', #15570, 125.0000000000000000 ) ;
#39158 = CARTESIAN_POINT ( 'NONE',  ( 60.51025563957495024, -193.5000000000000000, 59.13814366165116354 ) ) ;
#39159 = DIRECTION ( 'NONE',  ( 0.01787127051204739914, -0.8746197071393964073, -0.4844801188631808198 ) ) ;
#39161 = ORIENTED_EDGE ( 'NONE', *, *, #17231, .T. ) ;
#39160 = DIRECTION ( 'NONE',  ( -0.000000000000000000, 1.000000000000000000, -0.000000000000000000 ) ) ;
#39162 = ORIENTED_EDGE ( 'NONE', *, *, #11242, .T. ) ;
#39163 = EDGE_CURVE ( 'NONE', #9746, #15667, #31989, .T. ) ;
#39164 = VECTOR ( 'NONE', #15909, 1000.000000000000000 ) ;
#39165 = CARTESIAN_POINT ( 'NONE',  ( -48.47912675150885065, -183.6283474603465606, 6.938893903907228378E-15 ) ) ;
#39166 = AXIS2_PLACEMENT_3D ( 'NONE', #33736, #41610, #30053 ) ;
#39167 = CARTESIAN_POINT ( 'NONE',  ( -112.7586829773731267, -175.3837268820161057, -107.2060569716373379 ) ) ;
#39168 = DIRECTION ( 'NONE',  ( -0.6068001458185890984, 0.000000000000000000, -0.7948544414133565938 ) ) ;
#39169 = LINE ( 'NONE', #3424, #6927 ) ;
#39170 = DIRECTION ( 'NONE',  ( 0.000000000000000000, -0.000000000000000000, 1.000000000000000000 ) ) ;
#39171 = VECTOR ( 'NONE', #23223, 1000.000000000000114 ) ;
#39172 = ORIENTED_EDGE ( 'NONE', *, *, #44089, .T. ) ;
#39173 = EDGE_CURVE ( 'NONE', #43321, #17649, #46278, .T. ) ;
#39174 = EDGE_CURVE ( 'NONE', #30367, #19842, #3756, .T. ) ;
#39175 = CARTESIAN_POINT ( 'NONE',  ( 4.010723116466015092, 52.52602521353311005, -19.70746035629181847 ) ) ;
#39176 = ADVANCED_FACE ( 'NONE', ( #4033 ), #12145, .T. ) ;
#39177 = EDGE_CURVE ( 'NONE', #17406, #10047, #20050, .T. ) ;
#39178 = ORIENTED_EDGE ( 'NONE', *, *, #7529, .T. ) ;
#39179 = AXIS2_PLACEMENT_3D ( 'NONE', #17502, #18004, #4888 ) ;
#39180 = ORIENTED_EDGE ( 'NONE', *, *, #49938, .F. ) ;
#39181 = CIRCLE ( 'NONE', #49254, 125.0000000000000000 ) ;
#39182 = VERTEX_POINT ( 'NONE', #32131 ) ;
#39183 = CARTESIAN_POINT ( 'NONE',  ( -339.1964088526558498, -144.3080463282022663, -56.27632902032068785 ) ) ;
#39184 = AXIS2_PLACEMENT_3D ( 'NONE', #23959, #51568, #19263 ) ;
#39186 = CIRCLE ( 'NONE', #46780, 125.0000000000000000 ) ;
#39185 = CARTESIAN_POINT ( 'NONE',  ( -60.86541030502398542, -177.1207230881787780, -124.3848060646151623 ) ) ;
#39187 = EDGE_LOOP ( 'NONE', ( #7729, #29688, #44010, #5777 ) ) ;
#39188 = CIRCLE ( 'NONE', #34173, 125.0000000000000000 ) ;
#39189 = CARTESIAN_POINT ( 'NONE',  ( -339.1964088526558498, -103.0458197858324496, 55.34326076196052213 ) ) ;
#39190 = DIRECTION ( 'NONE',  ( 0.000000000000000000, -0.6631226582407937498, 0.7485107481711024136 ) ) ;
#39193 = VERTEX_POINT ( 'NONE', #36076 ) ;
#39192 = DIRECTION ( 'NONE',  ( -0.2348860457809707758, 0.000000000000000000, -0.9720229140804138579 ) ) ;
#39191 = CARTESIAN_POINT ( 'NONE',  ( -48.47912675150885065, -121.5000000000000142, 6.938893903907228378E-15 ) ) ;
#39194 = ADVANCED_FACE ( 'NONE', ( #48176 ), #40522, .T. ) ;
#39195 = CARTESIAN_POINT ( 'NONE',  ( -238.7407812814481076, -213.5000000000000000, -9.999999999999987566 ) ) ;
#39196 = ORIENTED_EDGE ( 'NONE', *, *, #8288, .T. ) ;
#39197 = CARTESIAN_POINT ( 'NONE',  ( -73.70588833648349691, -183.6283474603465606, 121.4073237908568359 ) ) ;
#39198 = ORIENTED_EDGE ( 'NONE', *, *, #46223, .F. ) ;
#39199 = DIRECTION ( 'NONE',  ( 0.000000000000000000, -1.346129392433909288E-16, 1.000000000000000000 ) ) ;
#39200 = DIRECTION ( 'NONE',  ( -0.000000000000000000, 0.5680647467311540355, -0.8229838658936575735 ) ) ;
#39202 = CARTESIAN_POINT ( 'NONE',  ( -16.10442403432823255, -193.5000000000000000, -119.6996507684850286 ) ) ;
#39201 = CARTESIAN_POINT ( 'NONE',  ( -332.3517673607765914, -67.75522407825191351, 19.39547174791671935 ) ) ;
#39203 = ORIENTED_EDGE ( 'NONE', *, *, #17373, .T. ) ;
#39204 = EDGE_CURVE ( 'NONE', #39548, #12962, #38707, .T. ) ;
#39205 = FACE_OUTER_BOUND ( 'NONE', #12336, .T. ) ;
#39206 = VECTOR ( 'NONE', #45110, 1000.000000000000000 ) ;
#39207 = VERTEX_POINT ( 'NONE', #74 ) ;
#39208 = CARTESIAN_POINT ( 'NONE',  ( -48.47912675150885065, -189.7472609257535510, 6.938893903907228378E-15 ) ) ;
#39209 = CIRCLE ( 'NONE', #35008, 125.0000000000000000 ) ;
#39210 = CARTESIAN_POINT ( 'NONE',  ( -332.3517673607765914, -179.5993808087905279, -18.46045550523168899 ) ) ;
#39211 = EDGE_LOOP ( 'NONE', ( #42623, #27611, #39022, #28061 ) ) ;
#39212 = CARTESIAN_POINT ( 'NONE',  ( -330.4913330509368166, -68.51134412508180560, -21.38919645685231075 ) ) ;
#39213 = AXIS2_PLACEMENT_3D ( 'NONE', #5587, #21614, #33686 ) ;
#39214 = DIRECTION ( 'NONE',  ( -1.000000000000000000, 1.013386094502325718E-14, 2.497772389992443424E-15 ) ) ;
#39215 = EDGE_LOOP ( 'NONE', ( #15177, #12821, #48330, #5279 ) ) ;
#39216 = FACE_BOUND ( 'NONE', #41952, .T. ) ;
#39217 = CARTESIAN_POINT ( 'NONE',  ( 0.000000000000000000, -123.5000000000002416, -59.00000000000002132 ) ) ;
#39218 = EDGE_LOOP ( 'NONE', ( #8901, #23815, #17767, #37403 ) ) ;
#39219 = CARTESIAN_POINT ( 'NONE',  ( -48.47912675150885065, -177.1207230881787780, 6.938893903907228378E-15 ) ) ;
#39220 = VERTEX_POINT ( 'NONE', #44229 ) ;
#39221 = AXIS2_PLACEMENT_3D ( 'NONE', #34832, #10156, #50377 ) ;
#39222 = CARTESIAN_POINT ( 'NONE',  ( 27.50603775690334274, -189.7472609257535510, -99.25348746834811209 ) ) ;
#39223 = CIRCLE ( 'NONE', #32510, 125.0000000000000000 ) ;
#39224 = CARTESIAN_POINT ( 'NONE',  ( -48.41988612361514299, -189.7472609257535510, -0.9982437317643144681 ) ) ;
#39225 = ORIENTED_EDGE ( 'NONE', *, *, #28066, .T. ) ;
#39226 = AXIS2_PLACEMENT_3D ( 'NONE', #1722, #29571, #41654 ) ;
#39227 = PLANE ( 'NONE',  #24375 ) ;
#39228 = CARTESIAN_POINT ( 'NONE',  ( 0.000000000000000000, -53.50000000000000000, 0.000000000000000000 ) ) ;
#39229 = LINE ( 'NONE', #19507, #36660 ) ;
#39230 = VECTOR ( 'NONE', #16547, 1000.000000000000000 ) ;
#39231 = FACE_OUTER_BOUND ( 'NONE', #47699, .T. ) ;
#39233 = VECTOR ( 'NONE', #47817, 999.9999999999998863 ) ;
#39232 = FACE_OUTER_BOUND ( 'NONE', #34778, .T. ) ;
#39234 = DIRECTION ( 'NONE',  ( -0.6749830015182196608, 0.000000000000000000, 0.7378332790417189146 ) ) ;
#39235 = CARTESIAN_POINT ( 'NONE',  ( -332.3517673607765914, -75.87119766449505676, -34.85916744524372746 ) ) ;
#39237 = ORIENTED_EDGE ( 'NONE', *, *, #3538, .T. ) ;
#39236 = CARTESIAN_POINT ( 'NONE',  ( -48.47912675150885065, -177.1207230881787780, 6.938893903907228378E-15 ) ) ;
#39238 = ORIENTED_EDGE ( 'NONE', *, *, #49912, .T. ) ;
#39239 = ADVANCED_FACE ( 'NONE', ( #43708 ), #4542, .T. ) ;
#39240 = EDGE_CURVE ( 'NONE', #48318, #18389, #47916, .T. ) ;
#39241 = DIRECTION ( 'NONE',  ( 0.000000000000000000, 0.000000000000000000, -1.000000000000000000 ) ) ;
#39242 = LINE ( 'NONE', #23226, #25464 ) ;
#39243 = VERTEX_POINT ( 'NONE', #8226 ) ;
#39244 = VECTOR ( 'NONE', #32414, 999.9999999999998863 ) ;
#39245 = CIRCLE ( 'NONE', #8187, 125.0000000000000000 ) ;
#39246 = ORIENTED_EDGE ( 'NONE', *, *, #2860, .T. ) ;
#39247 = CARTESIAN_POINT ( 'NONE',  ( -99.22478721462985618, -189.7472609257535510, -113.1409892739921901 ) ) ;
#39248 = ORIENTED_EDGE ( 'NONE', *, *, #7511, .F. ) ;
#39249 = DIRECTION ( 'NONE',  ( 1.000000000000000000, 0.000000000000000000, 8.718379230999707126E-17 ) ) ;
#39250 = LINE ( 'NONE', #30322, #7380 ) ;
#39251 = AXIS2_PLACEMENT_3D ( 'NONE', #17995, #22188, #32968 ) ;
#39252 = DIRECTION ( 'NONE',  ( 0.6528221181905174975, 0.000000000000000000, 0.7575112421616236880 ) ) ;
#39253 = DIRECTION ( 'NONE',  ( 0.000000000000000000, 1.000000000000000000, 0.000000000000000000 ) ) ;
#39254 = ORIENTED_EDGE ( 'NONE', *, *, #921, .F. ) ;
#39255 = ORIENTED_EDGE ( 'NONE', *, *, #40966, .F. ) ;
#39256 = ORIENTED_EDGE ( 'NONE', *, *, #2010, .F. ) ;
#39257 = DIRECTION ( 'NONE',  ( 0.000000000000000000, 0.000000000000000000, -1.000000000000000000 ) ) ;
#39258 = CARTESIAN_POINT ( 'NONE',  ( 43.63512310656540905, -175.3837268820161057, 84.49831343337136502 ) ) ;
#39259 = CIRCLE ( 'NONE', #7387, 125.0000000000000000 ) ;
#39260 = DIRECTION ( 'NONE',  ( -1.000000000000000000, 0.000000000000000000, 0.000000000000000000 ) ) ;
#39261 = EDGE_CURVE ( 'NONE', #23501, #5804, #47125, .T. ) ;
#39262 = VECTOR ( 'NONE', #28980, 1000.000000000000000 ) ;
#39263 = CARTESIAN_POINT ( 'NONE',  ( -73.94077438226447896, -177.1207230881787780, 122.3793467049372481 ) ) ;
#39264 = CARTESIAN_POINT ( 'NONE',  ( -43.48323084606168720, -193.5000000000000000, 124.9001241957026167 ) ) ;
#39265 = ORIENTED_EDGE ( 'NONE', *, *, #5937, .T. ) ;
#39266 = LINE ( 'NONE', #35316, #44099 ) ;
#39267 = CARTESIAN_POINT ( 'NONE',  ( -145.6517069852673103, -189.7472609257535510, 78.62880929222940551 ) ) ;
#39268 = EDGE_CURVE ( 'NONE', #33217, #14253, #2628, .T. ) ;
#39269 = VECTOR ( 'NONE', #42818, 1000.000000000000000 ) ;
#39270 = ORIENTED_EDGE ( 'NONE', *, *, #16947, .T. ) ;
#39271 = ORIENTED_EDGE ( 'NONE', *, *, #30897, .T. ) ;
#39272 = DIRECTION ( 'NONE',  ( 0.9982437317643217956, 0.000000000000000000, -0.05924062789370748011 ) ) ;
#39273 = DIRECTION ( 'NONE',  ( 1.000000000000000000, 0.000000000000000000, 0.000000000000000000 ) ) ;
#39274 = ORIENTED_EDGE ( 'NONE', *, *, #43847, .T. ) ;
#39275 = DIRECTION ( 'NONE',  ( 0.000000000000000000, -1.000000000000000000, 0.000000000000000000 ) ) ;
#39276 = FACE_OUTER_BOUND ( 'NONE', #47982, .T. ) ;
#39277 = LINE ( 'NONE', #26923, #9198 ) ;
#39278 = ORIENTED_EDGE ( 'NONE', *, *, #20184, .F. ) ;
#39280 = ADVANCED_FACE ( 'NONE', ( #40262 ), #4278, .F. ) ;
#39279 = FACE_OUTER_BOUND ( 'NONE', #33556, .T. ) ;
#39281 = ORIENTED_EDGE ( 'NONE', *, *, #46193, .T. ) ;
#39282 = CARTESIAN_POINT ( 'NONE',  ( -48.93575598890257794, -193.5000000000000000, 0.8896570909947506545 ) ) ;
#39283 = CIRCLE ( 'NONE', #46881, 125.0000000000000000 ) ;
#39284 = AXIS2_PLACEMENT_3D ( 'NONE', #42502, #2566, #7288 ) ;
#39285 = CARTESIAN_POINT ( 'NONE',  ( -133.8011377042516301, -193.5000000000000000, -91.35181687837437892 ) ) ;
#39286 = ORIENTED_EDGE ( 'NONE', *, *, #45916, .F. ) ;
#39287 = VECTOR ( 'NONE', #37582, 1000.000000000000000 ) ;
#39288 = CARTESIAN_POINT ( 'NONE',  ( -168.4003408533108086, -183.6283474603465606, -35.26900067126612726 ) ) ;
#39289 = DIRECTION ( 'NONE',  ( 0.000000000000000000, 0.000000000000000000, -1.000000000000000000 ) ) ;
#39290 = PLANE ( 'NONE',  #22359 ) ;
#39291 = DIRECTION ( 'NONE',  ( 0.000000000000000000, -0.000000000000000000, -1.000000000000000000 ) ) ;
#39292 = EDGE_CURVE ( 'NONE', #26252, #41591, #16065, .T. ) ;
#39293 = DIRECTION ( 'NONE',  ( 0.000000000000000000, -1.000000000000000000, -0.000000000000000000 ) ) ;
#39294 = ORIENTED_EDGE ( 'NONE', *, *, #31937, .F. ) ;
#39295 = ORIENTED_EDGE ( 'NONE', *, *, #11621, .F. ) ;
#39296 = AXIS2_PLACEMENT_3D ( 'NONE', #7579, #34407, #42803 ) ;
#39297 = LINE ( 'NONE', #3301, #10910 ) ;
#39299 = VERTEX_POINT ( 'NONE', #24502 ) ;
#39298 = PLANE ( 'NONE',  #19536 ) ;
#39300 = ORIENTED_EDGE ( 'NONE', *, *, #16049, .T. ) ;
#39301 = CARTESIAN_POINT ( 'NONE',  ( -126.2322430781613605, -183.6283474603465606, 97.87467957288053810 ) ) ;
#39302 = EDGE_CURVE ( 'NONE', #6939, #13237, #41223, .T. ) ;
#39303 = VECTOR ( 'NONE', #24404, 1000.000000000000000 ) ;
#39304 = FACE_OUTER_BOUND ( 'NONE', #31921, .T. ) ;
#39305 = EDGE_CURVE ( 'NONE', #19975, #14630, #28693, .T. ) ;
#39306 = VERTEX_POINT ( 'NONE', #4814 ) ;
#39307 = LINE ( 'NONE', #3309, #27285 ) ;
#39308 = DIRECTION ( 'NONE',  ( -1.000000000000000000, -0.000000000000000000, 0.000000000000000000 ) ) ;
#39309 = ORIENTED_EDGE ( 'NONE', *, *, #49274, .F. ) ;
#39310 = LINE ( 'NONE', #25604, #25020 ) ;
#39311 = LINE ( 'NONE', #47732, #31135 ) ;
#39312 = FACE_OUTER_BOUND ( 'NONE', #19807, .T. ) ;
#39313 = ORIENTED_EDGE ( 'NONE', *, *, #24913, .F. ) ;
#39314 = VERTEX_POINT ( 'NONE', #31616 ) ;
#39315 = EDGE_LOOP ( 'NONE', ( #18973, #9141, #36770, #5187 ) ) ;
#39316 = CARTESIAN_POINT ( 'NONE',  ( -48.47912675150885065, -189.7472609257535510, 6.938893903907228378E-15 ) ) ;
#39317 = EDGE_CURVE ( 'NONE', #6162, #16187, #15832, .T. ) ;
#39318 = DIRECTION ( 'NONE',  ( 0.000000000000000000, 1.000000000000000000, 0.000000000000000000 ) ) ;
#39319 = AXIS2_PLACEMENT_3D ( 'NONE', #45884, #9878, #25901 ) ;
#39320 = VECTOR ( 'NONE', #34661, 1000.000000000000000 ) ;
#39321 = EDGE_CURVE ( 'NONE', #16323, #15864, #11652, .T. ) ;
#39322 = CARTESIAN_POINT ( 'NONE',  ( -339.1964088526558498, -84.08827740916129301, -45.24064679492073537 ) ) ;
#39323 = CARTESIAN_POINT ( 'NONE',  ( 0.000000000000000000, 28.00000000000000355, 0.000000000000000000 ) ) ;
#39324 = VERTEX_POINT ( 'NONE', #32902 ) ;
#39325 = AXIS2_PLACEMENT_3D ( 'NONE', #27552, #35425, #7830 ) ;
#39326 = DIRECTION ( 'NONE',  ( 0.000000000000000000, -1.000000000000000000, 0.000000000000000000 ) ) ;
#39327 = VERTEX_POINT ( 'NONE', #29741 ) ;
#39329 = ORIENTED_EDGE ( 'NONE', *, *, #11898, .F. ) ;
#39328 = CARTESIAN_POINT ( 'NONE',  ( -12.10142301649613827, -189.7472609257535510, -118.5439281552630746 ) ) ;
#39330 = CIRCLE ( 'NONE', #16700, 60.00000000000000000 ) ;
#39331 = ORIENTED_EDGE ( 'NONE', *, *, #29013, .T. ) ;
#39332 = DIRECTION ( 'NONE',  ( 0.000000000000000000, 0.000000000000000000, -1.000000000000000000 ) ) ;
#39333 = CARTESIAN_POINT ( 'NONE',  ( 37.99238433767461487, -175.3837268820161057, -90.26448786734026442 ) ) ;
#39334 = DIRECTION ( 'NONE',  ( 1.000000000000000000, 8.465038975556392596E-17, -2.086444717177575158E-17 ) ) ;
#39335 = ORIENTED_EDGE ( 'NONE', *, *, #9573, .F. ) ;
#39336 = PLANE ( 'NONE',  #7410 ) ;
#39337 = EDGE_LOOP ( 'NONE', ( #31578, #29181, #51436, #13644 ) ) ;
#39338 = CIRCLE ( 'NONE', #29288, 125.0000000000000000 ) ;
#39339 = VERTEX_POINT ( 'NONE', #33941 ) ;
#39340 = LINE ( 'NONE', #3594, #19558 ) ;
#39341 = DIRECTION ( 'NONE',  ( -0.9374196611341206742, 0.000000000000000000, -0.3482016354343996367 ) ) ;
#39342 = CARTESIAN_POINT ( 'NONE',  ( -37.08895481556041318, -183.6283474603465606, 124.4799742258550452 ) ) ;
#39343 = FACE_OUTER_BOUND ( 'NONE', #40328, .T. ) ;
#39344 = EDGE_CURVE ( 'NONE', #41229, #12335, #25546, .T. ) ;
#39345 = DIRECTION ( 'NONE',  ( 0.1768902751225592818, 0.000000000000000000, 0.9842305779475992722 ) ) ;
#39346 = DIRECTION ( 'NONE',  ( 0.000000000000000000, -0.000000000000000000, 1.000000000000000000 ) ) ;
#39347 = ORIENTED_EDGE ( 'NONE', *, *, #34971, .F. ) ;
#39348 = DIRECTION ( 'NONE',  ( 0.000000000000000000, 1.000000000000000000, -0.000000000000000000 ) ) ;
#39349 = CARTESIAN_POINT ( 'NONE',  ( -167.6453766917639427, -183.6283474603465606, 37.74128873232411507 ) ) ;
#39350 = CARTESIAN_POINT ( 'NONE',  ( 0.000000000000000000, -71.25809448646026567, 27.41866715058169390 ) ) ;
#39351 = VERTEX_POINT ( 'NONE', #49494 ) ;
#39352 = AXIS2_PLACEMENT_3D ( 'NONE', #24434, #28098, #783 ) ;
#39353 = LINE ( 'NONE', #3359, #9659 ) ;
#39354 = AXIS2_PLACEMENT_3D ( 'NONE', #19657, #20178, #200 ) ;
#39355 = FACE_OUTER_BOUND ( 'NONE', #8189, .T. ) ;
#39356 = ORIENTED_EDGE ( 'NONE', *, *, #23642, .T. ) ;
#39357 = DIRECTION ( 'NONE',  ( -0.000000000000000000, 1.000000000000000000, -0.000000000000000000 ) ) ;
#39358 = EDGE_CURVE ( 'NONE', #42195, #43059, #1648, .T. ) ;
#39359 = ORIENTED_EDGE ( 'NONE', *, *, #33020, .F. ) ;
#39360 = ADVANCED_FACE ( 'NONE', ( #5072 ), #21086, .T. ) ;
#39361 = VECTOR ( 'NONE', #18811, 1000.000000000000000 ) ;
#39362 = FACE_OUTER_BOUND ( 'NONE', #6336, .T. ) ;
#39363 = EDGE_CURVE ( 'NONE', #20713, #39399, #49734, .T. ) ;
#39364 = FACE_BOUND ( 'NONE', #46273, .T. ) ;
#39365 = CARTESIAN_POINT ( 'NONE',  ( -330.4913330509368166, -115.8919814278871598, -58.50955523165758621 ) ) ;
#39366 = CARTESIAN_POINT ( 'NONE',  ( -123.5870580700902508, -193.5000000000000000, -98.66508442481455177 ) ) ;
#39367 = ORIENTED_EDGE ( 'NONE', *, *, #41095, .T. ) ;
#39368 = ORIENTED_EDGE ( 'NONE', *, *, #41365, .F. ) ;
#39369 = DIRECTION ( 'NONE',  ( 0.000000000000000000, 0.000000000000000000, 1.000000000000000000 ) ) ;
#39370 = VERTEX_POINT ( 'NONE', #37646 ) ;
#39371 = DIRECTION ( 'NONE',  ( -0.9473263538541899509, 0.000000000000000000, -0.3202698538628415692 ) ) ;
#39372 = CARTESIAN_POINT ( 'NONE',  ( -330.4913330509368166, -89.57268800991444380, 48.27201571435978877 ) ) ;
#39373 = DIRECTION ( 'NONE',  ( 0.9785564922995060311, 0.000000000000000000, -0.2059786187410889424 ) ) ;
#39374 = ORIENTED_EDGE ( 'NONE', *, *, #27765, .T. ) ;
#39377 = ORIENTED_EDGE ( 'NONE', *, *, #35617, .F. ) ;
#39376 = FACE_OUTER_BOUND ( 'NONE', #44878, .T. ) ;
#39375 = PLANE ( 'NONE',  #1495 ) ;
#39378 = VECTOR ( 'NONE', #42984, 1000.000000000000227 ) ;
#39379 = PLANE ( 'NONE',  #47493 ) ;
#39380 = VERTEX_POINT ( 'NONE', #5862 ) ;
#39381 = FACE_OUTER_BOUND ( 'NONE', #24610, .T. ) ;
#39382 = AXIS2_PLACEMENT_3D ( 'NONE', #24845, #30018, #28265 ) ;
#39383 = ORIENTED_EDGE ( 'NONE', *, *, #12163, .F. ) ;
#39384 = LINE ( 'NONE', #51492, #43510 ) ;
#39385 = ORIENTED_EDGE ( 'NONE', *, *, #38702, .T. ) ;
#39387 = LINE ( 'NONE', #27042, #20797 ) ;
#39386 = CARTESIAN_POINT ( 'NONE',  ( -85.77912150413021664, -175.3837268820161057, -119.3051146910911768 ) ) ;
#39388 = ORIENTED_EDGE ( 'NONE', *, *, #45396, .T. ) ;
#39389 = DIRECTION ( 'NONE',  ( 1.000000000000000000, -0.000000000000000000, -0.000000000000000000 ) ) ;
#39390 = ORIENTED_EDGE ( 'NONE', *, *, #3447, .F. ) ;
#39391 = DIRECTION ( 'NONE',  ( -0.02963332782255633305, 0.000000000000000000, -0.9995608365087944591 ) ) ;
#39392 = CARTESIAN_POINT ( 'NONE',  ( -91.84482189527193441, -175.3837268820161057, -117.2365833888816695 ) ) ;
#39393 = PLANE ( 'NONE',  #7072 ) ;
#39394 = DIRECTION ( 'NONE',  ( -0.000000000000000000, 1.000000000000000000, -0.000000000000000000 ) ) ;
#39395 = CARTESIAN_POINT ( 'NONE',  ( 24.88090138098523241, -183.6283474603465606, 99.97252634603304955 ) ) ;
#39396 = DIRECTION ( 'NONE',  ( 0.000000000000000000, -0.1205366802553130001, 0.9927088740980551940 ) ) ;
#39397 = EDGE_CURVE ( 'NONE', #20913, #36158, #47949, .T. ) ;
#39398 = EDGE_CURVE ( 'NONE', #32761, #49503, #9787, .T. ) ;
#39399 = VERTEX_POINT ( 'NONE', #6113 ) ;
#39400 = ADVANCED_FACE ( 'NONE', ( #21879 ), #21351, .T. ) ;
#39401 = DIRECTION ( 'NONE',  ( 0.1884548733085491812, -2.775557561562891351E-17, 0.9820818503191366400 ) ) ;
#39402 = PLANE ( 'NONE',  #14549 ) ;
#39403 = FACE_OUTER_BOUND ( 'NONE', #11257, .T. ) ;
#39404 = EDGE_CURVE ( 'NONE', #41896, #4643, #33695, .T. ) ;
#39405 = FACE_OUTER_BOUND ( 'NONE', #37578, .T. ) ;
#39406 = ORIENTED_EDGE ( 'NONE', *, *, #31455, .T. ) ;
#39407 = CARTESIAN_POINT ( 'NONE',  ( 57.12946453413545100, -175.3837268820161057, 66.87170886602000053 ) ) ;
#39408 = EDGE_CURVE ( 'NONE', #13737, #153, #5157, .T. ) ;
#39409 = LINE ( 'NONE', #47321, #50454 ) ;
#39410 = EDGE_CURVE ( 'NONE', #19952, #19715, #853, .T. ) ;
#39411 = DIRECTION ( 'NONE',  ( 0.000000000000000000, 0.000000000000000000, 1.000000000000000000 ) ) ;
#39413 = VERTEX_POINT ( 'NONE', #49220 ) ;
#39412 = DIRECTION ( 'NONE',  ( -0.000000000000000000, 1.000000000000000000, -0.000000000000000000 ) ) ;
#39414 = VERTEX_POINT ( 'NONE', #17433 ) ;
#39415 = ADVANCED_FACE ( 'NONE', ( #1894 ), #17931, .T. ) ;
#39416 = VERTEX_POINT ( 'NONE', #26065 ) ;
#39417 = ADVANCED_FACE ( 'NONE', ( #33454 ), #48953, .T. ) ;
#39418 = CARTESIAN_POINT ( 'NONE',  ( -171.7589556598192360, -183.6283474603465606, -13.35228579481114863 ) ) ;
#39419 = EDGE_CURVE ( 'NONE', #48198, #16597, #45022, .T. ) ;
#39420 = VECTOR ( 'NONE', #45081, 1000.000000000000000 ) ;
#39421 = DIRECTION ( 'NONE',  ( 0.000000000000000000, 1.000000000000000000, 0.000000000000000000 ) ) ;
#39422 = CARTESIAN_POINT ( 'NONE',  ( -127.0132498732365889, -193.5000000000000000, 97.24912084693261249 ) ) ;
#39423 = CARTESIAN_POINT ( 'NONE',  ( -180.0000000000000568, -123.5000000000000284, 41.63467731922665394 ) ) ;
#39424 = EDGE_CURVE ( 'NONE', #14713, #8278, #45534, .T. ) ;
#39425 = EDGE_LOOP ( 'NONE', ( #44646, #2162, #37533, #38099 ) ) ;
#39426 = DIRECTION ( 'NONE',  ( -0.000000000000000000, 1.000000000000000000, -0.000000000000000000 ) ) ;
#39427 = VERTEX_POINT ( 'NONE', #25294 ) ;
#39428 = ORIENTED_EDGE ( 'NONE', *, *, #34013, .T. ) ;
#39429 = VERTEX_POINT ( 'NONE', #51043 ) ;
#39430 = FACE_OUTER_BOUND ( 'NONE', #26080, .T. ) ;
#39431 = CARTESIAN_POINT ( 'NONE',  ( -173.3968853974275817, -193.5000000000000000, 4.533605064404221174 ) ) ;
#39432 = ORIENTED_EDGE ( 'NONE', *, *, #16978, .F. ) ;
#39433 = EDGE_CURVE ( 'NONE', #33166, #20294, #10817, .T. ) ;
#39434 = CIRCLE ( 'NONE', #31078, 125.0000000000000000 ) ;
#39435 = VECTOR ( 'NONE', #19010, 1000.000000000000000 ) ;
#39436 = DIRECTION ( 'NONE',  ( -0.000000000000000000, 1.000000000000000000, 0.000000000000000000 ) ) ;
#39437 = DIRECTION ( 'NONE',  ( -1.000000000000000000, -0.000000000000000000, 0.000000000000000000 ) ) ;
#39440 = ORIENTED_EDGE ( 'NONE', *, *, #41298, .F. ) ;
#39439 = LINE ( 'NONE', #51291, #11530 ) ;
#39438 = LINE ( 'NONE', #21297, #29174 ) ;
#39441 = CARTESIAN_POINT ( 'NONE',  ( -49.13194886969938580, -189.7472609257535510, 0.7575112421616214675 ) ) ;
#39442 = ORIENTED_EDGE ( 'NONE', *, *, #40046, .F. ) ;
#39443 = LINE ( 'NONE', #16317, #41494 ) ;
#39444 = VERTEX_POINT ( 'NONE', #47340 ) ;
#39445 = CARTESIAN_POINT ( 'NONE',  ( -330.4913330509368166, -103.0458197858332312, -55.34326076196081345 ) ) ;
#39446 = CARTESIAN_POINT ( 'NONE',  ( -336.3521761649653854, -82.50558083279611310, 43.81161486573607533 ) ) ;
#39448 = DIRECTION ( 'NONE',  ( 0.000000000000000000, 0.000000000000000000, 1.000000000000000000 ) ) ;
#39447 = DIRECTION ( 'NONE',  ( 0.000000000000000000, -0.000000000000000000, 1.000000000000000000 ) ) ;
#39449 = ORIENTED_EDGE ( 'NONE', *, *, #42726, .F. ) ;
#39450 = EDGE_CURVE ( 'NONE', #33330, #24129, #18962, .T. ) ;
#39451 = CARTESIAN_POINT ( 'NONE',  ( 61.98524708613674505, -177.1207230881787780, 56.33604425924833237 ) ) ;
#39452 = DIRECTION ( 'NONE',  ( -0.000000000000000000, 1.000000000000000000, 0.000000000000000000 ) ) ;
#39454 = VECTOR ( 'NONE', #450, 1000.000000000000000 ) ;
#39453 =( NAMED_UNIT ( * ) PLANE_ANGLE_UNIT ( ) SI_UNIT ( $, .RADIAN. ) );
#39455 = EDGE_LOOP ( 'NONE', ( #16168, #40603, #37122, #14796 ) ) ;
#39456 = DIRECTION ( 'NONE',  ( -0.000000000000000000, 1.000000000000000000, -0.000000000000000000 ) ) ;
#39457 = DIRECTION ( 'NONE',  ( 0.000000000000000000, 0.000000000000000000, -1.000000000000000000 ) ) ;
#39458 = EDGE_CURVE ( 'NONE', #10970, #2101, #15239, .T. ) ;
#39459 = ADVANCED_FACE ( 'NONE', ( #26579 ), #15033, .T. ) ;
#39460 = ADVANCED_FACE ( 'NONE', ( #34718 ), #31293, .T. ) ;
#39461 = ORIENTED_EDGE ( 'NONE', *, *, #31463, .F. ) ;
#39462 = ADVANCED_FACE ( 'NONE', ( #18192 ), #22130, .F. ) ;
#39463 = FACE_OUTER_BOUND ( 'NONE', #44947, .T. ) ;
#39464 = DIRECTION ( 'NONE',  ( 0.000000000000000000, 0.000000000000000000, -1.000000000000000000 ) ) ;
#39465 = EDGE_CURVE ( 'NONE', #7505, #14417, #50768, .T. ) ;
#39466 = EDGE_LOOP ( 'NONE', ( #31524, #38579, #39848, #1394 ) ) ;
#39467 = DIRECTION ( 'NONE',  ( 0.000000000000000000, 1.595945597898662527E-14, 1.000000000000000000 ) ) ;
#39468 = EDGE_LOOP ( 'NONE', ( #31361, #48780, #51876, #30156 ) ) ;
#39469 = DIRECTION ( 'NONE',  ( 0.4031234292879665171, 0.000000000000000000, 0.9151456172430210145 ) ) ;
#39470 = EDGE_CURVE ( 'NONE', #20555, #3885, #6629, .T. ) ;
#39471 = FACE_OUTER_BOUND ( 'NONE', #27748, .T. ) ;
#39472 = CARTESIAN_POINT ( 'NONE',  ( -91.22542124915045747, -175.3837268820161057, 117.4638425504669925 ) ) ;
#39473 = CARTESIAN_POINT ( 'NONE',  ( -339.1964088526558498, -157.4273119900853146, -48.27201571435997352 ) ) ;
#39474 = CARTESIAN_POINT ( 'NONE',  ( -41.90263914168912152, -193.5000000000000000, -124.8268793598473536 ) ) ;
#39475 = EDGE_CURVE ( 'NONE', #1228, #38434, #22649, .T. ) ;
#39476 = VECTOR ( 'NONE', #31554, 1000.000000000000000 ) ;
#39477 = ADVANCED_FACE ( 'NONE', ( #30269 ), #11313, .F. ) ;
#39478 = VECTOR ( 'NONE', #573, 1000.000000000000000 ) ;
#39479 = PLANE ( 'NONE',  #33003 ) ;
#39480 = EDGE_CURVE ( 'NONE', #38994, #9854, #40424, .T. ) ;
#39481 = LINE ( 'NONE', #15853, #31194 ) ;
#39482 = DIRECTION ( 'NONE',  ( 0.8858462335218260097, -0.000000000000000000, -0.4639789333096864810 ) ) ;
#39484 = ORIENTED_EDGE ( 'NONE', *, *, #47204, .T. ) ;
#39483 = CARTESIAN_POINT ( 'NONE',  ( -30.00000000000000000, -43.50000000000000000, -30.00000000000000711 ) ) ;
#39485 = EDGE_CURVE ( 'NONE', #13511, #30309, #26171, .T. ) ;
#39486 = ORIENTED_EDGE ( 'NONE', *, *, #3047, .F. ) ;
#39487 = PLANE ( 'NONE',  #13191 ) ;
#39488 = EDGE_CURVE ( 'NONE', #34611, #9242, #34985, .T. ) ;
#39489 = DIRECTION ( 'NONE',  ( 0.000000000000000000, 1.000000000000000000, -0.000000000000000000 ) ) ;
#39490 = ORIENTED_EDGE ( 'NONE', *, *, #50713, .F. ) ;
#39491 = ORIENTED_EDGE ( 'NONE', *, *, #23200, .T. ) ;
#39492 = AXIS2_PLACEMENT_3D ( 'NONE', #18261, #34281, #21933 ) ;
#39493 = DIRECTION ( 'NONE',  ( -0.000000000000000000, -0.5680647467311485954, 0.8229838658936613482 ) ) ;
#39494 = ORIENTED_EDGE ( 'NONE', *, *, #38328, .T. ) ;
#39495 = DIRECTION ( 'NONE',  ( -0.000000000000000000, 1.000000000000000000, -0.000000000000000000 ) ) ;
#39496 = LINE ( 'NONE', #19782, #31712 ) ;
#39497 = CARTESIAN_POINT ( 'NONE',  ( 69.14211578623219623, -183.6283474603465606, 42.31126686685117733 ) ) ;
#39498 = CARTESIAN_POINT ( 'NONE',  ( -339.1964088526558498, -89.00580675195261904, 49.09328500076523483 ) ) ;
#39499 = ORIENTED_EDGE ( 'NONE', *, *, #10256, .F. ) ;
#39500 = ORIENTED_EDGE ( 'NONE', *, *, #17686, .F. ) ;
#39501 = ORIENTED_EDGE ( 'NONE', *, *, #16517, .F. ) ;
#39502 = ADVANCED_FACE ( 'NONE', ( #50262 ), #2664, .F. ) ;
#39503 = CARTESIAN_POINT ( 'NONE',  ( -170.0000000000000284, -113.5000000000000142, 39.99999999999998579 ) ) ;
#39504 = DIRECTION ( 'NONE',  ( 0.4566292373937077542, 0.000000000000000000, 0.8896570909947499883 ) ) ;
#39505 = DIRECTION ( 'NONE',  ( 0.9564009842765202052, 0.000000000000000000, 0.2920567706369833760 ) ) ;
#39506 = CARTESIAN_POINT ( 'NONE',  ( -156.6671849566219805, -193.5000000000000000, 60.59166255800406731 ) ) ;
#39507 = FACE_OUTER_BOUND ( 'NONE', #28585, .T. ) ;
#39508 = ORIENTED_EDGE ( 'NONE', *, *, #7612, .F. ) ;
#39509 = VECTOR ( 'NONE', #42070, 1000.000000000000000 ) ;
#39510 = PRODUCT_DEFINITION_CONTEXT ( 'detailed design', #12554, 'design' ) ;
#39511 = CARTESIAN_POINT ( 'NONE',  ( -49.03777351731250889, -183.6283474603465606, 0.8294056854502042109 ) ) ;
#39512 = AXIS2_PLACEMENT_3D ( 'NONE', #26493, #41483, #6278 ) ;
#39513 = EDGE_LOOP ( 'NONE', ( #1686, #26829, #19349, #24248 ) ) ;
#39514 = EDGE_LOOP ( 'NONE', ( #17934, #39009, #49579, #21751 ) ) ;
#39515 = ORIENTED_EDGE ( 'NONE', *, *, #9225, .T. ) ;
#39516 = DIRECTION ( 'NONE',  ( -0.000000000000000000, 1.000000000000000000, -0.000000000000000000 ) ) ;
#39517 = DIRECTION ( 'NONE',  ( -0.3482016354343866471, 0.000000000000000000, -0.9374196611341253371 ) ) ;
#39518 = VERTEX_POINT ( 'NONE', #34466 ) ;
#39519 = FACE_OUTER_BOUND ( 'NONE', #21469, .T. ) ;
#39520 = DIRECTION ( 'NONE',  ( 0.6965510290630033685, 0.000000000000000000, -0.7175072570443249420 ) ) ;
#39521 = EDGE_CURVE ( 'NONE', #41796, #24186, #11057, .T. ) ;
#39523 = ADVANCED_FACE ( 'NONE', ( #14511 ), #18704, .T. ) ;
#39522 = LINE ( 'NONE', #46928, #5000 ) ;
#39524 = ORIENTED_EDGE ( 'NONE', *, *, #46138, .F. ) ;
#39525 = CARTESIAN_POINT ( 'NONE',  ( -332.3517673607765914, -105.0395444947681369, -56.09938080879045685 ) ) ;
#39526 = ORIENTED_EDGE ( 'NONE', *, *, #41242, .T. ) ;
#39527 = DIRECTION ( 'NONE',  ( -1.000000000000000000, -0.000000000000000000, -0.000000000000000000 ) ) ;
#39528 = VECTOR ( 'NONE', #23989, 1000.000000000000000 ) ;
#39529 = PLANE ( 'NONE',  #27842 ) ;
#39530 = VERTEX_POINT ( 'NONE', #27087 ) ;
#39531 = DIRECTION ( 'NONE',  ( -0.000000000000000000, 1.000000000000000000, -0.000000000000000000 ) ) ;
#39532 = DIRECTION ( 'NONE',  ( 0.000000000000000000, 1.000000000000000000, 0.000000000000000000 ) ) ;
#39533 = DIRECTION ( 'NONE',  ( -8.718379230999707126E-17, -0.9927088740980527515, 0.1205366802553337890 ) ) ;
#39534 = FACE_OUTER_BOUND ( 'NONE', #17552, .T. ) ;
#39535 = LINE ( 'NONE', #3545, #43753 ) ;
#39536 = ORIENTED_EDGE ( 'NONE', *, *, #39397, .F. ) ;
#39537 = ORIENTED_EDGE ( 'NONE', *, *, #36896, .F. ) ;
#39538 = EDGE_CURVE ( 'NONE', #48929, #9685, #49085, .T. ) ;
#39539 = DIRECTION ( 'NONE',  ( -0.000000000000000000, 1.000000000000000000, -0.000000000000000000 ) ) ;
#39541 = ORIENTED_EDGE ( 'NONE', *, *, #42248, .F. ) ;
#39540 = CARTESIAN_POINT ( 'NONE',  ( -330.4913330509368166, -84.00150778970706256, 43.83057281297416097 ) ) ;
#39542 = VECTOR ( 'NONE', #29849, 999.9999999999998863 ) ;
#39543 = ORIENTED_EDGE ( 'NONE', *, *, #30282, .T. ) ;
#39544 = CARTESIAN_POINT ( 'NONE',  ( 52.36832552120769435, -175.3837268820161057, -72.15117186584490128 ) ) ;
#39545 = EDGE_CURVE ( 'NONE', #49872, #20460, #39562, .T. ) ;
#39546 = AXIS2_PLACEMENT_3D ( 'NONE', #44600, #8589, #24619 ) ;
#39547 = CARTESIAN_POINT ( 'NONE',  ( 67.42090074966655777, -175.3837268820161057, -46.82076062204441058 ) ) ;
#39548 = VERTEX_POINT ( 'NONE', #28830 ) ;
#39549 = FACE_BOUND ( 'NONE', #36142, .T. ) ;
#39550 = CARTESIAN_POINT ( 'NONE',  ( -330.4913330509368166, -175.9742670995611036, 26.97593913775620678 ) ) ;
#39551 = ORIENTED_EDGE ( 'NONE', *, *, #4263, .T. ) ;
#39552 = CARTESIAN_POINT ( 'NONE',  ( 49.03269102277813829, 35.00000000000000000, -50.83217377521822300 ) ) ;
#39553 = CARTESIAN_POINT ( 'NONE',  ( -365.0000000000001137, -168.5000000000000284, -5.000000000000001776 ) ) ;
#39554 = CARTESIAN_POINT ( 'NONE',  ( 43.12693905415815010, -193.5000000000000000, -83.57229767764155781 ) ) ;
#39555 = CARTESIAN_POINT ( 'NONE',  ( -70.75782287548088334, -189.7472609257535510, 122.9986166548864901 ) ) ;
#39556 = ORIENTED_EDGE ( 'NONE', *, *, #2760, .F. ) ;
#39557 = CIRCLE ( 'NONE', #9387, 124.9999999999999858 ) ;
#39558 = EDGE_LOOP ( 'NONE', ( #27614, #15888, #29614, #39501 ) ) ;
#39559 = VERTEX_POINT ( 'NONE', #738 ) ;
#39560 = DIRECTION ( 'NONE',  ( -0.000000000000000000, 1.000000000000000000, -0.000000000000000000 ) ) ;
#39561 = CARTESIAN_POINT ( 'NONE',  ( 38.48673058372652633, -189.7472609257535510, 88.39086586114804334 ) ) ;
#39562 = CIRCLE ( 'NONE', #32027, 60.00000000000000000 ) ;
#39563 = CARTESIAN_POINT ( 'NONE',  ( -170.0000000000000284, -173.5000000000000284, -60.00000000000001421 ) ) ;
#39564 = DIRECTION ( 'NONE',  ( 0.000000000000000000, -0.000000000000000000, -1.000000000000000000 ) ) ;
#39565 = CARTESIAN_POINT ( 'NONE',  ( 17.15229921100054611, -193.5000000000000000, -106.3838142112212921 ) ) ;
#39566 = VERTEX_POINT ( 'NONE', #48836 ) ;
#39567 = DIRECTION ( 'NONE',  ( 0.9890401873221644768, 0.000000000000000000, -0.1476465640024779702 ) ) ;
#39568 = VERTEX_POINT ( 'NONE', #7403 ) ;
#39570 = ORIENTED_EDGE ( 'NONE', *, *, #45282, .T. ) ;
#39569 = LINE ( 'NONE', #28775, #1296 ) ;
#39571 = ORIENTED_EDGE ( 'NONE', *, *, #48077, .F. ) ;
#39572 = DIRECTION ( 'NONE',  ( -0.000000000000000000, 1.000000000000000000, 0.000000000000000000 ) ) ;
#39573 = CARTESIAN_POINT ( 'NONE',  ( 75.32224018181403835, -177.1207230881787780, 7.024906801079477958 ) ) ;
#39574 = VECTOR ( 'NONE', #4768, 1000.000000000000000 ) ;
#39575 = CARTESIAN_POINT ( 'NONE',  ( 50.88012955800436998, -193.5000000000000000, 74.18852968774250201 ) ) ;
#39576 = EDGE_CURVE ( 'NONE', #34925, #32740, #24641, .T. ) ;
#39577 = LINE ( 'NONE', #3588, #28412 ) ;
#39578 = EDGE_LOOP ( 'NONE', ( #18501, #12284, #37942, #24040 ) ) ;
#39579 = CARTESIAN_POINT ( 'NONE',  ( -339.1964088526558498, -175.5095439275177398, -27.86139516340860212 ) ) ;
#39580 = AXIS2_PLACEMENT_3D ( 'NONE', #45122, #20665, #9112 ) ;
#39581 = ORIENTED_EDGE ( 'NONE', *, *, #24054, .T. ) ;
#39582 = AXIS2_PLACEMENT_3D ( 'NONE', #14755, #41830, #23906 ) ;
#39583 = EDGE_LOOP ( 'NONE', ( #43904, #31752, #42068, #41428 ) ) ;
#39584 = LINE ( 'NONE', #48270, #42207 ) ;
#39585 = CARTESIAN_POINT ( 'NONE',  ( -339.1964088526558498, -123.5000000000000284, 0.000000000000000000 ) ) ;
#39586 = DIRECTION ( 'NONE',  ( -1.000000000000000000, -0.000000000000000000, -0.000000000000000000 ) ) ;
#39587 = FACE_OUTER_BOUND ( 'NONE', #2137, .T. ) ;
#39588 = LINE ( 'NONE', #44585, #5402 ) ;
#39589 = CYLINDRICAL_SURFACE ( 'NONE', #46383, 125.0000000000000000 ) ;
#39590 = ORIENTED_EDGE ( 'NONE', *, *, #32052, .F. ) ;
#39591 = LINE ( 'NONE', #31461, #37229 ) ;
#39592 = FACE_OUTER_BOUND ( 'NONE', #15203, .T. ) ;
#39593 = AXIS2_PLACEMENT_3D ( 'NONE', #36063, #12659, #12402 ) ;
#39594 = CARTESIAN_POINT ( 'NONE',  ( -48.47912675150885065, -189.7472609257535510, 6.938893903907228378E-15 ) ) ;
#39595 = ORIENTED_EDGE ( 'NONE', *, *, #35602, .T. ) ;
#39596 = VECTOR ( 'NONE', #44656, 1000.000000000000000 ) ;
#39597 = VECTOR ( 'NONE', #24001, 1000.000000000000000 ) ;
#39598 = EDGE_CURVE ( 'NONE', #40102, #13896, #16515, .T. ) ;
#39599 = CARTESIAN_POINT ( 'NONE',  ( -339.1964088526558498, -79.00630452878414189, 38.74998146212082162 ) ) ;
#39600 = DIRECTION ( 'NONE',  ( -0.3482016354343928088, 0.000000000000000000, -0.9374196611341231167 ) ) ;
#39601 = VERTEX_POINT ( 'NONE', #40653 ) ;
#39602 = FACE_OUTER_BOUND ( 'NONE', #37009, .T. ) ;
#39603 = ORIENTED_EDGE ( 'NONE', *, *, #20750, .T. ) ;
#39604 = DIRECTION ( 'NONE',  ( 0.000000000000000000, 0.000000000000000000, 1.000000000000000000 ) ) ;
#39605 = FACE_BOUND ( 'NONE', #5126, .T. ) ;
#39607 = VERTEX_POINT ( 'NONE', #17293 ) ;
#39606 = CARTESIAN_POINT ( 'NONE',  ( -336.3521761649654422, -133.2247606357419443, -58.25253621232173629 ) ) ;
#39608 = AXIS2_PLACEMENT_3D ( 'NONE', #34932, #23123, #14992 ) ;
#39609 = CARTESIAN_POINT ( 'NONE',  ( -88.78924379339714790, -177.1207230881787780, -118.3219948448692520 ) ) ;
#39610 = ORIENTED_EDGE ( 'NONE', *, *, #13065, .T. ) ;
#39611 = VECTOR ( 'NONE', #35473, 1000.000000000000000 ) ;
#39612 = EDGE_LOOP ( 'NONE', ( #25507, #25339, #25685, #31820 ) ) ;
#39613 = CARTESIAN_POINT ( 'NONE',  ( -336.3521761649654422, -140.1754235130667610, -56.65561927338005432 ) ) ;
#39614 = ORIENTED_EDGE ( 'NONE', *, *, #17776, .T. ) ;
#39615 = PLANE ( 'NONE',  #34300 ) ;
#39616 = DIRECTION ( 'NONE',  ( -0.4031234292879600778, 0.000000000000000000, -0.9151456172430237901 ) ) ;
#39617 = EDGE_CURVE ( 'NONE', #37719, #3202, #8545, .T. ) ;
#39618 = VECTOR ( 'NONE', #17672, 1000.000000000000000 ) ;
#39619 = VECTOR ( 'NONE', #48980, 1000.000000000000000 ) ;
#39620 = ADVANCED_FACE ( 'NONE', ( #12807 ), #1239, .T. ) ;
#39621 = CARTESIAN_POINT ( 'NONE',  ( -162.4844509910036265, -183.6283474603465606, -48.77484799213895172 ) ) ;
#39622 = ORIENTED_EDGE ( 'NONE', *, *, #15048, .F. ) ;
#39625 = VERTEX_POINT ( 'NONE', #8874 ) ;
#39624 = DIRECTION ( 'NONE',  ( 0.000000000000000000, 0.000000000000000000, 1.000000000000000000 ) ) ;
#39623 = CARTESIAN_POINT ( 'NONE',  ( -336.3521761649654422, -64.50000000000000000, -2.632288850093980503 ) ) ;
#39626 = VECTOR ( 'NONE', #9049, 1000.000000000000000 ) ;
#39627 = ORIENTED_EDGE ( 'NONE', *, *, #31710, .F. ) ;
#39628 = DIRECTION ( 'NONE',  ( -0.000000000000000000, 0.7485107481710934207, -0.6631226582408039638 ) ) ;
#39629 = VERTEX_POINT ( 'NONE', #13347 ) ;
#39630 = CARTESIAN_POINT ( 'NONE',  ( 75.27070168362158142, -175.3837268820161057, 17.63462396184792524 ) ) ;
#39631 = ORIENTED_EDGE ( 'NONE', *, *, #32240, .T. ) ;
#39632 = EDGE_CURVE ( 'NONE', #29000, #14596, #33315, .T. ) ;
#39633 = CARTESIAN_POINT ( 'NONE',  ( -339.1964088526558498, -115.8919814278862503, 58.50955523165745831 ) ) ;
#39634 = VERTEX_POINT ( 'NONE', #3434 ) ;
#39636 = CARTESIAN_POINT ( 'NONE',  ( -169.9131040279660283, -193.5000000000000000, 29.64437826672835996 ) ) ;
#39635 = DIRECTION ( 'NONE',  ( 0.000000000000000000, 0.000000000000000000, 1.000000000000000000 ) ) ;
#39637 = VERTEX_POINT ( 'NONE', #40930 ) ;
#39638 = ADVANCED_FACE ( 'NONE', ( #24387 ), #41185, .T. ) ;
#39639 = DIRECTION ( 'NONE',  ( 0.000000000000000000, 0.000000000000000000, 1.000000000000000000 ) ) ;
#39640 = VERTEX_POINT ( 'NONE', #45164 ) ;
#39641 = CARTESIAN_POINT ( 'NONE',  ( -47.47956591500005885, -183.6283474603465606, 0.02963332782257025594 ) ) ;
#39642 = EDGE_CURVE ( 'NONE', #34518, #16239, #5209, .T. ) ;
#39643 = DIRECTION ( 'NONE',  ( 0.000000000000000000, 1.000000000000000000, 0.000000000000000000 ) ) ;
#39644 = DIRECTION ( 'NONE',  ( -0.8455960035018199594, 0.000000000000000000, -0.5338233779648003940 ) ) ;
#39645 = CARTESIAN_POINT ( 'NONE',  ( -330.4913330509368166, -151.8251501453686956, -52.89315522109000511 ) ) ;
#39646 = DIRECTION ( 'NONE',  ( 0.000000000000000000, 1.000000000000000000, 0.000000000000000000 ) ) ;
#39647 = VECTOR ( 'NONE', #29580, 1000.000000000000000 ) ;
#39648 = FACE_OUTER_BOUND ( 'NONE', #48197, .T. ) ;
#39649 = EDGE_LOOP ( 'NONE', ( #36159, #32542, #11185, #30089 ) ) ;
#39650 = CARTESIAN_POINT ( 'NONE',  ( -336.3521761649654422, -182.2665742509934148, -5.491276508484069119 ) ) ;
#39651 = DIRECTION ( 'NONE',  ( 0.000000000000000000, 0.000000000000000000, -1.000000000000000000 ) ) ;
#39652 = AXIS2_PLACEMENT_3D ( 'NONE', #2912, #34967, #51031 ) ;
#39653 = PLANE ( 'NONE',  #28785 ) ;
#39654 = ORIENTED_EDGE ( 'NONE', *, *, #402, .T. ) ;
#39655 = LINE ( 'NONE', #23896, #3882 ) ;
#39656 = ADVANCED_FACE ( 'NONE', ( #17039 ), #20438, .F. ) ;
#39657 = DIRECTION ( 'NONE',  ( 0.000000000000000000, -1.000000000000000000, 0.000000000000000000 ) ) ;
#39659 = ORIENTED_EDGE ( 'NONE', *, *, #34013, .F. ) ;
#39658 = CARTESIAN_POINT ( 'NONE',  ( 46.00000000000000711, 20.00000000000000000, 41.00000000000000000 ) ) ;
#39660 = ORIENTED_EDGE ( 'NONE', *, *, #48027, .F. ) ;
#39661 = AXIS2_PLACEMENT_3D ( 'NONE', #31264, #27059, #47057 ) ;
#39662 = EDGE_LOOP ( 'NONE', ( #17145, #47481, #43763, #37234 ) ) ;
#39663 = AXIS2_PLACEMENT_3D ( 'NONE', #48294, #39862, #24378 ) ;
#39664 = AXIS2_PLACEMENT_3D ( 'NONE', #19972, #24684, #7874 ) ;
#39665 = CARTESIAN_POINT ( 'NONE',  ( 72.05536924052414349, -193.5000000000000000, 33.11246405730899056 ) ) ;
#39666 = VECTOR ( 'NONE', #45368, 1000.000000000000000 ) ;
#39667 = LINE ( 'NONE', #35739, #21143 ) ;
#39668 = DIRECTION ( 'NONE',  ( 0.5085311186492094127, 0.000000000000000000, 0.8610436117673619938 ) ) ;
#39669 = LINE ( 'NONE', #2913, #40456 ) ;
#39670 = ORIENTED_EDGE ( 'NONE', *, *, #38113, .T. ) ;
#39671 = CARTESIAN_POINT ( 'NONE',  ( 4.460702607355470306, 53.89045795899486535, -18.69908610442183772 ) ) ;
#39672 = ORIENTED_EDGE ( 'NONE', *, *, #46870, .T. ) ;
#39673 = ORIENTED_EDGE ( 'NONE', *, *, #38110, .F. ) ;
#39674 = VERTEX_POINT ( 'NONE', #8606 ) ;
#39675 = CARTESIAN_POINT ( 'NONE',  ( -133.0671220150036334, -193.5000000000000000, -92.03190238880748097 ) ) ;
#39676 = CIRCLE ( 'NONE', #18742, 60.00000000000000000 ) ;
#39677 = EDGE_CURVE ( 'NONE', #26704, #23694, #3523, .T. ) ;
#39678 = EDGE_CURVE ( 'NONE', #34018, #3155, #44618, .T. ) ;
#39679 = VERTEX_POINT ( 'NONE', #4953 ) ;
#39680 = VECTOR ( 'NONE', #22959, 1000.000000000000000 ) ;
#39681 = CARTESIAN_POINT ( 'NONE',  ( -336.3521761649654422, -163.8460225846223466, -43.07972642080364523 ) ) ;
#39682 = CYLINDRICAL_SURFACE ( 'NONE', #41999, 125.0000000000000000 ) ;
#39685 = ORIENTED_EDGE ( 'NONE', *, *, #23595, .F. ) ;
#39684 = LINE ( 'NONE', #6637, #37543 ) ;
#39683 = PLANE ( 'NONE',  #15774 ) ;
#39686 = CARTESIAN_POINT ( 'NONE',  ( -330.4913330509368166, -157.4273119900852578, -48.27201571436002325 ) ) ;
#39687 = VERTEX_POINT ( 'NONE', #20973 ) ;
#39688 = FACE_OUTER_BOUND ( 'NONE', #21080, .T. ) ;
#39689 = EDGE_LOOP ( 'NONE', ( #37841, #10516, #20216, #29706 ) ) ;
#39690 = FACE_OUTER_BOUND ( 'NONE', #372, .T. ) ;
#39691 = EDGE_CURVE ( 'NONE', #18519, #11626, #458, .T. ) ;
#39692 = DIRECTION ( 'NONE',  ( -0.9473263538541946138, 0.000000000000000000, 0.3202698538628279690 ) ) ;
#39694 = DIRECTION ( 'NONE',  ( 0.000000000000000000, 0.000000000000000000, 1.000000000000000000 ) ) ;
#39693 = DIRECTION ( 'NONE',  ( -0.000000000000000000, 0.8229838658936634577, 0.5680647467311457088 ) ) ;
#39695 = VECTOR ( 'NONE', #49466, 1000.000000000000000 ) ;
#39696 = VERTEX_POINT ( 'NONE', #35487 ) ;
#39697 = ADVANCED_FACE ( 'NONE', ( #31551 ), #47607, .F. ) ;
#39698 = FACE_OUTER_BOUND ( 'NONE', #41346, .T. ) ;
#39699 = CIRCLE ( 'NONE', #16212, 125.0000000000000000 ) ;
#39700 = FACE_OUTER_BOUND ( 'NONE', #33596, .T. ) ;
#39701 = EDGE_CURVE ( 'NONE', #22526, #42721, #35406, .T. ) ;
#39702 = ORIENTED_EDGE ( 'NONE', *, *, #28713, .T. ) ;
#39703 = DIRECTION ( 'NONE',  ( -0.000000000000000000, 1.000000000000000000, -0.000000000000000000 ) ) ;
#39704 = DIRECTION ( 'NONE',  ( -1.000000000000000000, 0.000000000000000000, -0.000000000000000000 ) ) ;
#39705 = CARTESIAN_POINT ( 'NONE',  ( -162.9896759831412965, -183.6283474603465606, -50.12318939043964861 ) ) ;
#39706 = EDGE_CURVE ( 'NONE', #31601, #4103, #34088, .T. ) ;
#39707 = ORIENTED_EDGE ( 'NONE', *, *, #34076, .F. ) ;
#39708 = DIRECTION ( 'NONE',  ( 0.000000000000000000, 1.000000000000000000, 0.000000000000000000 ) ) ;
#39709 = AXIS2_PLACEMENT_3D ( 'NONE', #2275, #47199, #42196 ) ;
#39710 = CARTESIAN_POINT ( 'NONE',  ( -172.9089226952081617, -193.5000000000000000, 11.92584929509620117 ) ) ;
#39711 = ORIENTED_EDGE ( 'NONE', *, *, #28073, .F. ) ;
#39712 = DIRECTION ( 'NONE',  ( 0.000000000000000000, 0.000000000000000000, -1.000000000000000000 ) ) ;
#39713 = EDGE_LOOP ( 'NONE', ( #32553, #28096, #10363, #29440 ) ) ;
#39714 = CARTESIAN_POINT ( 'NONE',  ( -7.223120065443619175, -183.6283474603465606, 117.9955164924470523 ) ) ;
#39715 = CARTESIAN_POINT ( 'NONE',  ( -330.4913330509368166, -71.02573290043878274, -26.97593913775585150 ) ) ;
#39716 = AXIS2_PLACEMENT_3D ( 'NONE', #3940, #23634, #12056 ) ;
#39717 = CARTESIAN_POINT ( 'NONE',  ( -159.8192355313504152, -183.6283474603465606, -56.81883646197837834 ) ) ;
#39718 = DIRECTION ( 'NONE',  ( 0.000000000000000000, 1.000000000000000000, 0.000000000000000000 ) ) ;
#39719 = DIRECTION ( 'NONE',  ( -0.000000000000000000, -0.9709418174260502354, 0.2393156642875652051 ) ) ;
#39720 = AXIS2_PLACEMENT_3D ( 'NONE', #45973, #25975, #22030 ) ;
#39721 = DIRECTION ( 'NONE',  ( -0.9960498426152158968, 0.000000000000000000, -0.08879589532294571153 ) ) ;
#39722 = DIRECTION ( 'NONE',  ( -0.000000000000000000, 1.000000000000000000, -0.000000000000000000 ) ) ;
#39723 = DIRECTION ( 'NONE',  ( 0.000000000000000000, 0.000000000000000000, -1.000000000000000000 ) ) ;
#39725 = EDGE_LOOP ( 'NONE', ( #1928, #36256, #30037, #919 ) ) ;
#39724 = DIRECTION ( 'NONE',  ( -0.000000000000000000, 1.000000000000000000, -0.000000000000000000 ) ) ;
#39726 = ORIENTED_EDGE ( 'NONE', *, *, #13522, .F. ) ;
#39727 = DIRECTION ( 'NONE',  ( 0.2348860457809775482, 0.000000000000000000, 0.9720229140804121926 ) ) ;
#39728 = AXIS2_PLACEMENT_3D ( 'NONE', #3450, #43661, #23679 ) ;
#39729 = EDGE_CURVE ( 'NONE', #5479, #42477, #17561, .T. ) ;
#39730 = PLANE ( 'NONE',  #27961 ) ;
#39731 = EDGE_LOOP ( 'NONE', ( #4282, #21788, #18795, #18834 ) ) ;
#39732 = ORIENTED_EDGE ( 'NONE', *, *, #40435, .T. ) ;
#39733 = DIRECTION ( 'NONE',  ( -0.9266896074318291543, 0.000000000000000000, -0.3758275821142488260 ) ) ;
#39734 = ORIENTED_EDGE ( 'NONE', *, *, #51954, .F. ) ;
#39735 = FACE_OUTER_BOUND ( 'NONE', #47391, .T. ) ;
#39736 = FACE_OUTER_BOUND ( 'NONE', #16699, .T. ) ;
#39737 = EDGE_CURVE ( 'NONE', #2241, #33953, #49609, .T. ) ;
#39738 = EDGE_CURVE ( 'NONE', #51208, #22860, #37510, .T. ) ;
#39739 = EDGE_CURVE ( 'NONE', #6533, #46287, #49865, .T. ) ;
#39740 = DIRECTION ( 'NONE',  ( 0.000000000000000000, -0.000000000000000000, -1.000000000000000000 ) ) ;
#39741 = DIRECTION ( 'NONE',  ( -1.000000000000000000, 0.000000000000000000, 0.000000000000000000 ) ) ;
#39742 = VERTEX_POINT ( 'NONE', #37767 ) ;
#39743 = EDGE_LOOP ( 'NONE', ( #51533, #29256, #46803, #28329 ) ) ;
#39744 = ADVANCED_FACE ( 'NONE', ( #50138 ), #6235, .T. ) ;
#39745 = ORIENTED_EDGE ( 'NONE', *, *, #42340, .T. ) ;
#39746 = DIRECTION ( 'NONE',  ( -0.000000000000000000, 1.000000000000000000, -0.000000000000000000 ) ) ;
#39747 = DIRECTION ( 'NONE',  ( -0.000000000000000000, 0.9350162426854158326, 0.3546048870425331789 ) ) ;
#39748 = CARTESIAN_POINT ( 'NONE',  ( -336.3521761649654422, -123.5000000000000284, 0.000000000000000000 ) ) ;
#39749 = EDGE_CURVE ( 'NONE', #11792, #6023, #47986, .T. ) ;
#39750 = DIRECTION ( 'NONE',  ( 0.000000000000000000, 0.000000000000000000, -1.000000000000000000 ) ) ;
#39751 = CARTESIAN_POINT ( 'NONE',  ( -330.4913330509368166, -75.22798428563987727, -33.92731199008506593 ) ) ;
#39752 = CIRCLE ( 'NONE', #5357, 60.00000000000000000 ) ;
#39753 = ORIENTED_EDGE ( 'NONE', *, *, #3196, .T. ) ;
#39754 = LINE ( 'NONE', #340, #2856 ) ;
#39755 = EDGE_CURVE ( 'NONE', #15605, #24889, #26139, .T. ) ;
#39756 = CARTESIAN_POINT ( 'NONE',  ( -30.00000000000000000, 0.000000000000000000, 30.00000000000000355 ) ) ;
#39757 = PLANE ( 'NONE',  #27403 ) ;
#39758 = VECTOR ( 'NONE', #5435, 1000.000000000000000 ) ;
#39759 = EDGE_CURVE ( 'NONE', #22186, #16764, #43774, .T. ) ;
#39760 = ORIENTED_EDGE ( 'NONE', *, *, #13800, .F. ) ;
#39761 = ORIENTED_EDGE ( 'NONE', *, *, #1897, .F. ) ;
#39762 = ORIENTED_EDGE ( 'NONE', *, *, #42745, .T. ) ;
#39763 = CARTESIAN_POINT ( 'NONE',  ( -89.44307666693794090, -183.6283474603465606, -117.0391155081702266 ) ) ;
#39764 = EDGE_CURVE ( 'NONE', #51485, #51398, #41445, .T. ) ;
#39765 = CARTESIAN_POINT ( 'NONE',  ( -339.1964088526558498, -66.33409060400673241, -14.60509510167901404 ) ) ;
#39766 = VERTEX_POINT ( 'NONE', #1513 ) ;
#39767 = CARTESIAN_POINT ( 'NONE',  ( -336.3521761649654422, -174.5186198893880771, 29.74944317415823392 ) ) ;
#39768 = EDGE_CURVE ( 'NONE', #47058, #7135, #22252, .T. ) ;
#39769 = CARTESIAN_POINT ( 'NONE',  ( -73.70588833648351113, -177.1207230881787780, 121.4073237908568359 ) ) ;
#39770 = DIRECTION ( 'NONE',  ( 0.9374196611341231167, 0.000000000000000000, -0.3482016354343928088 ) ) ;
#39771 = ORIENTED_EDGE ( 'NONE', *, *, #35249, .F. ) ;
#39772 = PLANE ( 'NONE',  #45233 ) ;
#39773 = AXIS2_PLACEMENT_3D ( 'NONE', #9402, #25429, #16785 ) ;
#39774 = EDGE_CURVE ( 'NONE', #50591, #29857, #30145, .T. ) ;
#39775 = EDGE_CURVE ( 'NONE', #29802, #29776, #25428, .T. ) ;
#39776 = VERTEX_POINT ( 'NONE', #18332 ) ;
#39777 = LINE ( 'NONE', #12182, #38324 ) ;
#39778 = CARTESIAN_POINT ( 'NONE',  ( -56.71246971489870958, -193.5000000000000000, -124.7285535218267682 ) ) ;
#39779 = CARTESIAN_POINT ( 'NONE',  ( -48.47912675150885065, -189.7472609257535510, 6.938893903907228378E-15 ) ) ;
#39780 = VERTEX_POINT ( 'NONE', #17802 ) ;
#39781 = CARTESIAN_POINT ( 'NONE',  ( 74.80070215680143519, -177.1207230881787780, 13.35228579481199596 ) ) ;
#39782 = CARTESIAN_POINT ( 'NONE',  ( 34.93559171950835918, -183.6283474603465606, -93.09664195018497423 ) ) ;
#39783 = CARTESIAN_POINT ( 'NONE',  ( -71.22983192549011733, -175.3837268820161057, -121.8950816227732759 ) ) ;
#39784 = CARTESIAN_POINT ( 'NONE',  ( 32.49319223169170812, -189.7472609257535510, -95.22858582633060109 ) ) ;
#39785 = EDGE_CURVE ( 'NONE', #15240, #50991, #41964, .T. ) ;
#39786 = ORIENTED_EDGE ( 'NONE', *, *, #30191, .F. ) ;
#39787 = CARTESIAN_POINT ( 'NONE',  ( -169.6719064342497632, -177.1207230881787780, 30.61552143554992256 ) ) ;
#39788 = ORIENTED_EDGE ( 'NONE', *, *, #73, .F. ) ;
#39789 = VERTEX_POINT ( 'NONE', #38278 ) ;
#39790 = CARTESIAN_POINT ( 'NONE',  ( 24.88090138098524307, -193.5000000000000000, 99.97252634603304955 ) ) ;
#39792 = EDGE_LOOP ( 'NONE', ( #22512, #5876, #36622, #39825 ) ) ;
#39791 = DIRECTION ( 'NONE',  ( 0.000000000000000000, 0.000000000000000000, 1.000000000000000000 ) ) ;
#39793 = CIRCLE ( 'NONE', #28022, 125.0000000000000000 ) ;
#39794 = VECTOR ( 'NONE', #42304, 1000.000000000000000 ) ;
#39795 = VERTEX_POINT ( 'NONE', #2020 ) ;
#39796 = CARTESIAN_POINT ( 'NONE',  ( -336.3521761649654422, -106.8245764869328980, 56.65561927337994064 ) ) ;
#39797 = AXIS2_PLACEMENT_3D ( 'NONE', #5114, #33490, #37151 ) ;
#39798 = CARTESIAN_POINT ( 'NONE',  ( -332.3517673607765914, -65.12692710742291524, -8.732051761643681687 ) ) ;
#39799 = EDGE_LOOP ( 'NONE', ( #43549, #50096, #744, #36247 ) ) ;
#39800 = DIRECTION ( 'NONE',  ( -0.000000000000000000, 1.000000000000000000, -0.000000000000000000 ) ) ;
#39801 = CARTESIAN_POINT ( 'NONE',  ( -49.42645310536304493, -193.5000000000000000, 0.3202698538628349079 ) ) ;
#39802 = EDGE_LOOP ( 'NONE', ( #13576, #34293, #25281, #32629 ) ) ;
#39803 = DIRECTION ( 'NONE',  ( -0.000000000000000000, 1.000000000000000000, -0.000000000000000000 ) ) ;
#39804 = CARTESIAN_POINT ( 'NONE',  ( -117.8923552450419265, -189.7472609257535510, 102.7511748916629131 ) ) ;
#39805 = EDGE_CURVE ( 'NONE', #47094, #4101, #2298, .T. ) ;
#39806 = EDGE_CURVE ( 'NONE', #10115, #50532, #46189, .T. ) ;
#39808 = AXIS2_PLACEMENT_3D ( 'NONE', #148, #4356, #40094 ) ;
#39807 = LINE ( 'NONE', #28760, #47092 ) ;
#39809 = CARTESIAN_POINT ( 'NONE',  ( -47.57632892154310866, -193.5000000000000000, -0.4300652022765113491 ) ) ;
#39810 = ORIENTED_EDGE ( 'NONE', *, *, #38553, .T. ) ;
#39811 = VERTEX_POINT ( 'NONE', #50388 ) ;
#39812 = EDGE_CURVE ( 'NONE', #42957, #13339, #14376, .T. ) ;
#39813 = ORIENTED_EDGE ( 'NONE', *, *, #25321, .T. ) ;
#39814 = EDGE_CURVE ( 'NONE', #840, #22277, #34541, .T. ) ;
#39815 = DIRECTION ( 'NONE',  ( 0.5085311186492216251, 0.000000000000000000, -0.8610436117673548884 ) ) ;
#39816 = CARTESIAN_POINT ( 'NONE',  ( -106.2948367055609964, -175.3837268820161057, -110.8257356506552327 ) ) ;
#39817 = DIRECTION ( 'NONE',  ( 0.5586467658036415873, 0.000000000000000000, 0.8294056854502090959 ) ) ;
#39818 = CARTESIAN_POINT ( 'NONE',  ( 51.70113075622899856, 35.00000000000000000, -45.78969942005421956 ) ) ;
#39819 = CARTESIAN_POINT ( 'NONE',  ( -332.3517673607765914, -77.52356969168074841, 38.55084767037245541 ) ) ;
#39820 = ORIENTED_EDGE ( 'NONE', *, *, #17657, .T. ) ;
#39821 = CARTESIAN_POINT ( 'NONE',  ( -336.3521761649654422, -179.2447759217480154, -19.39547174791710660 ) ) ;
#39822 = ORIENTED_EDGE ( 'NONE', *, *, #46741, .T. ) ;
#39824 = EDGE_LOOP ( 'NONE', ( #51924, #9351, #14135, #44642 ) ) ;
#39823 = CARTESIAN_POINT ( 'NONE',  ( -336.3521761649654422, -83.15397741537739762, 43.07972642080338233 ) ) ;
#39825 = ORIENTED_EDGE ( 'NONE', *, *, #44293, .T. ) ;
#39826 = VECTOR ( 'NONE', #30669, 1000.000000000000000 ) ;
#39827 = EDGE_CURVE ( 'NONE', #24601, #10174, #23808, .T. ) ;
#39828 = DIRECTION ( 'NONE',  ( 0.4827922027307366970, 0.000000000000000000, 0.8757349421956412971 ) ) ;
#39829 = PLANE ( 'NONE',  #12354 ) ;
#39830 = AXIS2_PLACEMENT_3D ( 'NONE', #28393, #44442, #8428 ) ;
#39831 = CIRCLE ( 'NONE', #17207, 125.0000000000000000 ) ;
#39832 = CARTESIAN_POINT ( 'NONE',  ( 67.87295084395104539, -183.6283474603465606, 42.87565520599286373 ) ) ;
#39833 = LINE ( 'NONE', #27509, #20055 ) ;
#39834 = VERTEX_POINT ( 'NONE', #26717 ) ;
#39835 = DIRECTION ( 'NONE',  ( -0.2920567706369833760, 0.000000000000000000, 0.9564009842765202052 ) ) ;
#39836 = ORIENTED_EDGE ( 'NONE', *, *, #37635, .T. ) ;
#39837 = VECTOR ( 'NONE', #51852, 1000.000000000000000 ) ;
#39838 = ADVANCED_FACE ( 'NONE', ( #14911 ), #7531, .T. ) ;
#39839 = EDGE_LOOP ( 'NONE', ( #36754, #46681, #14182, #17086 ) ) ;
#39840 = LINE ( 'NONE', #4376, #11971 ) ;
#39841 = COLOUR_RGB ( '', 0.31764706, 0.68627451, 0.89019608) ;
#39842 = CARTESIAN_POINT ( 'NONE',  ( -339.1964088526558498, -131.1080185721124849, 58.50955523165764305 ) ) ;
#39843 = CARTESIAN_POINT ( 'NONE',  ( -339.1964088526558498, -138.1050951016783301, 57.16590939599346655 ) ) ;
#39844 = CIRCLE ( 'NONE', #21411, 125.0000000000000000 ) ;
#39845 = LINE ( 'NONE', #169, #45757 ) ;
#39846 = CARTESIAN_POINT ( 'NONE',  ( -47.70260288879080690, -175.3837268820161057, -0.6300878435817026668 ) ) ;
#39847 = DIRECTION ( 'NONE',  ( 0.000000000000000000, 0.000000000000000000, 1.000000000000000000 ) ) ;
#39848 = ORIENTED_EDGE ( 'NONE', *, *, #46249, .F. ) ;
#39849 = AXIS2_PLACEMENT_3D ( 'NONE', #15879, #31112, #27940 ) ;
#39850 = CARTESIAN_POINT ( 'NONE',  ( -81.70897914701313880, -177.1207230881787780, -120.5021863277716534 ) ) ;
#39851 = DIRECTION ( 'NONE',  ( -0.000000000000000000, 1.000000000000000000, -0.000000000000000000 ) ) ;
#39852 = FACE_BOUND ( 'NONE', #4492, .T. ) ;
#39853 = VERTEX_POINT ( 'NONE', #31429 ) ;
#39854 = CARTESIAN_POINT ( 'NONE',  ( -332.3517673607765914, -160.6539403396202772, 45.90766452162722544 ) ) ;
#39855 = DIRECTION ( 'NONE',  ( -0.000000000000000000, 1.000000000000000000, -0.000000000000000000 ) ) ;
#39856 = ORIENTED_EDGE ( 'NONE', *, *, #46560, .T. ) ;
#39857 = DIRECTION ( 'NONE',  ( 0.5451229641719399499, -0.8383561021024406035, 0.000000000000000000 ) ) ;
#39858 = VERTEX_POINT ( 'NONE', #39818 ) ;
#39859 = PLANE ( 'NONE',  #36019 ) ;
#39860 = VECTOR ( 'NONE', #36562, 1000.000000000000114 ) ;
#39861 = FACE_BOUND ( 'NONE', #52025, .T. ) ;
#39863 = EDGE_LOOP ( 'NONE', ( #44963, #28720, #24587, #16005 ) ) ;
#39862 = DIRECTION ( 'NONE',  ( 0.000000000000000000, -1.000000000000000000, 0.000000000000000000 ) ) ;
#39864 = VECTOR ( 'NONE', #31637, 1000.000000000000227 ) ;
#39865 = AXIS2_PLACEMENT_3D ( 'NONE', #10853, #51322, #7439 ) ;
#39866 = EDGE_CURVE ( 'NONE', #14596, #15649, #39047, .T. ) ;
#39867 = LINE ( 'NONE', #11763, #47882 ) ;
#39868 = EDGE_LOOP ( 'NONE', ( #21713, #43133, #8405, #22246 ) ) ;
#39869 = AXIS2_PLACEMENT_3D ( 'NONE', #13320, #21464, #35346 ) ;
#39870 = ORIENTED_EDGE ( 'NONE', *, *, #5158, .T. ) ;
#39871 = LINE ( 'NONE', #48302, #30930 ) ;
#39872 = ORIENTED_EDGE ( 'NONE', *, *, #9348, .T. ) ;
#39873 = CIRCLE ( 'NONE', #17254, 125.0000000000000000 ) ;
#39874 = CARTESIAN_POINT ( 'NONE',  ( -171.7300019102062549, -183.6283474603465606, -20.83798868929510562 ) ) ;
#39875 = AXIS2_PLACEMENT_3D ( 'NONE', #46496, #30705, #49921 ) ;
#39876 = CARTESIAN_POINT ( 'NONE',  ( -65.65563056894596627, -193.5000000000000000, 123.8142468240612999 ) ) ;
#39877 = AXIS2_PLACEMENT_3D ( 'NONE', #4755, #48907, #16315 ) ;
#39878 = VECTOR ( 'NONE', #42698, 1000.000000000000000 ) ;
#39879 = LINE ( 'NONE', #44100, #4937 ) ;
#39880 = LINE ( 'NONE', #43834, #40721 ) ;
#39881 = ORIENTED_EDGE ( 'NONE', *, *, #21697, .F. ) ;
#39884 = ORIENTED_EDGE ( 'NONE', *, *, #25945, .T. ) ;
#39883 = CYLINDRICAL_SURFACE ( 'NONE', #42371, 125.0000000000000000 ) ;
#39882 = DIRECTION ( 'NONE',  ( 0.000000000000000000, 0.000000000000000000, -1.000000000000000000 ) ) ;
#39885 = VERTEX_POINT ( 'NONE', #23550 ) ;
#39886 = EDGE_CURVE ( 'NONE', #46591, #26732, #3844, .T. ) ;
#39887 = CARTESIAN_POINT ( 'NONE',  ( -172.5669052183642123, -183.6283474603465606, 15.07392567185546994 ) ) ;
#39888 = ORIENTED_EDGE ( 'NONE', *, *, #11162, .T. ) ;
#39889 = DIRECTION ( 'NONE',  ( -0.7175072570443299380, 0.000000000000000000, -0.6965510290629983725 ) ) ;
#39890 = VERTEX_POINT ( 'NONE', #31695 ) ;
#39891 = DIRECTION ( 'NONE',  ( 0.000000000000000000, 0.000000000000000000, 1.000000000000000000 ) ) ;
#39892 = EDGE_LOOP ( 'NONE', ( #20830, #15590, #4598, #35242 ) ) ;
#39894 = DIRECTION ( 'NONE',  ( -0.000000000000000000, 1.000000000000000000, 0.000000000000000000 ) ) ;
#39893 = CYLINDRICAL_SURFACE ( 'NONE', #42571, 15.00000000000000000 ) ;
#39895 = ORIENTED_EDGE ( 'NONE', *, *, #33007, .F. ) ;
#39896 = ADVANCED_FACE ( 'NONE', ( #6759 ), #11720, .T. ) ;
#39897 = CARTESIAN_POINT ( 'NONE',  ( 26.52087324849106054, -173.5000000000000284, -70.00000000000002842 ) ) ;
#39898 = ORIENTED_EDGE ( 'NONE', *, *, #32946, .T. ) ;
#39899 = CARTESIAN_POINT ( 'NONE',  ( -49.38192458147459263, -193.5000000000000000, -0.4300652022765235616 ) ) ;
#39900 = VECTOR ( 'NONE', #47833, 1000.000000000000000 ) ;
#39901 = FACE_OUTER_BOUND ( 'NONE', #42388, .T. ) ;
#39902 = CARTESIAN_POINT ( 'NONE',  ( 46.01898237923986557, -193.5000000000000000, -81.82363577055902226 ) ) ;
#39903 = CARTESIAN_POINT ( 'NONE',  ( -339.1964088526558498, -71.02573290043838483, 26.97593913775504504 ) ) ;
#39904 = CARTESIAN_POINT ( 'NONE',  ( -101.0675409952200283, -183.6283474603465606, 113.3995532942340958 ) ) ;
#39905 = VECTOR ( 'NONE', #45043, 1000.000000000000000 ) ;
#39906 = FACE_OUTER_BOUND ( 'NONE', #24161, .T. ) ;
#39907 = AXIS2_PLACEMENT_3D ( 'NONE', #32105, #48149, #12122 ) ;
#39908 = ORIENTED_EDGE ( 'NONE', *, *, #20800, .T. ) ;
#39909 = EDGE_CURVE ( 'NONE', #8157, #46358, #4353, .T. ) ;
#39910 = PLANE ( 'NONE',  #39716 ) ;
#39911 = LINE ( 'NONE', #28085, #36576 ) ;
#39912 = CARTESIAN_POINT ( 'NONE',  ( 19.33815737959698566, -177.1207230881787780, 105.0038855142078233 ) ) ;
#39913 = EDGE_LOOP ( 'NONE', ( #44253, #45811, #43740, #42932 ) ) ;
#39914 = CARTESIAN_POINT ( 'NONE',  ( -336.3521761649654422, -181.1761995186066088, -12.53476669029101842 ) ) ;
#39915 = AXIS2_PLACEMENT_3D ( 'NONE', #46141, #19481, #3710 ) ;
#39916 = CIRCLE ( 'NONE', #20654, 60.00000000000000000 ) ;
#39917 = CARTESIAN_POINT ( 'NONE',  ( -172.6359455740846158, -183.6283474603465606, -14.49428645563797069 ) ) ;
#39918 = CARTESIAN_POINT ( 'NONE',  ( -30.00000000000000000, -43.50000000000000000, 30.00000000000000355 ) ) ;
#39919 = VERTEX_POINT ( 'NONE', #35899 ) ;
#39920 = VERTEX_POINT ( 'NONE', #46967 ) ;
#39921 = AXIS2_PLACEMENT_3D ( 'NONE', #17392, #8699, #40745 ) ;
#39922 = ORIENTED_EDGE ( 'NONE', *, *, #47437, .F. ) ;
#39923 = ADVANCED_FACE ( 'NONE', ( #51427 ), #51950, .T. ) ;
#39924 = CIRCLE ( 'NONE', #5569, 125.0000000000000000 ) ;
#39925 = FACE_OUTER_BOUND ( 'NONE', #31583, .T. ) ;
#39926 = DIRECTION ( 'NONE',  ( 0.8896570909947499883, 0.000000000000000000, -0.4566292373937077542 ) ) ;
#39927 = DIRECTION ( 'NONE',  ( -0.8610436117673621048, 0.000000000000000000, 0.5085311186492095237 ) ) ;
#39928 = CARTESIAN_POINT ( 'NONE',  ( -60.00000000000000000, -63.50000000000000000, 0.000000000000000000 ) ) ;
#39929 = ORIENTED_EDGE ( 'NONE', *, *, #42856, .F. ) ;
#39930 = EDGE_CURVE ( 'NONE', #40473, #3020, #46700, .T. ) ;
#39931 = CARTESIAN_POINT ( 'NONE',  ( 1.165667945738152245, 58.00551856110927673, -16.50937507019845540 ) ) ;
#39932 = ORIENTED_EDGE ( 'NONE', *, *, #49473, .F. ) ;
#39933 = ORIENTED_EDGE ( 'NONE', *, *, #27910, .T. ) ;
#39934 = EDGE_CURVE ( 'NONE', #31030, #50099, #7009, .T. ) ;
#39935 = VECTOR ( 'NONE', #31462, 1000.000000000000000 ) ;
#39936 = VECTOR ( 'NONE', #24605, 1000.000000000000000 ) ;
#39937 = ORIENTED_EDGE ( 'NONE', *, *, #41098, .T. ) ;
#39938 = CARTESIAN_POINT ( 'NONE',  ( 34.93559171950835918, -177.1207230881787780, -93.09664195018497423 ) ) ;
#39939 = AXIS2_PLACEMENT_3D ( 'NONE', #22084, #18917, #33908 ) ;
#39940 = AXIS2_PLACEMENT_3D ( 'NONE', #35778, #48669, #47632 ) ;
#39941 = ORIENTED_EDGE ( 'NONE', *, *, #12778, .F. ) ;
#39942 = CARTESIAN_POINT ( 'NONE',  ( -47.51449116960048968, -189.7472609257535510, 0.2635871660690785045 ) ) ;
#39943 = LINE ( 'NONE', #7132, #43688 ) ;
#39946 = VERTEX_POINT ( 'NONE', #39322 ) ;
#39945 = DIRECTION ( 'NONE',  ( -0.000000000000000000, 0.1205366802553337752, 0.9927088740980526405 ) ) ;
#39944 = LINE ( 'NONE', #16312, #40913 ) ;
#39947 = VECTOR ( 'NONE', #48401, 1000.000000000000000 ) ;
#39948 = ADVANCED_FACE ( 'NONE', ( #47471 ), #27219, .T. ) ;
#39949 = VECTOR ( 'NONE', #45200, 1000.000000000000000 ) ;
#39950 = CARTESIAN_POINT ( 'NONE',  ( -336.3521761649654422, -70.03480886230919111, 25.08789112700620194 ) ) ;
#39951 = ADVANCED_BREP_SHAPE_REPRESENTATION ( '', ( #36319, #31742 ), #2380 ) ;
#39953 = ORIENTED_EDGE ( 'NONE', *, *, #10944, .T. ) ;
#39952 = AXIS2_PLACEMENT_3D ( 'NONE', #37790, #37545, #34871 ) ;
#39954 = DIRECTION ( 'NONE',  ( -0.000000000000000000, -1.000000000000000000, -0.000000000000000000 ) ) ;
#39955 = EDGE_LOOP ( 'NONE', ( #30397, #27963, #39670, #12199 ) ) ;
#39956 = CARTESIAN_POINT ( 'NONE',  ( -123.0610352593084400, -189.7472609257535510, 99.06333546307732263 ) ) ;
#39957 = VECTOR ( 'NONE', #18567, 1000.000000000000000 ) ;
#39958 = CARTESIAN_POINT ( 'NONE',  ( -332.3517673607765914, -66.84438072661991725, -16.67542351306652648 ) ) ;
#39960 = DIRECTION ( 'NONE',  ( -0.000000000000000000, 1.000000000000000000, -0.000000000000000000 ) ) ;
#39959 = CARTESIAN_POINT ( 'NONE',  ( -305.0000000000000568, -109.6270296344161750, -58.37414404713471328 ) ) ;
#39961 = VERTEX_POINT ( 'NONE', #27744 ) ;
#39962 = CONICAL_SURFACE ( 'NONE', #6468, 4.042878180043863345, 0.07858164904571392217 ) ;
#39963 = DIRECTION ( 'NONE',  ( 0.6965510290629982615, 0.000000000000000000, -0.7175072570443298270 ) ) ;
#39964 = PLANE ( 'NONE',  #16948 ) ;
#39965 = CARTESIAN_POINT ( 'NONE',  ( -37.67038537088846084, -193.5000000000000000, -124.5318076226586470 ) ) ;
#39966 = VERTEX_POINT ( 'NONE', #19357 ) ;
#39967 = DIRECTION ( 'NONE',  ( 0.000000000000000000, 1.000000000000000000, 0.000000000000000000 ) ) ;
#39968 = CARTESIAN_POINT ( 'NONE',  ( -151.4272465800706016, -183.6283474603465606, 70.89911581792887318 ) ) ;
#39969 = ORIENTED_EDGE ( 'NONE', *, *, #4147, .F. ) ;
#39970 = LINE ( 'NONE', #20020, #10808 ) ;
#39971 = PLANE ( 'NONE',  #20599 ) ;
#39972 = ORIENTED_EDGE ( 'NONE', *, *, #15698, .T. ) ;
#39973 = DIRECTION ( 'NONE',  ( -0.8610436117673548884, 0.000000000000000000, -0.5085311186492216251 ) ) ;
#39974 = ORIENTED_EDGE ( 'NONE', *, *, #13061, .F. ) ;
#39975 = VECTOR ( 'NONE', #9222, 1000.000000000000000 ) ;
#39976 = VECTOR ( 'NONE', #7932, 1000.000000000000000 ) ;
#39977 = LINE ( 'NONE', #16624, #34040 ) ;
#39978 = CARTESIAN_POINT ( 'NONE',  ( -330.4913330509368166, -123.5000000000000284, 0.000000000000000000 ) ) ;
#39979 = VECTOR ( 'NONE', #9927, 1000.000000000000000 ) ;
#39980 = DIRECTION ( 'NONE',  ( 0.000000000000000000, -1.000000000000000000, -0.000000000000000000 ) ) ;
#39981 = ADVANCED_FACE ( 'NONE', ( #43776 ), #35119, .T. ) ;
#39982 = CARTESIAN_POINT ( 'NONE',  ( -332.3517673607765914, -149.9277501395804677, 53.86626052140529453 ) ) ;
#39983 = CARTESIAN_POINT ( 'NONE',  ( -339.1964088526558498, -178.8432607619609485, -20.45418021416653076 ) ) ;
#39984 = ADVANCED_FACE ( 'NONE', ( #3573 ), #7269, .F. ) ;
#39985 = CARTESIAN_POINT ( 'NONE',  ( 1.734723475976807489E-15, -43.50000000000000000, -30.00000000000000711 ) ) ;
#39986 = VECTOR ( 'NONE', #32205, 1000.000000000000114 ) ;
#39987 = VECTOR ( 'NONE', #45753, 1000.000000000000000 ) ;
#39988 = DIRECTION ( 'NONE',  ( -0.000000000000000000, 1.000000000000000000, -0.000000000000000000 ) ) ;
#39989 = DIRECTION ( 'NONE',  ( 0.000000000000000000, -1.000000000000000000, 0.000000000000000000 ) ) ;
#39991 = EDGE_LOOP ( 'NONE', ( #10632, #15594, #46220, #15988 ) ) ;
#39990 = DIRECTION ( 'NONE',  ( 0.000000000000000000, 0.9927088740980548609, 0.1205366802553164696 ) ) ;
#39992 = VECTOR ( 'NONE', #28195, 999.9999999999998863 ) ;
#39993 = CIRCLE ( 'NONE', #22384, 125.0000000000000000 ) ;
#39994 = EDGE_LOOP ( 'NONE', ( #27020, #23577, #28036, #33382 ) ) ;
#39995 = CARTESIAN_POINT ( 'NONE',  ( -142.2007120195389405, -193.5000000000000000, 81.19354792697798473 ) ) ;
#39996 = ADVANCED_FACE ( 'NONE', ( #15682, #8041, #44036, #48774, #24328, #16455, #20121, #32731, #16975, #24580, #32474, #4355, #21165, #40867, #40334, #4110, #48250, #16192, #49027, #24082, #45102, #48526, #928, #12743, #28768, #4614, #36150, #41132, #44821, #36938, #28002, #40093, #44560, #36404, #9089, #147, #32208, #12500, #12230, #5150, #28267, #28515, #8547, #44316, #37188, #8306, #25121, #20379, #40597, #399, #11969, #36678 ), #20642, .T. ) ;
#39997 = AXIS2_PLACEMENT_3D ( 'NONE', #18262, #46900, #5665 ) ;
#39998 = EDGE_CURVE ( 'NONE', #12264, #47175, #33766, .T. ) ;
#39999 = AXIS2_PLACEMENT_3D ( 'NONE', #12576, #7357, #3923 ) ;
#40000 = CARTESIAN_POINT ( 'NONE',  ( -339.1964088526558498, -66.33409060400673241, -14.60509510167901404 ) ) ;
#40001 = VERTEX_POINT ( 'NONE', #4891 ) ;
#40002 = ORIENTED_EDGE ( 'NONE', *, *, #44320, .F. ) ;
#40003 = EDGE_CURVE ( 'NONE', #41331, #17289, #20918, .T. ) ;
#40004 = VERTEX_POINT ( 'NONE', #29035 ) ;
#40005 = DIRECTION ( 'NONE',  ( 0.000000000000000000, 0.9709418174260534551, 0.2393156642875516327 ) ) ;
#40006 = LINE ( 'NONE', #35818, #48501 ) ;
#40007 = CARTESIAN_POINT ( 'NONE',  ( -48.47912675150885065, -189.7472609257535510, 6.938893903907228378E-15 ) ) ;
#40008 = CARTESIAN_POINT ( 'NONE',  ( -41.30311180514221547, -175.3837268820161057, 123.7921848946937899 ) ) ;
#40009 = ORIENTED_EDGE ( 'NONE', *, *, #43642, .T. ) ;
#40010 = ORIENTED_EDGE ( 'NONE', *, *, #21463, .F. ) ;
#40011 = ORIENTED_EDGE ( 'NONE', *, *, #5861, .T. ) ;
#40012 = LINE ( 'NONE', #4038, #25796 ) ;
#40013 = DIRECTION ( 'NONE',  ( -0.000000000000000000, 1.000000000000000000, -0.000000000000000000 ) ) ;
#40014 = CIRCLE ( 'NONE', #5656, 125.0000000000000000 ) ;
#40015 = LINE ( 'NONE', #50843, #577 ) ;
#40016 = VECTOR ( 'NONE', #50749, 1000.000000000000000 ) ;
#40017 = DIRECTION ( 'NONE',  ( -0.8757349421956412971, 0.000000000000000000, 0.4827922027307366970 ) ) ;
#40018 = DIRECTION ( 'NONE',  ( -1.000000000000000000, 1.036104688092334944E-14, -1.258058860540643439E-15 ) ) ;
#40019 = VERTEX_POINT ( 'NONE', #47989 ) ;
#40020 = CARTESIAN_POINT ( 'NONE',  ( -114.9600645115007040, -193.5000000000000000, 105.8550183720738573 ) ) ;
#40021 = VECTOR ( 'NONE', #28686, 1000.000000000000000 ) ;
#40022 = FACE_OUTER_BOUND ( 'NONE', #3581, .T. ) ;
#40023 = DIRECTION ( 'NONE',  ( 0.000000000000000000, 0.000000000000000000, -1.000000000000000000 ) ) ;
#40024 = DIRECTION ( 'NONE',  ( -0.000000000000000000, 1.000000000000000000, -0.000000000000000000 ) ) ;
#40025 = ORIENTED_EDGE ( 'NONE', *, *, #11802, .T. ) ;
#40026 = EDGE_LOOP ( 'NONE', ( #6316, #5414, #14423, #48900 ) ) ;
#40027 = VECTOR ( 'NONE', #39746, 1000.000000000000000 ) ;
#40028 = VERTEX_POINT ( 'NONE', #10368 ) ;
#40029 = DIRECTION ( 'NONE',  ( 1.043714542225393697E-14, 0.8229838658936495799, -0.5680647467311656929 ) ) ;
#40030 = LINE ( 'NONE', #16142, #42620 ) ;
#40031 = ORIENTED_EDGE ( 'NONE', *, *, #39998, .T. ) ;
#40032 = CARTESIAN_POINT ( 'NONE',  ( -332.3517673607765914, -114.7679482383557144, 58.37307289257701370 ) ) ;
#40033 = VECTOR ( 'NONE', #28650, 1000.000000000000114 ) ;
#40034 = CARTESIAN_POINT ( 'NONE',  ( -332.3517673607765914, -125.1322888500942270, -59.00000000000002132 ) ) ;
#40035 = DIRECTION ( 'NONE',  ( 1.000000000000000000, 0.000000000000000000, 0.000000000000000000 ) ) ;
#40036 = ORIENTED_EDGE ( 'NONE', *, *, #10104, .T. ) ;
#40037 = LINE ( 'NONE', #48208, #35986 ) ;
#40038 = AXIS2_PLACEMENT_3D ( 'NONE', #4543, #20565, #9272 ) ;
#40039 = AXIS2_PLACEMENT_3D ( 'NONE', #11786, #35706, #3392 ) ;
#40040 = EDGE_LOOP ( 'NONE', ( #6257, #30211, #6359, #38624 ) ) ;
#40041 = CARTESIAN_POINT ( 'NONE',  ( -48.47912675150885065, -183.6283474603465606, 6.938893903907228378E-15 ) ) ;
#40042 = VERTEX_POINT ( 'NONE', #18006 ) ;
#40043 = DIRECTION ( 'NONE',  ( 0.000000000000000000, 1.000000000000000000, 0.000000000000000000 ) ) ;
#40044 = FACE_OUTER_BOUND ( 'NONE', #26336, .T. ) ;
#40045 = ORIENTED_EDGE ( 'NONE', *, *, #45908, .F. ) ;
#40046 = EDGE_CURVE ( 'NONE', #12833, #40482, #17753, .T. ) ;
#40047 = LINE ( 'NONE', #12458, #18158 ) ;
#40048 = EDGE_CURVE ( 'NONE', #21919, #51603, #22476, .T. ) ;
#40049 = DIRECTION ( 'NONE',  ( 0.5085311186492154079, 0.000000000000000000, 0.8610436117673585521 ) ) ;
#40050 = CARTESIAN_POINT ( 'NONE',  ( -43.48323084606168720, -193.5000000000000000, 124.9001241957026167 ) ) ;
#40051 = EDGE_CURVE ( 'NONE', #44024, #27852, #18273, .T. ) ;
#40052 = DIRECTION ( 'NONE',  ( -0.000000000000000000, 1.000000000000000000, -0.000000000000000000 ) ) ;
#40053 = EDGE_CURVE ( 'NONE', #10162, #50250, #30373, .T. ) ;
#40054 = VERTEX_POINT ( 'NONE', #6445 ) ;
#40055 = DIRECTION ( 'NONE',  ( -1.000000000000000000, 0.000000000000000000, 0.000000000000000000 ) ) ;
#40056 = EDGE_CURVE ( 'NONE', #5333, #10177, #50331, .T. ) ;
#40057 = ORIENTED_EDGE ( 'NONE', *, *, #17296, .T. ) ;
#40058 = EDGE_LOOP ( 'NONE', ( #25754, #35057, #50274, #1175 ) ) ;
#40059 = AXIS2_PLACEMENT_3D ( 'NONE', #22790, #15173, #27229 ) ;
#40060 = AXIS2_PLACEMENT_3D ( 'NONE', #16016, #48327, #24663 ) ;
#40061 = ADVANCED_FACE ( 'NONE', ( #9599 ), #34026, .F. ) ;
#40062 = CARTESIAN_POINT ( 'NONE',  ( 0.000000000000000000, -79.33786585790510060, -39.12423683620700388 ) ) ;
#40064 = ORIENTED_EDGE ( 'NONE', *, *, #36239, .T. ) ;
#40063 = FACE_OUTER_BOUND ( 'NONE', #12761, .T. ) ;
#40065 = EDGE_CURVE ( 'NONE', #39601, #33164, #14319, .T. ) ;
#40066 = CIRCLE ( 'NONE', #2313, 4.999999999999997335 ) ;
#40067 = ORIENTED_EDGE ( 'NONE', *, *, #16347, .T. ) ;
#40068 = CARTESIAN_POINT ( 'NONE',  ( 27.23560471289042439, -189.7472609257535510, 99.45993886622848379 ) ) ;
#40069 = ADVANCED_FACE ( 'NONE', ( #49559 ), #42161, .F. ) ;
#40070 = ADVANCED_FACE ( 'NONE', ( #37445 ), #13285, .F. ) ;
#40071 = FACE_OUTER_BOUND ( 'NONE', #43575, .T. ) ;
#40072 = AXIS2_PLACEMENT_3D ( 'NONE', #47460, #4097, #20366 ) ;
#40073 = ORIENTED_EDGE ( 'NONE', *, *, #24366, .F. ) ;
#40074 = EDGE_CURVE ( 'NONE', #35455, #18186, #33767, .T. ) ;
#40075 = CARTESIAN_POINT ( 'NONE',  ( 46.00000000000000711, 20.00000000000000000, 46.00000000000000000 ) ) ;
#40076 = AXIS2_PLACEMENT_3D ( 'NONE', #8686, #12882, #17109 ) ;
#40077 = CARTESIAN_POINT ( 'NONE',  ( -5.113431607746556473, -175.3837268820161057, 117.2365833888819537 ) ) ;
#40078 = ORIENTED_EDGE ( 'NONE', *, *, #25723, .T. ) ;
#40079 = LINE ( 'NONE', #20111, #48506 ) ;
#40080 = FACE_OUTER_BOUND ( 'NONE', #42551, .T. ) ;
#40081 = VECTOR ( 'NONE', #9610, 1000.000000000000000 ) ;
#40082 = EDGE_CURVE ( 'NONE', #27333, #6252, #43812, .T. ) ;
#40083 = AXIS2_PLACEMENT_3D ( 'NONE', #46282, #18155, #45752 ) ;
#40084 = FACE_OUTER_BOUND ( 'NONE', #51101, .T. ) ;
#40085 = DIRECTION ( 'NONE',  ( 0.2920567706369694982, 0.000000000000000000, 0.9564009842765243130 ) ) ;
#40086 = EDGE_LOOP ( 'NONE', ( #32044, #27671, #36027, #27277 ) ) ;
#40087 = ORIENTED_EDGE ( 'NONE', *, *, #195, .T. ) ;
#40088 = EDGE_LOOP ( 'NONE', ( #8815, #24310, #20246, #36439 ) ) ;
#40089 = VECTOR ( 'NONE', #33638, 999.9999999999998863 ) ;
#40090 = FACE_OUTER_BOUND ( 'NONE', #5408, .T. ) ;
#40091 = FACE_OUTER_BOUND ( 'NONE', #37184, .T. ) ;
#40092 = DIRECTION ( 'NONE',  ( 0.000000000000000000, 0.000000000000000000, 1.000000000000000000 ) ) ;
#40093 = FACE_BOUND ( 'NONE', #14306, .T. ) ;
#40094 = DIRECTION ( 'NONE',  ( 0.000000000000000000, 0.000000000000000000, 1.000000000000000000 ) ) ;
#40095 = VERTEX_POINT ( 'NONE', #1178 ) ;
#40096 = EDGE_CURVE ( 'NONE', #49147, #33399, #6908, .T. ) ;
#40097 = DIRECTION ( 'NONE',  ( -0.000000000000000000, 1.000000000000000000, -0.000000000000000000 ) ) ;
#40098 = ORIENTED_EDGE ( 'NONE', *, *, #21753, .F. ) ;
#40100 = ORIENTED_EDGE ( 'NONE', *, *, #44337, .F. ) ;
#40099 = DIRECTION ( 'NONE',  ( 0.000000000000000000, -1.000000000000000000, 0.000000000000000000 ) ) ;
#40101 = VECTOR ( 'NONE', #874, 1000.000000000000000 ) ;
#40102 = VERTEX_POINT ( 'NONE', #1968 ) ;
#40103 = VECTOR ( 'NONE', #45373, 1000.000000000000000 ) ;
#40104 = CARTESIAN_POINT ( 'NONE',  ( -158.9435005891548371, -193.5000000000000000, -56.33604425924755077 ) ) ;
#40105 = DIRECTION ( 'NONE',  ( 0.000000000000000000, 0.000000000000000000, 1.000000000000000000 ) ) ;
#40106 = CIRCLE ( 'NONE', #40932, 125.0000000000000000 ) ;
#40107 = CARTESIAN_POINT ( 'NONE',  ( -49.13194886969938580, -193.5000000000000000, 0.7575112421616214675 ) ) ;
#40108 = CARTESIAN_POINT ( 'NONE',  ( -49.47868758801764955, -175.3837268820161057, 0.02963332782255607284 ) ) ;
#40109 = ORIENTED_EDGE ( 'NONE', *, *, #36515, .T. ) ;
#40110 = DIRECTION ( 'NONE',  ( 0.000000000000000000, 0.000000000000000000, -1.000000000000000000 ) ) ;
#40111 = ORIENTED_EDGE ( 'NONE', *, *, #4205, .F. ) ;
#40112 = EDGE_CURVE ( 'NONE', #34695, #32136, #14071, .T. ) ;
#40113 = ORIENTED_EDGE ( 'NONE', *, *, #37088, .T. ) ;
#40114 = DIRECTION ( 'NONE',  ( -0.000000000000000000, 1.000000000000000000, 0.000000000000000000 ) ) ;
#40115 = AXIS2_PLACEMENT_3D ( 'NONE', #37310, #34147, #25748 ) ;
#40116 = CARTESIAN_POINT ( 'NONE',  ( -339.1964088526558498, -130.1153096980153236, -58.63009191191284941 ) ) ;
#40117 = CARTESIAN_POINT ( 'NONE',  ( -48.47912675150885065, -183.6283474603465606, 6.938893903907228378E-15 ) ) ;
#40118 = EDGE_CURVE ( 'NONE', #38437, #2241, #41388, .T. ) ;
#40119 = EDGE_CURVE ( 'NONE', #49227, #27750, #16973, .T. ) ;
#40120 = DIRECTION ( 'NONE',  ( 0.000000000000000000, 0.000000000000000000, -1.000000000000000000 ) ) ;
#40121 = CARTESIAN_POINT ( 'NONE',  ( -20.16057156355605784, -175.3837268820161057, -120.7230919990158782 ) ) ;
#40122 = ADVANCED_FACE ( 'NONE', ( #6183 ), #33520, .F. ) ;
#40123 = ORIENTED_EDGE ( 'NONE', *, *, #26750, .F. ) ;
#40124 = LINE ( 'NONE', #23578, #30506 ) ;
#40125 = CARTESIAN_POINT ( 'NONE',  ( -339.1964088526558498, -178.4886558749180949, 21.38919645685277970 ) ) ;
#40126 = EDGE_CURVE ( 'NONE', #34274, #39306, #5238, .T. ) ;
#40127 = CIRCLE ( 'NONE', #7435, 125.0000000000000000 ) ;
#40128 = FACE_BOUND ( 'NONE', #27701, .T. ) ;
#40129 = EDGE_LOOP ( 'NONE', ( #48269, #48542, #3250, #45589 ) ) ;
#40130 = CARTESIAN_POINT ( 'NONE',  ( -46.12632737020502560, -193.5000000000000000, -123.9784823535113532 ) ) ;
#40131 = DIRECTION ( 'NONE',  ( 0.000000000000000000, 0.000000000000000000, -1.000000000000000000 ) ) ;
#40132 = ORIENTED_EDGE ( 'NONE', *, *, #9604, .F. ) ;
#40133 = DIRECTION ( 'NONE',  ( 0.000000000000000000, 0.9709418174260526779, 0.2393156642875547968 ) ) ;
#40134 = EDGE_CURVE ( 'NONE', #33953, #42476, #3270, .T. ) ;
#40135 = ORIENTED_EDGE ( 'NONE', *, *, #26364, .F. ) ;
#40136 = CIRCLE ( 'NONE', #14128, 10.99999999999999645 ) ;
#40137 = CARTESIAN_POINT ( 'NONE',  ( 27.42205759510523677, -193.5000000000000000, 98.05618656931996213 ) ) ;
#40138 = VECTOR ( 'NONE', #41338, 1000.000000000000000 ) ;
#40139 = ADVANCED_FACE ( 'NONE', ( #15356 ), #38490, .T. ) ;
#40140 = AXIS2_PLACEMENT_3D ( 'NONE', #36526, #47611, #11591 ) ;
#40141 = FACE_BOUND ( 'NONE', #31756, .T. ) ;
#40143 = ORIENTED_EDGE ( 'NONE', *, *, #39302, .T. ) ;
#40142 = CARTESIAN_POINT ( 'NONE',  ( -336.3521761649654422, -68.91285928486892942, -22.44790492310182017 ) ) ;
#40144 = AXIS2_PLACEMENT_3D ( 'NONE', #7128, #15031, #42611 ) ;
#40145 = EDGE_CURVE ( 'NONE', #32545, #50673, #42693, .T. ) ;
#40146 = DIRECTION ( 'NONE',  ( -8.718379230999705894E-17, 0.8229838658936536877, -0.5680647467311596976 ) ) ;
#40147 = ORIENTED_EDGE ( 'NONE', *, *, #49630, .F. ) ;
#40148 = ADVANCED_FACE ( 'NONE', ( #19304 ), #18651, .T. ) ;
#40149 = ORIENTED_EDGE ( 'NONE', *, *, #5396, .F. ) ;
#40150 = DIRECTION ( 'NONE',  ( -0.000000000000000000, -1.000000000000000000, 0.000000000000000000 ) ) ;
#40151 = VECTOR ( 'NONE', #22529, 1000.000000000000000 ) ;
#40152 = ORIENTED_EDGE ( 'NONE', *, *, #7419, .F. ) ;
#40153 = DIRECTION ( 'NONE',  ( 0.000000000000000000, 0.000000000000000000, -1.000000000000000000 ) ) ;
#40154 = CARTESIAN_POINT ( 'NONE',  ( 67.04262753014327814, -189.7472609257535510, -47.74645837849745078 ) ) ;
#40155 = VECTOR ( 'NONE', #26789, 1000.000000000000000 ) ;
#40156 = EDGE_CURVE ( 'NONE', #48767, #30683, #38774, .T. ) ;
#40157 = LINE ( 'NONE', #40400, #51094 ) ;
#40158 = DIRECTION ( 'NONE',  ( -1.000000000000000000, -0.000000000000000000, -0.000000000000000000 ) ) ;
#40159 = EDGE_LOOP ( 'NONE', ( #5605, #3114, #2716, #34891 ) ) ;
#40162 = ORIENTED_EDGE ( 'NONE', *, *, #22600, .T. ) ;
#40161 = DIRECTION ( 'NONE',  ( 1.000000000000000000, 0.000000000000000000, 0.000000000000000000 ) ) ;
#40160 = CARTESIAN_POINT ( 'NONE',  ( -332.3517673607765914, -177.3662605214052519, -26.42775013958060271 ) ) ;
#40163 = EDGE_LOOP ( 'NONE', ( #24382, #44045, #9790, #19600 ) ) ;
#40164 = LINE ( 'NONE', #214, #27332 ) ;
#40165 = VERTEX_POINT ( 'NONE', #35309 ) ;
#40166 = PLANE ( 'NONE',  #7949 ) ;
#40167 = ORIENTED_EDGE ( 'NONE', *, *, #37879, .T. ) ;
#40168 = FACE_OUTER_BOUND ( 'NONE', #18427, .T. ) ;
#40169 = EDGE_LOOP ( 'NONE', ( #10330, #2359, #23865, #17198 ) ) ;
#40171 = FACE_OUTER_BOUND ( 'NONE', #39027, .T. ) ;
#40170 = CARTESIAN_POINT ( 'NONE',  ( -111.3295483157475445, -189.7472609257535510, 108.0501018472332504 ) ) ;
#40172 = ORIENTED_EDGE ( 'NONE', *, *, #10991, .T. ) ;
#40173 = ORIENTED_EDGE ( 'NONE', *, *, #7847, .T. ) ;
#40174 = FACE_OUTER_BOUND ( 'NONE', #48745, .T. ) ;
#40175 = VECTOR ( 'NONE', #10582, 1000.000000000000000 ) ;
#40176 = CARTESIAN_POINT ( 'NONE',  ( -72.96029774493611342, -193.5000000000000000, 122.5792489240759409 ) ) ;
#40177 = MECHANICAL_DESIGN_GEOMETRIC_PRESENTATION_REPRESENTATION (  '', ( #7446 ), #9970 ) ;
#40178 = CARTESIAN_POINT ( 'NONE',  ( -336.3521761649654422, -88.64083255475578937, 47.62880233550460218 ) ) ;
#40179 = LINE ( 'NONE', #48070, #39230 ) ;
#40180 = CARTESIAN_POINT ( 'NONE',  ( -48.47912675150885065, -183.6283474603465606, 6.938893903907228378E-15 ) ) ;
#40181 = SHAPE_REPRESENTATION ( 'Lockable Linear Guide', ( #31742 ), #8256 ) ;
#40182 = AXIS2_PLACEMENT_3D ( 'NONE', #25752, #41785, #20773 ) ;
#40183 = FACE_OUTER_BOUND ( 'NONE', #28985, .T. ) ;
#40184 = ORIENTED_EDGE ( 'NONE', *, *, #29528, .F. ) ;
#40185 = EDGE_CURVE ( 'NONE', #46675, #13353, #6701, .T. ) ;
#40186 = ADVANCED_FACE ( 'NONE', ( #34531 ), #51608, .F. ) ;
#40187 = CARTESIAN_POINT ( 'NONE',  ( -149.5539421794694022, -189.7472609257535510, 73.54509967498655953 ) ) ;
#40188 = DIRECTION ( 'NONE',  ( -0.9995608365087946812, 0.000000000000000000, 0.02963332782254913048 ) ) ;
#40189 = CARTESIAN_POINT ( 'NONE',  ( -330.4913330509368166, -131.1080185721132807, -58.50955523165751515 ) ) ;
#40190 = EDGE_LOOP ( 'NONE', ( #12737, #31715, #224, #38429 ) ) ;
#40191 = VECTOR ( 'NONE', #2006, 1000.000000000000114 ) ;
#40192 = DIRECTION ( 'NONE',  ( 0.000000000000000000, 0.000000000000000000, -1.000000000000000000 ) ) ;
#40193 = DIRECTION ( 'NONE',  ( 0.000000000000000000, 0.000000000000000000, 1.000000000000000000 ) ) ;
#40194 = DIRECTION ( 'NONE',  ( 0.000000000000000000, 0.4647231720437789981, 0.8854560256532044704 ) ) ;
#40195 = ORIENTED_EDGE ( 'NONE', *, *, #5860, .T. ) ;
#40196 = EDGE_LOOP ( 'NONE', ( #4910, #42878, #16287, #8862 ) ) ;
#40197 = ORIENTED_EDGE ( 'NONE', *, *, #45212, .T. ) ;
#40198 = AXIS2_PLACEMENT_3D ( 'NONE', #42438, #9876, #41925 ) ;
#40199 = CARTESIAN_POINT ( 'NONE',  ( -154.6193097927903182, -193.5000000000000000, -66.02470404298122730 ) ) ;
#40200 = DIRECTION ( 'NONE',  ( 0.000000000000000000, -1.000000000000000000, -0.000000000000000000 ) ) ;
#40201 = ADVANCED_FACE ( 'NONE', ( #50582 ), #11660, .F. ) ;
#40202 = LINE ( 'NONE', #12341, #6117 ) ;
#40203 = PLANE ( 'NONE',  #51405 ) ;
#40204 = ORIENTED_EDGE ( 'NONE', *, *, #13541, .F. ) ;
#40205 = DIRECTION ( 'NONE',  ( -0.7575112421616284619, 0.000000000000000000, 0.6528221181905119463 ) ) ;
#40206 = EDGE_CURVE ( 'NONE', #14560, #5201, #38729, .T. ) ;
#40207 = ORIENTED_EDGE ( 'NONE', *, *, #23419, .F. ) ;
#40208 = VECTOR ( 'NONE', #46751, 1000.000000000000000 ) ;
#40209 = ORIENTED_EDGE ( 'NONE', *, *, #43627, .T. ) ;
#40210 = DIRECTION ( 'NONE',  ( -0.000000000000000000, 0.9709418174260519008, -0.2393156642875582940 ) ) ;
#40211 = VECTOR ( 'NONE', #6506, 1000.000000000000000 ) ;
#40212 = ORIENTED_EDGE ( 'NONE', *, *, #12754, .T. ) ;
#40213 = DIRECTION ( 'NONE',  ( 0.000000000000000000, 0.000000000000000000, -1.000000000000000000 ) ) ;
#40214 = CARTESIAN_POINT ( 'NONE',  ( -332.3517673607765914, -173.5513585866778214, -31.34948880313881503 ) ) ;
#40217 = ORIENTED_EDGE ( 'NONE', *, *, #32585, .F. ) ;
#40216 = CARTESIAN_POINT ( 'NONE',  ( -339.1964088526558498, -115.8919814278862503, 58.50955523165745831 ) ) ;
#40215 = DIRECTION ( 'NONE',  ( -1.000000000000000000, 1.258058860540389820E-15, -1.036104688092337784E-14 ) ) ;
#40218 = DIRECTION ( 'NONE',  ( 0.000000000000000000, 0.000000000000000000, -1.000000000000000000 ) ) ;
#40219 = EDGE_LOOP ( 'NONE', ( #33667, #36073, #2778, #28223 ) ) ;
#40220 = DIRECTION ( 'NONE',  ( -0.000000000000000000, 0.3546048870425463906, 0.9350162426854107256 ) ) ;
#40221 = VERTEX_POINT ( 'NONE', #23244 ) ;
#40222 = CARTESIAN_POINT ( 'NONE',  ( -48.53836737940257251, -175.3837268820161057, 0.9982437317643279018 ) ) ;
#40223 = LINE ( 'NONE', #4239, #51508 ) ;
#40225 = LINE ( 'NONE', #544, #18112 ) ;
#40224 = CARTESIAN_POINT ( 'NONE',  ( 7.859956736328458149, -189.7472609257535510, -111.5836353223468649 ) ) ;
#40226 = ORIENTED_EDGE ( 'NONE', *, *, #31761, .F. ) ;
#40227 = AXIS2_PLACEMENT_3D ( 'NONE', #22991, #35077, #23509 ) ;
#40228 = DIRECTION ( 'NONE',  ( 0.000000000000000000, 0.8854560256532110207, 0.4647231720437664526 ) ) ;
#40229 = CARTESIAN_POINT ( 'NONE',  ( -336.3521761649653854, -63.76276212672765809, 5.609136410542458151 ) ) ;
#40230 = VERTEX_POINT ( 'NONE', #7473 ) ;
#40231 = DIRECTION ( 'NONE',  ( 0.8124868780056783146, 0.000000000000000000, 0.5829794791144762289 ) ) ;
#40232 = CARTESIAN_POINT ( 'NONE',  ( -339.1964088526558498, -123.5000000000000284, 0.000000000000000000 ) ) ;
#40233 = DIRECTION ( 'NONE',  ( 0.000000000000000000, -0.7485107481711046340, -0.6631226582407911962 ) ) ;
#40234 = ORIENTED_EDGE ( 'NONE', *, *, #13683, .F. ) ;
#40235 = EDGE_CURVE ( 'NONE', #32301, #17165, #2736, .T. ) ;
#40236 = DIRECTION ( 'NONE',  ( 0.6068001458186002006, 0.000000000000000000, -0.7948544414133481562 ) ) ;
#40237 = CARTESIAN_POINT ( 'NONE',  ( -72.96029774493611342, -183.6283474603465606, 122.5792489240759409 ) ) ;
#40238 = ORIENTED_EDGE ( 'NONE', *, *, #14684, .F. ) ;
#40239 = PLANE ( 'NONE',  #29620 ) ;
#40240 = ORIENTED_EDGE ( 'NONE', *, *, #25440, .F. ) ;
#40241 = VECTOR ( 'NONE', #11700, 1000.000000000000000 ) ;
#40242 = DIRECTION ( 'NONE',  ( 0.000000000000000000, -1.000000000000000000, 0.000000000000000000 ) ) ;
#40243 = DIRECTION ( 'NONE',  ( 0.000000000000000000, -0.000000000000000000, 1.000000000000000000 ) ) ;
#40244 = LINE ( 'NONE', #7169, #32777 ) ;
#40245 = CARTESIAN_POINT ( 'NONE',  ( -48.30223647638628393, -189.7472609257535510, 0.9842305779476049343 ) ) ;
#40246 = LINE ( 'NONE', #28939, #24924 ) ;
#40247 = CARTESIAN_POINT ( 'NONE',  ( -15.81236726369127155, -183.6283474603465606, -120.6560517527615559 ) ) ;
#40248 = CARTESIAN_POINT ( 'NONE',  ( -166.8403286750647680, -175.3837268820161057, -40.19484891389966918 ) ) ;
#40249 = EDGE_CURVE ( 'NONE', #42721, #51264, #10630, .T. ) ;
#40250 = DIRECTION ( 'NONE',  ( -0.000000000000000000, 0.6631226582408016323, 0.7485107481710953081 ) ) ;
#40252 = ORIENTED_EDGE ( 'NONE', *, *, #28354, .T. ) ;
#40251 = DIRECTION ( 'NONE',  ( 0.000000000000000000, 1.000000000000000000, 0.000000000000000000 ) ) ;
#40253 = VERTEX_POINT ( 'NONE', #47679 ) ;
#40254 = DIRECTION ( 'NONE',  ( 0.000000000000000000, -0.3546048870425235200, 0.9350162426854194964 ) ) ;
#40255 = VECTOR ( 'NONE', #18824, 1000.000000000000000 ) ;
#40256 = CIRCLE ( 'NONE', #47009, 125.0000000000000000 ) ;
#40257 = DIRECTION ( 'NONE',  ( 0.000000000000000000, -1.503427012513232710E-14, 1.000000000000000000 ) ) ;
#40258 = ORIENTED_EDGE ( 'NONE', *, *, #19149, .F. ) ;
#40259 = VERTEX_POINT ( 'NONE', #27159 ) ;
#40260 = VERTEX_POINT ( 'NONE', #39263 ) ;
#40261 = DIRECTION ( 'NONE',  ( 0.000000000000000000, 0.000000000000000000, 1.000000000000000000 ) ) ;
#40262 = FACE_OUTER_BOUND ( 'NONE', #23882, .T. ) ;
#40263 = DIRECTION ( 'NONE',  ( 1.000000000000000000, 0.000000000000000000, -0.000000000000000000 ) ) ;
#40264 = EDGE_LOOP ( 'NONE', ( #23149, #38697, #21944, #37823 ) ) ;
#40265 = VERTEX_POINT ( 'NONE', #42939 ) ;
#40266 = EDGE_LOOP ( 'NONE', ( #14144, #2930, #39707, #15521 ) ) ;
#40267 = LINE ( 'NONE', #35306, #36714 ) ;
#40268 = DIRECTION ( 'NONE',  ( 0.7378332790417333475, 0.000000000000000000, -0.6749830015182038956 ) ) ;
#40270 = EDGE_LOOP ( 'NONE', ( #13759, #3485, #18564, #29981 ) ) ;
#40269 = DIRECTION ( 'NONE',  ( 0.000000000000000000, 0.000000000000000000, -1.000000000000000000 ) ) ;
#40271 = AXIS2_PLACEMENT_3D ( 'NONE', #51529, #7124, #23159 ) ;
#40272 = DIRECTION ( 'NONE',  ( 0.000000000000000000, 0.000000000000000000, 1.000000000000000000 ) ) ;
#40273 = DIRECTION ( 'NONE',  ( -0.000000000000000000, -1.000000000000000000, -0.000000000000000000 ) ) ;
#40274 = EDGE_LOOP ( 'NONE', ( #35780, #50651, #49099, #39933 ) ) ;
#40275 = DIRECTION ( 'NONE',  ( 0.000000000000000000, -0.000000000000000000, 1.000000000000000000 ) ) ;
#40276 = ADVANCED_FACE ( 'NONE', ( #43717 ), #18772, .T. ) ;
#40277 = CARTESIAN_POINT ( 'NONE',  ( 33.09766481721657527, -193.5000000000000000, 93.38753978496653474 ) ) ;
#40278 = LINE ( 'NONE', #47684, #20623 ) ;
#40279 = DIRECTION ( 'NONE',  ( 0.9785564922995017012, 0.000000000000000000, 0.2059786187411094538 ) ) ;
#40280 = EDGE_CURVE ( 'NONE', #31839, #41498, #6094, .T. ) ;
#40281 = ORIENTED_EDGE ( 'NONE', *, *, #29075, .T. ) ;
#40282 = VERTEX_POINT ( 'NONE', #26908 ) ;
#40283 = ORIENTED_EDGE ( 'NONE', *, *, #3213, .T. ) ;
#40284 = DIRECTION ( 'NONE',  ( 0.000000000000000000, -1.000000000000000000, 0.000000000000000000 ) ) ;
#40285 = LINE ( 'NONE', #39765, #19967 ) ;
#40286 = VERTEX_POINT ( 'NONE', #38986 ) ;
#40287 = DIRECTION ( 'NONE',  ( 0.000000000000000000, 1.000000000000000000, -0.000000000000000000 ) ) ;
#40288 = FACE_OUTER_BOUND ( 'NONE', #32713, .T. ) ;
#40289 = ORIENTED_EDGE ( 'NONE', *, *, #32604, .F. ) ;
#40290 = EDGE_CURVE ( 'NONE', #36835, #43044, #44687, .T. ) ;
#40291 = CARTESIAN_POINT ( 'NONE',  ( -14.52059121095390815, -193.5000000000000000, 119.2602935412682541 ) ) ;
#40292 = ADVANCED_FACE ( 'NONE', ( #15108 ), #31111, .T. ) ;
#40293 = AXIS2_PLACEMENT_3D ( 'NONE', #21883, #6634, #22655 ) ;
#40294 = VECTOR ( 'NONE', #20540, 1000.000000000000000 ) ;
#40295 = EDGE_LOOP ( 'NONE', ( #14989, #49690, #12781, #35134 ) ) ;
#40296 = DIRECTION ( 'NONE',  ( -0.9151456172430237901, 0.000000000000000000, 0.4031234292879600778 ) ) ;
#40297 = VERTEX_POINT ( 'NONE', #47925 ) ;
#40298 = DIRECTION ( 'NONE',  ( 0.000000000000000000, -9.714451465470119729E-15, -1.000000000000000000 ) ) ;
#40299 = LINE ( 'NONE', #24806, #35162 ) ;
#40300 = ADVANCED_FACE ( 'NONE', ( #8234 ), #27939, .F. ) ;
#40301 = CARTESIAN_POINT ( 'NONE',  ( 21.47984469475713354, -189.7472609257535510, 102.3804074221065292 ) ) ;
#40302 = ORIENTED_EDGE ( 'NONE', *, *, #25153, .F. ) ;
#40303 = LINE ( 'NONE', #4320, #4720 ) ;
#40304 = DIRECTION ( 'NONE',  ( -0.9842305779475992722, 0.000000000000000000, 0.1768902751225592818 ) ) ;
#40305 = FACE_OUTER_BOUND ( 'NONE', #45821, .T. ) ;
#40306 = DIRECTION ( 'NONE',  ( 0.000000000000000000, -1.000000000000000000, 1.047444401652940007E-14 ) ) ;
#40307 = EDGE_LOOP ( 'NONE', ( #12791, #7302, #11912, #1445 ) ) ;
#40308 = CARTESIAN_POINT ( 'NONE',  ( -180.0000000000000568, -115.7896721143442278, 18.45401972188388839 ) ) ;
#40309 = ORIENTED_EDGE ( 'NONE', *, *, #28852, .F. ) ;
#40310 = ORIENTED_EDGE ( 'NONE', *, *, #49242, .F. ) ;
#40311 = CIRCLE ( 'NONE', #28574, 125.0000000000000000 ) ;
#40312 = CARTESIAN_POINT ( 'NONE',  ( -48.36085358058748795, -193.5000000000000000, 0.9929810960135245779 ) ) ;
#40314 = ORIENTED_EDGE ( 'NONE', *, *, #44163, .T. ) ;
#40313 = DIRECTION ( 'NONE',  ( 0.000000000000000000, -0.000000000000000000, 1.000000000000000000 ) ) ;
#40315 = ORIENTED_EDGE ( 'NONE', *, *, #35608, .F. ) ;
#40316 = LINE ( 'NONE', #380, #11413 ) ;
#40317 = LINE ( 'NONE', #4336, #33550 ) ;
#40318 = ORIENTED_EDGE ( 'NONE', *, *, #30096, .T. ) ;
#40319 = CARTESIAN_POINT ( 'NONE',  ( -330.4913330509368166, -178.8432607619606358, 20.45418021416736565 ) ) ;
#40320 = FACE_OUTER_BOUND ( 'NONE', #29751, .T. ) ;
#40321 = VERTEX_POINT ( 'NONE', #40797 ) ;
#40322 = DIRECTION ( 'NONE',  ( 0.000000000000000000, 0.000000000000000000, -1.000000000000000000 ) ) ;
#40323 = DIRECTION ( 'NONE',  ( -0.000000000000000000, 1.000000000000000000, -0.000000000000000000 ) ) ;
#40324 = VECTOR ( 'NONE', #50548, 1000.000000000000000 ) ;
#40325 = CARTESIAN_POINT ( 'NONE',  ( 2.066935079424590871, -189.7472609257535510, -114.3245189510257660 ) ) ;
#40326 = DIRECTION ( 'NONE',  ( -0.000000000000000000, 1.000000000000000000, -0.000000000000000000 ) ) ;
#40327 = ORIENTED_EDGE ( 'NONE', *, *, #1395, .F. ) ;
#40328 = EDGE_LOOP ( 'NONE', ( #13028, #25864, #4673, #50452 ) ) ;
#40330 = ORIENTED_EDGE ( 'NONE', *, *, #22703, .F. ) ;
#40329 = VECTOR ( 'NONE', #22879, 1000.000000000000114 ) ;
#40331 = CARTESIAN_POINT ( 'NONE',  ( -60.00000000000000000, 0.000000000000000000, 60.00000000000000711 ) ) ;
#40332 = LINE ( 'NONE', #20119, #16778 ) ;
#40333 = DIRECTION ( 'NONE',  ( -0.000000000000000000, 0.3546048870425426158, 0.9350162426854120579 ) ) ;
#40334 = FACE_BOUND ( 'NONE', #13999, .T. ) ;
#40335 = CARTESIAN_POINT ( 'NONE',  ( -332.3517673607765914, -123.5000000000000284, 0.000000000000000000 ) ) ;
#40336 = ORIENTED_EDGE ( 'NONE', *, *, #4236, .F. ) ;
#40337 = ADVANCED_FACE ( 'NONE', ( #16127 ), #51882, .T. ) ;
#40338 = EDGE_CURVE ( 'NONE', #14481, #9782, #36344, .T. ) ;
#40339 = VERTEX_POINT ( 'NONE', #32666 ) ;
#40341 = ORIENTED_EDGE ( 'NONE', *, *, #42903, .F. ) ;
#40340 = DIRECTION ( 'NONE',  ( 0.000000000000000000, -0.000000000000000000, 1.000000000000000000 ) ) ;
#40342 = VERTEX_POINT ( 'NONE', #3768 ) ;
#40343 = CONICAL_SURFACE ( 'NONE', #47912, 4.000000000000003553, 0.7853981633974479459 ) ;
#40344 = CARTESIAN_POINT ( 'NONE',  ( 50.27798938500057346, -177.1207230881787780, 74.98773087994526065 ) ) ;
#40345 = EDGE_CURVE ( 'NONE', #4350, #19912, #31887, .T. ) ;
#40346 = CARTESIAN_POINT ( 'NONE',  ( -336.3521761649653854, -182.8437365148560616, 8.849911663702917153 ) ) ;
#40347 = CARTESIAN_POINT ( 'NONE',  ( -339.1964088526558498, -90.39567187580880159, -48.84008046109142498 ) ) ;
#40348 = LINE ( 'NONE', #16204, #51973 ) ;
#40349 = ORIENTED_EDGE ( 'NONE', *, *, #22523, .T. ) ;
#40350 = EDGE_CURVE ( 'NONE', #33085, #43701, #12679, .T. ) ;
#40351 = DIRECTION ( 'NONE',  ( -0.000000000000000000, 1.000000000000000000, -0.000000000000000000 ) ) ;
#40352 = ORIENTED_EDGE ( 'NONE', *, *, #31993, .F. ) ;
#40353 = EDGE_CURVE ( 'NONE', #33115, #33038, #44498, .T. ) ;
#40354 = ORIENTED_EDGE ( 'NONE', *, *, #16090, .T. ) ;
#40355 = CARTESIAN_POINT ( 'NONE',  ( -147.0463339291295881, -183.6283474603465606, 76.87330921200150158 ) ) ;
#40356 = ADVANCED_FACE ( 'NONE', ( #19795 ), #8741, .F. ) ;
#40357 = FACE_OUTER_BOUND ( 'NONE', #10356, .T. ) ;
#40358 = CARTESIAN_POINT ( 'NONE',  ( -172.9089226952081901, -189.7472609257535510, 11.92584929509617986 ) ) ;
#40359 = CARTESIAN_POINT ( 'NONE',  ( -336.3521761649654422, -75.87119766449505676, -34.85916744524372746 ) ) ;
#40360 = VECTOR ( 'NONE', #34698, 1000.000000000000000 ) ;
#40361 = EDGE_CURVE ( 'NONE', #26611, #5889, #179, .T. ) ;
#40362 = CARTESIAN_POINT ( 'NONE',  ( -166.6265240196292439, -175.3837268820161057, 40.81902153125349031 ) ) ;
#40363 = LINE ( 'NONE', #4381, #7762 ) ;
#40364 = ORIENTED_EDGE ( 'NONE', *, *, #26296, .F. ) ;
#40365 = CARTESIAN_POINT ( 'NONE',  ( -336.3521761649654422, -97.52665284734005979, -53.00046796564681983 ) ) ;
#40366 = CARTESIAN_POINT ( 'NONE',  ( -67.22356632362124174, -193.5000000000000000, -123.5865930638409509 ) ) ;
#40367 = VECTOR ( 'NONE', #20416, 1000.000000000000114 ) ;
#40368 = DIRECTION ( 'NONE',  ( 0.000000000000000000, -1.000000000000000000, 0.000000000000000000 ) ) ;
#40369 = FACE_BOUND ( 'NONE', #43177, .T. ) ;
#40370 = ORIENTED_EDGE ( 'NONE', *, *, #20809, .F. ) ;
#40371 = VECTOR ( 'NONE', #41358, 1000.000000000000000 ) ;
#40372 = CARTESIAN_POINT ( 'NONE',  ( -305.0000000000000568, -89.82879061784626629, 49.66134974749640207 ) ) ;
#40373 = FACE_OUTER_BOUND ( 'NONE', #5765, .T. ) ;
#40374 = EDGE_LOOP ( 'NONE', ( #2671, #43131, #10546, #47110 ) ) ;
#40375 = LINE ( 'NONE', #4395, #11998 ) ;
#40376 = ORIENTED_EDGE ( 'NONE', *, *, #32203, .T. ) ;
#40377 = EDGE_CURVE ( 'NONE', #51496, #26301, #13623, .T. ) ;
#40378 = DIRECTION ( 'NONE',  ( 0.000000000000000000, 0.000000000000000000, 1.000000000000000000 ) ) ;
#40379 = VECTOR ( 'NONE', #50834, 1000.000000000000000 ) ;
#40380 = DIRECTION ( 'NONE',  ( 0.000000000000000000, -0.8660254037844354880, 0.5000000000000054401 ) ) ;
#40382 = VERTEX_POINT ( 'NONE', #36086 ) ;
#40381 = CARTESIAN_POINT ( 'NONE',  ( -127.4665351220365324, -183.6283474603465606, -96.88131563365297438 ) ) ;
#40383 = DIRECTION ( 'NONE',  ( -0.000000000000000000, 1.000000000000000000, -0.000000000000000000 ) ) ;
#40384 = ORIENTED_EDGE ( 'NONE', *, *, #40082, .F. ) ;
#40385 = ORIENTED_EDGE ( 'NONE', *, *, #11709, .T. ) ;
#40386 = EDGE_CURVE ( 'NONE', #31640, #20084, #35829, .T. ) ;
#40387 = DIRECTION ( 'NONE',  ( 0.000000000000000000, -0.000000000000000000, -1.000000000000000000 ) ) ;
#40388 = ORIENTED_EDGE ( 'NONE', *, *, #330, .F. ) ;
#40389 = SURFACE_SIDE_STYLE ('',( #737 ) ) ;
#40390 = DIRECTION ( 'NONE',  ( 0.000000000000000000, -1.000000000000000000, 0.000000000000000000 ) ) ;
#40391 = DIRECTION ( 'NONE',  ( 0.000000000000000000, -0.000000000000000000, -1.000000000000000000 ) ) ;
#40392 = CIRCLE ( 'NONE', #26982, 125.0000000000000000 ) ;
#40393 = EDGE_CURVE ( 'NONE', #23372, #3704, #82, .T. ) ;
#40394 = EDGE_CURVE ( 'NONE', #28183, #23609, #48186, .T. ) ;
#40395 = ADVANCED_FACE ( 'NONE', ( #32397 ), #20575, .T. ) ;
#40396 = EDGE_CURVE ( 'NONE', #48950, #48787, #34703, .T. ) ;
#40397 = VECTOR ( 'NONE', #5172, 1000.000000000000000 ) ;
#40398 = ADVANCED_FACE ( 'NONE', ( #39925 ), #31276, .F. ) ;
#40399 = VECTOR ( 'NONE', #48421, 1000.000000000000000 ) ;
#40400 = CARTESIAN_POINT ( 'NONE',  ( -336.3521761649654422, -141.9604555052315220, 56.09938080879057765 ) ) ;
#40401 = CARTESIAN_POINT ( 'NONE',  ( -339.1964088526558498, -144.8891964568526305, -54.98865587491811624 ) ) ;
#40402 = EDGE_LOOP ( 'NONE', ( #44053, #48627, #14519, #34533 ) ) ;
#40405 = VERTEX_POINT ( 'NONE', #27336 ) ;
#40404 = PLANE ( 'NONE',  #48271 ) ;
#40403 = DIRECTION ( 'NONE',  ( -0.000000000000000000, 1.000000000000000000, -0.000000000000000000 ) ) ;
#40406 = VERTEX_POINT ( 'NONE', #39418 ) ;
#40407 = EDGE_CURVE ( 'NONE', #885, #38237, #32104, .T. ) ;
#40408 = DIRECTION ( 'NONE',  ( 0.000000000000000000, -0.000000000000000000, 1.000000000000000000 ) ) ;
#40409 = ORIENTED_EDGE ( 'NONE', *, *, #47421, .T. ) ;
#40410 = CARTESIAN_POINT ( 'NONE',  ( -339.1964088526558498, -137.3729703655831429, 58.37414404713489091 ) ) ;
#40411 = ORIENTED_EDGE ( 'NONE', *, *, #6815, .F. ) ;
#40412 = CARTESIAN_POINT ( 'NONE',  ( -332.3517673607765914, -161.4024510877913485, 45.24454186338643780 ) ) ;
#40413 = CARTESIAN_POINT ( 'NONE',  ( 69.66827051661184100, -189.7472609257535510, -40.81902153125260213 ) ) ;
#40414 = ORIENTED_EDGE ( 'NONE', *, *, #50243, .T. ) ;
#40415 = EDGE_CURVE ( 'NONE', #4396, #13513, #12818, .T. ) ;
#40417 = LINE ( 'NONE', #12310, #18293 ) ;
#40416 = FACE_OUTER_BOUND ( 'NONE', #50988, .T. ) ;
#40418 = ORIENTED_EDGE ( 'NONE', *, *, #3817, .F. ) ;
#40419 = VECTOR ( 'NONE', #14044, 1000.000000000000114 ) ;
#40420 = ADVANCED_FACE ( 'NONE', ( #15800 ), #42849, .F. ) ;
#40421 = ORIENTED_EDGE ( 'NONE', *, *, #49529, .T. ) ;
#40422 = LINE ( 'NONE', #20208, #24545 ) ;
#40424 = CIRCLE ( 'NONE', #7690, 13.99999999999998934 ) ;
#40423 = DIRECTION ( 'NONE',  ( -0.000000000000000000, 1.000000000000000000, -0.000000000000000000 ) ) ;
#40425 = EDGE_CURVE ( 'NONE', #20084, #26704, #31535, .T. ) ;
#40426 = CARTESIAN_POINT ( 'NONE',  ( -330.4913330509368166, -108.8949048983204904, 57.16590939599316812 ) ) ;
#40427 = DIRECTION ( 'NONE',  ( 0.000000000000000000, 0.000000000000000000, 1.000000000000000000 ) ) ;
#40428 = CARTESIAN_POINT ( 'NONE',  ( 4.298610786024391605E-15, 20.00000000000000000, -41.00000000000000711 ) ) ;
#40429 = DIRECTION ( 'NONE',  ( 0.000000000000000000, -1.000000000000000000, 0.000000000000000000 ) ) ;
#40430 = EDGE_CURVE ( 'NONE', #49256, #39057, #23411, .T. ) ;
#40431 = ORIENTED_EDGE ( 'NONE', *, *, #13811, .F. ) ;
#40432 = CARTESIAN_POINT ( 'NONE',  ( -339.1964088526558498, -145.2430625708876732, -55.92172413327814695 ) ) ;
#40433 = DIRECTION ( 'NONE',  ( 0.000000000000000000, 0.9350162426854146114, -0.3546048870425363986 ) ) ;
#40434 = DIRECTION ( 'NONE',  ( -0.000000000000000000, -1.000000000000000000, 0.000000000000000000 ) ) ;
#40435 = EDGE_CURVE ( 'NONE', #13544, #26773, #27072, .T. ) ;
#40436 = DIRECTION ( 'NONE',  ( 0.000000000000000000, 1.000000000000000000, -0.000000000000000000 ) ) ;
#40437 = ORIENTED_EDGE ( 'NONE', *, *, #6366, .F. ) ;
#40438 = CARTESIAN_POINT ( 'NONE',  ( -48.47912675150885065, -187.5000000000000284, 6.938893903907228378E-15 ) ) ;
#40439 = VECTOR ( 'NONE', #47305, 1000.000000000000000 ) ;
#40440 = CARTESIAN_POINT ( 'NONE',  ( -172.1341525481710164, -175.3837268820161057, 18.28755301364338237 ) ) ;
#40441 = DIRECTION ( 'NONE',  ( -8.718379230999705894E-17, -0.1205366802553303057, -0.9927088740980530845 ) ) ;
#40442 = ORIENTED_EDGE ( 'NONE', *, *, #13435, .F. ) ;
#40443 = ORIENTED_EDGE ( 'NONE', *, *, #10403, .T. ) ;
#40444 = VECTOR ( 'NONE', #43999, 1000.000000000000000 ) ;
#40445 = EDGE_LOOP ( 'NONE', ( #30028, #13618, #8675, #34701 ) ) ;
#40446 = EDGE_CURVE ( 'NONE', #27774, #6375, #15019, .T. ) ;
#40447 = VECTOR ( 'NONE', #43885, 1000.000000000000227 ) ;
#40448 = ADVANCED_FACE ( 'NONE', ( #43108 ), #18942, .T. ) ;
#40449 = PLANE ( 'NONE',  #25924 ) ;
#40450 = DIRECTION ( 'NONE',  ( 0.000000000000000000, 0.000000000000000000, 1.000000000000000000 ) ) ;
#40451 = CARTESIAN_POINT ( 'NONE',  ( -155.4121128832437364, -177.1207230881787780, -62.78108192021941392 ) ) ;
#40452 = DIRECTION ( 'NONE',  ( 0.4031234292879665171, 0.000000000000000000, 0.9151456172430210145 ) ) ;
#40453 = ORIENTED_EDGE ( 'NONE', *, *, #24963, .F. ) ;
#40454 = LINE ( 'NONE', #20490, #36704 ) ;
#40455 = DIRECTION ( 'NONE',  ( 0.000000000000000000, 1.000000000000000000, 0.000000000000000000 ) ) ;
#40456 = VECTOR ( 'NONE', #18946, 1000.000000000000000 ) ;
#40457 = ORIENTED_EDGE ( 'NONE', *, *, #37566, .F. ) ;
#40458 = VERTEX_POINT ( 'NONE', #43382 ) ;
#40459 = AXIS2_PLACEMENT_3D ( 'NONE', #40077, #51666, #9266 ) ;
#40460 = VECTOR ( 'NONE', #19104, 1000.000000000000000 ) ;
#40461 = ORIENTED_EDGE ( 'NONE', *, *, #34906, .F. ) ;
#40462 = DIRECTION ( 'NONE',  ( 0.6965510290629932655, 0.000000000000000000, 0.7175072570443347120 ) ) ;
#40463 = EDGE_CURVE ( 'NONE', #24385, #34100, #50581, .T. ) ;
#40464 = EDGE_CURVE ( 'NONE', #30731, #37301, #7763, .T. ) ;
#40465 = ADVANCED_FACE ( 'NONE', ( #27601, #43631, #31020 ), #7629, .F. ) ;
#40466 = ADVANCED_FACE ( 'NONE', ( #27071 ), #7117, .F. ) ;
#40467 = CARTESIAN_POINT ( 'NONE',  ( 75.60865171534658202, -193.5000000000000000, -15.07392567185468124 ) ) ;
#40468 = PLANE ( 'NONE',  #50428 ) ;
#40471 = ORIENTED_EDGE ( 'NONE', *, *, #32362, .F. ) ;
#40470 = DIRECTION ( 'NONE',  ( -0.000000000000000000, 1.000000000000000000, 0.000000000000000000 ) ) ;
#40469 = DIRECTION ( 'NONE',  ( -0.4827922027307551267, 0.000000000000000000, 0.8757349421956311941 ) ) ;
#40472 = DIRECTION ( 'NONE',  ( -0.000000000000000000, 0.3546048870425363986, 0.9350162426854146114 ) ) ;
#40473 = VERTEX_POINT ( 'NONE', #3676 ) ;
#40474 = CARTESIAN_POINT ( 'NONE',  ( -11.80936624585914707, -175.3837268820161057, -119.5003291395395735 ) ) ;
#40475 = VECTOR ( 'NONE', #32556, 1000.000000000000000 ) ;
#40476 = FACE_OUTER_BOUND ( 'NONE', #21167, .T. ) ;
#40477 = ORIENTED_EDGE ( 'NONE', *, *, #48436, .T. ) ;
#40478 = DIRECTION ( 'NONE',  ( 0.000000000000000000, -1.000000000000000000, 0.000000000000000000 ) ) ;
#40479 = CARTESIAN_POINT ( 'NONE',  ( -140.0851925571752474, -175.3837268820161057, 83.57229767764225414 ) ) ;
#40481 = CARTESIAN_POINT ( 'NONE',  ( 26.62880456707183896, -189.7472609257535510, 98.66508442481513441 ) ) ;
#40480 = CARTESIAN_POINT ( 'NONE',  ( -330.4913330509368166, -182.5000000000000568, 0.4999999999999549249 ) ) ;
#40482 = VERTEX_POINT ( 'NONE', #27846 ) ;
#40483 = AXIS2_PLACEMENT_3D ( 'NONE', #48632, #21018, #17355 ) ;
#40484 = PLANE ( 'NONE',  #39921 ) ;
#40485 = CARTESIAN_POINT ( 'NONE',  ( 60.90550954139435902, -193.5000000000000000, 60.49794494914085874 ) ) ;
#40486 = LINE ( 'NONE', #11612, #20831 ) ;
#40487 = ORIENTED_EDGE ( 'NONE', *, *, #17818, .F. ) ;
#40488 = DIRECTION ( 'NONE',  ( 0.000000000000000000, -1.000000000000000000, 0.000000000000000000 ) ) ;
#40489 = DIRECTION ( 'NONE',  ( 0.000000000000000000, -0.6631226582407965253, -0.7485107481711000821 ) ) ;
#40490 = DIRECTION ( 'NONE',  ( 0.000000000000000000, 1.000000000000000000, 0.000000000000000000 ) ) ;
#40491 = VERTEX_POINT ( 'NONE', #43883 ) ;
#40492 = DIRECTION ( 'NONE',  ( 0.000000000000000000, -1.000000000000000000, 0.000000000000000000 ) ) ;
#40493 = AXIS2_PLACEMENT_3D ( 'NONE', #19649, #20169, #3892 ) ;
#40495 = AXIS2_PLACEMENT_3D ( 'NONE', #47695, #15371, #31379 ) ;
#40494 = DIRECTION ( 'NONE',  ( 0.000000000000000000, 0.000000000000000000, -1.000000000000000000 ) ) ;
#40496 = EDGE_CURVE ( 'NONE', #23459, #51539, #7878, .T. ) ;
#40497 = ORIENTED_EDGE ( 'NONE', *, *, #43916, .T. ) ;
#40498 = DIRECTION ( 'NONE',  ( 0.9960498426152171181, 0.000000000000000000, -0.08879589532293157006 ) ) ;
#40499 = ORIENTED_EDGE ( 'NONE', *, *, #12417, .T. ) ;
#40500 = CIRCLE ( 'NONE', #47248, 124.9999999999999858 ) ;
#40501 = AXIS2_PLACEMENT_3D ( 'NONE', #38454, #14818, #50039 ) ;
#40502 = DIRECTION ( 'NONE',  ( -0.000000000000000000, 1.000000000000000000, 0.000000000000000000 ) ) ;
#40503 = DIRECTION ( 'NONE',  ( 1.000000000000000000, 0.000000000000000000, -0.000000000000000000 ) ) ;
#40504 = CARTESIAN_POINT ( 'NONE',  ( -336.3521761649654422, -179.5993808087905279, -18.46045550523168899 ) ) ;
#40505 = PLANE ( 'NONE',  #26419 ) ;
#40506 = DIRECTION ( 'NONE',  ( 0.000000000000000000, 1.000000000000000000, -0.000000000000000000 ) ) ;
#40507 = DIRECTION ( 'NONE',  ( -0.000000000000000000, 1.000000000000000000, -0.000000000000000000 ) ) ;
#40508 = DIRECTION ( 'NONE',  ( -0.000000000000000000, -0.3546048870425396182, -0.9350162426854132791 ) ) ;
#40509 = CARTESIAN_POINT ( 'NONE',  ( -339.1964088526558498, -162.9984922102927385, -43.83057281297435992 ) ) ;
#40511 = ORIENTED_EDGE ( 'NONE', *, *, #2099, .F. ) ;
#40510 = LINE ( 'NONE', #62, #1829 ) ;
#40512 = VECTOR ( 'NONE', #36170, 1000.000000000000000 ) ;
#40513 = ORIENTED_EDGE ( 'NONE', *, *, #16048, .F. ) ;
#40514 = DIRECTION ( 'NONE',  ( -0.9027978299657477557, 0.000000000000000000, 0.4300652022765115712 ) ) ;
#40515 = VECTOR ( 'NONE', #42143, 1000.000000000000000 ) ;
#40516 = DIRECTION ( 'NONE',  ( 0.4031234292879665171, 0.000000000000000000, 0.9151456172430210145 ) ) ;
#40517 = ORIENTED_EDGE ( 'NONE', *, *, #46422, .F. ) ;
#40518 = ORIENTED_EDGE ( 'NONE', *, *, #31900, .T. ) ;
#40519 = ORIENTED_EDGE ( 'NONE', *, *, #35981, .F. ) ;
#40520 = DIRECTION ( 'NONE',  ( -0.8455960035018272869, 0.000000000000000000, 0.5338233779647886257 ) ) ;
#40521 = EDGE_CURVE ( 'NONE', #42748, #50890, #30767, .T. ) ;
#40522 = PLANE ( 'NONE',  #26966 ) ;
#40523 = DIRECTION ( 'NONE',  ( -1.000000000000000000, 0.000000000000000000, 0.000000000000000000 ) ) ;
#40525 = ORIENTED_EDGE ( 'NONE', *, *, #20358, .F. ) ;
#40524 = AXIS2_PLACEMENT_3D ( 'NONE', #4456, #21007, #40967 ) ;
#40526 = VECTOR ( 'NONE', #42204, 1000.000000000000000 ) ;
#40527 = EDGE_LOOP ( 'NONE', ( #38526, #5779, #3116, #24256 ) ) ;
#40528 = ORIENTED_EDGE ( 'NONE', *, *, #37465, .F. ) ;
#40529 = LINE ( 'NONE', #20306, #19085 ) ;
#40530 = LINE ( 'NONE', #20571, #26872 ) ;
#40532 = ORIENTED_EDGE ( 'NONE', *, *, #5334, .F. ) ;
#40531 = DIRECTION ( 'NONE',  ( -0.000000000000000000, 1.047444401652940007E-14, 1.000000000000000000 ) ) ;
#40533 = AXIS2_PLACEMENT_3D ( 'NONE', #26049, #49717, #1876 ) ;
#40534 = DIRECTION ( 'NONE',  ( 0.000000000000000000, 0.4647231720437631775, -0.8854560256532126861 ) ) ;
#40535 = DIRECTION ( 'NONE',  ( 0.000000000000000000, 0.000000000000000000, -1.000000000000000000 ) ) ;
#40536 = ORIENTED_EDGE ( 'NONE', *, *, #27247, .F. ) ;
#40537 = DIRECTION ( 'NONE',  ( 0.000000000000000000, 0.000000000000000000, -1.000000000000000000 ) ) ;
#40538 = VECTOR ( 'NONE', #46676, 1000.000000000000114 ) ;
#40539 = LINE ( 'NONE', #4557, #31642 ) ;
#40540 = DIRECTION ( 'NONE',  ( -0.000000000000000000, 1.000000000000000000, -0.000000000000000000 ) ) ;
#40541 = FACE_OUTER_BOUND ( 'NONE', #33630, .T. ) ;
#40542 = ORIENTED_EDGE ( 'NONE', *, *, #40767, .T. ) ;
#40543 = VERTEX_POINT ( 'NONE', #25383 ) ;
#40544 = CARTESIAN_POINT ( 'NONE',  ( -127.0132498732365889, -177.1207230881787780, 97.24912084693261249 ) ) ;
#40545 = DIRECTION ( 'NONE',  ( -0.000000000000000000, 1.000000000000000000, -0.000000000000000000 ) ) ;
#40546 = ORIENTED_EDGE ( 'NONE', *, *, #44767, .T. ) ;
#40547 = EDGE_CURVE ( 'NONE', #39299, #3275, #9102, .T. ) ;
#40548 = LINE ( 'NONE', #16144, #24029 ) ;
#40549 = CIRCLE ( 'NONE', #32158, 125.0000000000000000 ) ;
#40550 = CARTESIAN_POINT ( 'NONE',  ( -47.57632892154310866, -189.7472609257535510, -0.4300652022765113491 ) ) ;
#40551 = VERTEX_POINT ( 'NONE', #13297 ) ;
#40552 = CARTESIAN_POINT ( 'NONE',  ( 0.000000000000000000, -144.4216883355091170, 55.16595831843969933 ) ) ;
#40554 = AXIS2_PLACEMENT_3D ( 'NONE', #2134, #38912, #26570 ) ;
#40553 = CARTESIAN_POINT ( 'NONE',  ( -330.4913330509368166, -79.00630452878421295, 38.74998146212088557 ) ) ;
#40555 = ORIENTED_EDGE ( 'NONE', *, *, #44788, .F. ) ;
#40556 = CARTESIAN_POINT ( 'NONE',  ( 14.94072793302542124, -193.5000000000000000, 107.7168604805791574 ) ) ;
#40557 = ORIENTED_EDGE ( 'NONE', *, *, #45451, .T. ) ;
#40558 = FACE_OUTER_BOUND ( 'NONE', #51162, .T. ) ;
#40559 = EDGE_CURVE ( 'NONE', #34133, #19374, #5273, .T. ) ;
#40560 = VERTEX_POINT ( 'NONE', #21178 ) ;
#40561 = CARTESIAN_POINT ( 'NONE',  ( -48.59739992243022755, -177.1207230881787780, 0.9929810960135230236 ) ) ;
#40562 = CARTESIAN_POINT ( 'NONE',  ( -95.18697522258266019, -177.1207230881787780, 115.9455772817713353 ) ) ;
#40563 = DIRECTION ( 'NONE',  ( -0.000000000000000000, 1.000000000000000000, -0.000000000000000000 ) ) ;
#40564 = EDGE_CURVE ( 'NONE', #41391, #11859, #32990, .T. ) ;
#40565 = CIRCLE ( 'NONE', #7012, 125.0000000000000000 ) ;
#40566 = DIRECTION ( 'NONE',  ( 0.000000000000000000, -1.000000000000000000, -0.000000000000000000 ) ) ;
#40567 = ORIENTED_EDGE ( 'NONE', *, *, #24891, .F. ) ;
#40568 = CARTESIAN_POINT ( 'NONE',  ( -48.47912675150885065, -175.3837268820161057, 6.938893903907228378E-15 ) ) ;
#40569 = EDGE_LOOP ( 'NONE', ( #29811, #30476, #16417, #18561 ) ) ;
#40570 = ORIENTED_EDGE ( 'NONE', *, *, #26241, .F. ) ;
#40571 = CIRCLE ( 'NONE', #45636, 125.0000000000000000 ) ;
#40572 = LINE ( 'NONE', #12204, #8496 ) ;
#40574 = VERTEX_POINT ( 'NONE', #49040 ) ;
#40573 = CARTESIAN_POINT ( 'NONE',  ( 73.50869128264329788, -193.5000000000000000, -22.25084316132035056 ) ) ;
#40575 = ORIENTED_EDGE ( 'NONE', *, *, #37755, .F. ) ;
#40576 = CARTESIAN_POINT ( 'NONE',  ( -47.70260288879081401, -175.3837268820161057, 0.6300878435817218737 ) ) ;
#40577 = ADVANCED_FACE ( 'NONE', ( #9357 ), #13023, .T. ) ;
#40578 = DIRECTION ( 'NONE',  ( 0.7575112421616145841, 0.000000000000000000, 0.6528221181905280446 ) ) ;
#40579 = ORIENTED_EDGE ( 'NONE', *, *, #28380, .F. ) ;
#40580 = CARTESIAN_POINT ( 'NONE',  ( -134.9734323446613189, -193.5000000000000000, 88.85232316304893629 ) ) ;
#40581 = ORIENTED_EDGE ( 'NONE', *, *, #6108, .F. ) ;
#40582 = DIRECTION ( 'NONE',  ( -0.8455960035018199594, 0.000000000000000000, -0.5338233779648003940 ) ) ;
#40583 = CARTESIAN_POINT ( 'NONE',  ( -172.0839188101925004, -175.3837268820161057, -18.62405380494756812 ) ) ;
#40584 = CIRCLE ( 'NONE', #15448, 125.0000000000000000 ) ;
#40585 = EDGE_CURVE ( 'NONE', #16507, #27859, #37930, .T. ) ;
#40586 = DIRECTION ( 'NONE',  ( -0.000000000000000000, -0.2393156642875482742, 0.9709418174260544543 ) ) ;
#40587 = DIRECTION ( 'NONE',  ( 0.000000000000000000, 0.000000000000000000, 1.000000000000000000 ) ) ;
#40588 = EDGE_LOOP ( 'NONE', ( #40240, #11127, #43612, #40 ) ) ;
#40589 = ORIENTED_EDGE ( 'NONE', *, *, #3341, .F. ) ;
#40590 = ADVANCED_FACE ( 'NONE', ( #41875 ), #33205, .T. ) ;
#40591 = AXIS2_PLACEMENT_3D ( 'NONE', #6537, #30424, #46731 ) ;
#40592 = ORIENTED_EDGE ( 'NONE', *, *, #11802, .F. ) ;
#40593 = CARTESIAN_POINT ( 'NONE',  ( -332.3517673607765914, -110.9652333097088217, -57.67619951860654481 ) ) ;
#40594 = CARTESIAN_POINT ( 'NONE',  ( -169.2746641285359317, -189.7472609257535510, -32.14713283941905786 ) ) ;
#40595 = ADVANCED_FACE ( 'NONE', ( #1411 ), #25849, .T. ) ;
#40596 = CARTESIAN_POINT ( 'NONE',  ( 2.449293598294706119E-15, -63.50000000000000000, -20.00000000000000000 ) ) ;
#40597 = FACE_BOUND ( 'NONE', #34636, .T. ) ;
#40598 = DIRECTION ( 'NONE',  ( 0.000000000000000000, -0.5680647467311485954, 0.8229838658936613482 ) ) ;
#40599 = ORIENTED_EDGE ( 'NONE', *, *, #22902, .F. ) ;
#40600 = VECTOR ( 'NONE', #1767, 1000.000000000000000 ) ;
#40601 = ORIENTED_EDGE ( 'NONE', *, *, #8613, .F. ) ;
#40603 = ORIENTED_EDGE ( 'NONE', *, *, #30622, .F. ) ;
#40602 = CARTESIAN_POINT ( 'NONE',  ( -339.1964088526558498, -167.9936954712156592, -38.74998146212110584 ) ) ;
#40604 = ORIENTED_EDGE ( 'NONE', *, *, #12465, .T. ) ;
#40605 = DIRECTION ( 'NONE',  ( 0.000000000000000000, 0.000000000000000000, 1.000000000000000000 ) ) ;
#40606 = EDGE_CURVE ( 'NONE', #15472, #43725, #44723, .T. ) ;
#40607 = LINE ( 'NONE', #8317, #19940 ) ;
#40608 = DIRECTION ( 'NONE',  ( 0.000000000000000000, 7.100801428331730794E-14, -1.000000000000000000 ) ) ;
#40609 = CARTESIAN_POINT ( 'NONE',  ( -38.66762320617017679, -177.1207230881787780, -124.6143426664033740 ) ) ;
#40610 = ORIENTED_EDGE ( 'NONE', *, *, #35090, .F. ) ;
#40611 = CARTESIAN_POINT ( 'NONE',  ( -332.3517673607765914, -181.7525362123217292, 9.724760635742144999 ) ) ;
#40612 = EDGE_LOOP ( 'NONE', ( #46057, #16427, #33626, #41337 ) ) ;
#40613 = VERTEX_POINT ( 'NONE', #25083 ) ;
#40614 = DIRECTION ( 'NONE',  ( 0.000000000000000000, -1.000000000000000000, -0.000000000000000000 ) ) ;
#40615 = CARTESIAN_POINT ( 'NONE',  ( -33.52607327456453135, -189.7472609257535510, -124.1024020384603119 ) ) ;
#40616 = FACE_OUTER_BOUND ( 'NONE', #43391, .T. ) ;
#40617 = VECTOR ( 'NONE', #37384, 1000.000000000000000 ) ;
#40618 = LINE ( 'NONE', #24606, #38195 ) ;
#40619 = AXIS2_PLACEMENT_3D ( 'NONE', #37017, #24669, #13370 ) ;
#40620 = LINE ( 'NONE', #4138, #50705 ) ;
#40621 = CARTESIAN_POINT ( 'NONE',  ( -332.3517673607765914, -181.4155151828941825, -11.56382487286496463 ) ) ;
#40622 = ORIENTED_EDGE ( 'NONE', *, *, #48204, .F. ) ;
#40623 = DIRECTION ( 'NONE',  ( 0.000000000000000000, -1.000000000000000000, 0.000000000000000000 ) ) ;
#40624 = CARTESIAN_POINT ( 'NONE',  ( -48.47912675150885065, -177.1207230881787780, 6.938893903907228378E-15 ) ) ;
#40625 = CIRCLE ( 'NONE', #21366, 125.0000000000000000 ) ;
#40626 = EDGE_CURVE ( 'NONE', #48534, #18665, #28753, .T. ) ;
#40627 = CARTESIAN_POINT ( 'NONE',  ( 60.00000000000001421, -63.50000000000000000, 0.000000000000000000 ) ) ;
#40628 = FACE_BOUND ( 'NONE', #24255, .T. ) ;
#40629 = ORIENTED_EDGE ( 'NONE', *, *, #5972, .T. ) ;
#40630 = LINE ( 'NONE', #8846, #5519 ) ;
#40631 = ORIENTED_EDGE ( 'NONE', *, *, #21636, .F. ) ;
#40632 = CARTESIAN_POINT ( 'NONE',  ( -145.4373324222574126, -175.3837268820161057, -78.89300572996837957 ) ) ;
#40633 = EDGE_CURVE ( 'NONE', #21155, #38288, #33485, .T. ) ;
#40634 = ORIENTED_EDGE ( 'NONE', *, *, #22236, .F. ) ;
#40635 = EDGE_CURVE ( 'NONE', #26640, #11081, #46098, .T. ) ;
#40636 = DIRECTION ( 'NONE',  ( 0.000000000000000000, 0.000000000000000000, -1.000000000000000000 ) ) ;
#40637 = AXIS2_PLACEMENT_3D ( 'NONE', #21166, #8548, #37446 ) ;
#40638 = ORIENTED_EDGE ( 'NONE', *, *, #11245, .T. ) ;
#40639 = DIRECTION ( 'NONE',  ( 0.000000000000000000, -0.000000000000000000, -1.000000000000000000 ) ) ;
#40640 = DIRECTION ( 'NONE',  ( -0.000000000000000000, 1.000000000000000000, -0.000000000000000000 ) ) ;
#40642 = VERTEX_POINT ( 'NONE', #29267 ) ;
#40641 = DIRECTION ( 'NONE',  ( -1.000000000000000000, 0.000000000000000000, 0.000000000000000000 ) ) ;
#40643 = EDGE_CURVE ( 'NONE', #51592, #28874, #5110, .T. ) ;
#40644 = LINE ( 'NONE', #4668, #39454 ) ;
#40645 = ORIENTED_EDGE ( 'NONE', *, *, #31099, .F. ) ;
#40646 = ADVANCED_FACE ( 'NONE', ( #9557 ), #28990, .T. ) ;
#40647 = EDGE_LOOP ( 'NONE', ( #5489, #29682, #40622, #7960 ) ) ;
#40648 = CARTESIAN_POINT ( 'NONE',  ( 59.70893145360470555, -175.3837268820161057, -60.59166255800331413 ) ) ;
#40649 = ADVANCED_FACE ( 'NONE', ( #41602 ), #25329, .T. ) ;
#40650 = ORIENTED_EDGE ( 'NONE', *, *, #26559, .F. ) ;
#40651 = CARTESIAN_POINT ( 'NONE',  ( 62.13187335169531167, -183.6283474603465606, -58.22548115875872554 ) ) ;
#40652 = VECTOR ( 'NONE', #17113, 1000.000000000000000 ) ;
#40653 = CARTESIAN_POINT ( 'NONE',  ( -33.86391487983340909, -189.7472609257535510, 124.1426420773540684 ) ) ;
#40654 = DIRECTION ( 'NONE',  ( 0.000000000000000000, 0.000000000000000000, -1.000000000000000000 ) ) ;
#40655 = EDGE_CURVE ( 'NONE', #18230, #7739, #5365, .T. ) ;
#40656 = CIRCLE ( 'NONE', #37302, 125.0000000000000000 ) ;
#40657 = AXIS2_PLACEMENT_3D ( 'NONE', #19139, #51210, #7309 ) ;
#40658 = FACE_OUTER_BOUND ( 'NONE', #43655, .T. ) ;
#40659 = DIRECTION ( 'NONE',  ( 0.000000000000000000, 0.000000000000000000, -1.000000000000000000 ) ) ;
#40660 = ORIENTED_EDGE ( 'NONE', *, *, #43785, .F. ) ;
#40663 = ORIENTED_EDGE ( 'NONE', *, *, #29590, .T. ) ;
#40662 = PLANE ( 'NONE',  #25602 ) ;
#40661 = DIRECTION ( 'NONE',  ( -1.000000000000000000, 0.000000000000000000, 0.000000000000000000 ) ) ;
#40664 = ORIENTED_EDGE ( 'NONE', *, *, #2585, .F. ) ;
#40665 = AXIS2_PLACEMENT_3D ( 'NONE', #43332, #2613, #3382 ) ;
#40666 = DIRECTION ( 'NONE',  ( 0.000000000000000000, -0.9350162426854169428, -0.3546048870425300148 ) ) ;
#40667 = ORIENTED_EDGE ( 'NONE', *, *, #42031, .T. ) ;
#40668 = DIRECTION ( 'NONE',  ( -0.000000000000000000, 0.000000000000000000, 1.000000000000000000 ) ) ;
#40669 = ORIENTED_EDGE ( 'NONE', *, *, #10006, .F. ) ;
#40670 = LINE ( 'NONE', #16799, #12022 ) ;
#40671 = CARTESIAN_POINT ( 'NONE',  ( -49.08592689732745384, -183.6283474603465606, 0.7948544414133550395 ) ) ;
#40672 = ORIENTED_EDGE ( 'NONE', *, *, #21997, .T. ) ;
#40674 = CARTESIAN_POINT ( 'NONE',  ( -21.64528618042744412, -183.6283474603465606, 121.0625654437174887 ) ) ;
#40673 = CARTESIAN_POINT ( 'NONE',  ( 46.00000000000000711, 20.00000000000000000, -46.00000000000000000 ) ) ;
#40675 = AXIS2_PLACEMENT_3D ( 'NONE', #1114, #863, #49502 ) ;
#40676 = ORIENTED_EDGE ( 'NONE', *, *, #17202, .F. ) ;
#40677 = ORIENTED_EDGE ( 'NONE', *, *, #27666, .T. ) ;
#40678 = PLANE ( 'NONE',  #31257 ) ;
#40679 = CARTESIAN_POINT ( 'NONE',  ( 73.03012110230136500, -175.3837268820161057, 24.72869175143112130 ) ) ;
#40680 = FACE_OUTER_BOUND ( 'NONE', #40159, .T. ) ;
#40681 = PLANE ( 'NONE',  #2333 ) ;
#40682 = LINE ( 'NONE', #19957, #4796 ) ;
#40683 = DIRECTION ( 'NONE',  ( -0.000000000000000000, -0.7485107481710953081, 0.6631226582408016323 ) ) ;
#40684 = APPLICATION_PROTOCOL_DEFINITION ( 'draft international standard', 'automotive_design', 1998, #13556 ) ;
#40685 = DIRECTION ( 'NONE',  ( 0.000000000000000000, 0.9350162426854194964, 0.3546048870425235200 ) ) ;
#40686 = DIRECTION ( 'NONE',  ( -0.000000000000000000, 1.047444401652940007E-14, 1.000000000000000000 ) ) ;
#40687 = LINE ( 'NONE', #37798, #14765 ) ;
#40688 = PLANE ( 'NONE',  #42221 ) ;
#40689 = ORIENTED_EDGE ( 'NONE', *, *, #43507, .F. ) ;
#40690 = VERTEX_POINT ( 'NONE', #37407 ) ;
#40691 = AXIS2_PLACEMENT_3D ( 'NONE', #23570, #39341, #8504 ) ;
#40692 = PLANE ( 'NONE',  #45009 ) ;
#40693 = EDGE_CURVE ( 'NONE', #47251, #24620, #17467, .T. ) ;
#40694 = VECTOR ( 'NONE', #29372, 1000.000000000000000 ) ;
#40695 = AXIS2_PLACEMENT_3D ( 'NONE', #3601, #7803, #44342 ) ;
#40696 = ADVANCED_FACE ( 'NONE', ( #13762 ), #50813, .T. ) ;
#40697 = CARTESIAN_POINT ( 'NONE',  ( -330.4913330509368166, -109.8658467157472813, -57.40522506028090532 ) ) ;
#40698 = CARTESIAN_POINT ( 'NONE',  ( 66.11593792271145276, -175.3837268820161057, -47.37063079638321739 ) ) ;
#40699 = ADVANCED_FACE ( 'NONE', ( #25858 ), #30560, .F. ) ;
#40700 = VERTEX_POINT ( 'NONE', #6415 ) ;
#40701 = EDGE_CURVE ( 'NONE', #48252, #30276, #14555, .T. ) ;
#40702 = ORIENTED_EDGE ( 'NONE', *, *, #50629, .F. ) ;
#40703 = ORIENTED_EDGE ( 'NONE', *, *, #27879, .F. ) ;
#40704 = EDGE_CURVE ( 'NONE', #12031, #2659, #10342, .T. ) ;
#40705 = CARTESIAN_POINT ( 'NONE',  ( 76.51419089073348800, -177.1207230881787780, -1.292495564988658030 ) ) ;
#40706 = ADVANCED_FACE ( 'NONE', ( #18237 ), #22692, .F. ) ;
#40707 = LINE ( 'NONE', #8408, #13598 ) ;
#40708 = CIRCLE ( 'NONE', #8011, 125.0000000000000000 ) ;
#40709 = LINE ( 'NONE', #28625, #37155 ) ;
#40710 = DIRECTION ( 'NONE',  ( 0.000000000000000000, 0.000000000000000000, -1.000000000000000000 ) ) ;
#40711 = VECTOR ( 'NONE', #11647, 1000.000000000000000 ) ;
#40712 = VERTEX_POINT ( 'NONE', #21918 ) ;
#40713 = DIRECTION ( 'NONE',  ( -0.000000000000000000, 1.000000000000000000, -0.000000000000000000 ) ) ;
#40714 = EDGE_CURVE ( 'NONE', #49553, #17248, #6135, .T. ) ;
#40715 = AXIS2_PLACEMENT_3D ( 'NONE', #24721, #44695, #8174 ) ;
#40716 = FACE_OUTER_BOUND ( 'NONE', #42778, .T. ) ;
#40717 = ORIENTED_EDGE ( 'NONE', *, *, #22482, .T. ) ;
#40718 = EDGE_CURVE ( 'NONE', #6765, #41945, #18748, .T. ) ;
#40719 = CARTESIAN_POINT ( 'NONE',  ( 67.42090074966655777, -193.5000000000000000, -46.82076062204441058 ) ) ;
#40720 = EDGE_LOOP ( 'NONE', ( #30579, #50818 ) ) ;
#40721 = VECTOR ( 'NONE', #47541, 1000.000000000000000 ) ;
#40722 = ADVANCED_FACE ( 'NONE', ( #34258 ), #37941, .T. ) ;
#40723 = ORIENTED_EDGE ( 'NONE', *, *, #45278, .F. ) ;
#40724 = CARTESIAN_POINT ( 'NONE',  ( -170.0000000000000284, -123.5000000000000284, 0.000000000000000000 ) ) ;
#40725 = EDGE_CURVE ( 'NONE', #2935, #22714, #1942, .T. ) ;
#40726 = EDGE_CURVE ( 'NONE', #30974, #1806, #24565, .T. ) ;
#40727 = DIRECTION ( 'NONE',  ( -1.000000000000000000, -0.000000000000000000, -0.000000000000000000 ) ) ;
#40728 = CARTESIAN_POINT ( 'NONE',  ( -170.0000000000000284, -115.7896721143442278, -60.00000000000000711 ) ) ;
#40731 = ORIENTED_EDGE ( 'NONE', *, *, #43785, .T. ) ;
#40730 = DIRECTION ( 'NONE',  ( 0.4639789333096864810, 0.000000000000000000, -0.8858462335218260097 ) ) ;
#40729 = CARTESIAN_POINT ( 'NONE',  ( -47.50057025920934706, -177.1207230881787780, -0.2059786187410884151 ) ) ;
#40732 = AXIS2_PLACEMENT_3D ( 'NONE', #34493, #35016, #14541 ) ;
#40733 = CARTESIAN_POINT ( 'NONE',  ( -48.47912675150885065, -175.3837268820161057, 6.938893903907228378E-15 ) ) ;
#40734 = VECTOR ( 'NONE', #3219, 1000.000000000000000 ) ;
#40735 = ORIENTED_EDGE ( 'NONE', *, *, #22114, .F. ) ;
#40736 = CARTESIAN_POINT ( 'NONE',  ( 62.59443091842027940, -177.1207230881787780, -57.33816169485140790 ) ) ;
#40737 = DIRECTION ( 'NONE',  ( 0.000000000000000000, -0.000000000000000000, 1.000000000000000000 ) ) ;
#40738 = EDGE_LOOP ( 'NONE', ( #43771, #39256, #29919, #8893 ) ) ;
#40739 = VECTOR ( 'NONE', #13702, 999.9999999999998863 ) ;
#40740 = FACE_OUTER_BOUND ( 'NONE', #10493, .T. ) ;
#40742 = CARTESIAN_POINT ( 'NONE',  ( -166.8403286750647680, -189.7472609257535510, -40.19484891389974734 ) ) ;
#40741 = CARTESIAN_POINT ( 'NONE',  ( 61.98524708613674505, -183.6283474603465606, 56.33604425924833237 ) ) ;
#40743 = EDGE_CURVE ( 'NONE', #49730, #7246, #48931, .T. ) ;
#40744 = ORIENTED_EDGE ( 'NONE', *, *, #14766, .T. ) ;
#40745 = DIRECTION ( 'NONE',  ( -0.9785564922995046988, 0.000000000000000000, 0.2059786187410953262 ) ) ;
#40746 = DIRECTION ( 'NONE',  ( 0.000000000000000000, 0.000000000000000000, -1.000000000000000000 ) ) ;
#40747 = DIRECTION ( 'NONE',  ( -0.000000000000000000, -0.9350162426854158326, -0.3546048870425331234 ) ) ;
#40748 = ORIENTED_EDGE ( 'NONE', *, *, #8285, .T. ) ;
#40749 = DIRECTION ( 'NONE',  ( -0.6749830015182091136, 0.000000000000000000, -0.7378332790417285736 ) ) ;
#40750 = DIRECTION ( 'NONE',  ( -0.000000000000000000, -0.2393156642875615969, -0.9709418174260511236 ) ) ;
#40751 = VECTOR ( 'NONE', #41156, 1000.000000000000114 ) ;
#40752 = LINE ( 'NONE', #16615, #23209 ) ;
#40753 = EDGE_LOOP ( 'NONE', ( #49170, #14584, #27898, #13087 ) ) ;
#40754 = VECTOR ( 'NONE', #16078, 1000.000000000000227 ) ;
#40755 = DIRECTION ( 'NONE',  ( 0.000000000000000000, 1.000000000000000000, 0.000000000000000000 ) ) ;
#40756 = VECTOR ( 'NONE', #41190, 1000.000000000000114 ) ;
#40757 = EDGE_CURVE ( 'NONE', #26962, #36738, #22440, .T. ) ;
#40758 = VERTEX_POINT ( 'NONE', #26633 ) ;
#40759 = CARTESIAN_POINT ( 'NONE',  ( 0.000000000000000000, -172.0560480877254861, 33.51582005713859758 ) ) ;
#40760 = ORIENTED_EDGE ( 'NONE', *, *, #19596, .T. ) ;
#40761 = DIRECTION ( 'NONE',  ( -1.000000000000000000, -0.000000000000000000, -0.000000000000000000 ) ) ;
#40762 = CARTESIAN_POINT ( 'NONE',  ( -149.5539421794694022, -193.5000000000000000, 73.54509967498655953 ) ) ;
#40763 = ADVANCED_FACE ( 'NONE', ( #14295 ), #13773, .T. ) ;
#40764 = DIRECTION ( 'NONE',  ( -0.9266896074318343723, 0.000000000000000000, 0.3758275821142357809 ) ) ;
#40765 = CARTESIAN_POINT ( 'NONE',  ( 33.25242634436024503, -175.3837268820161057, -94.57776286494160445 ) ) ;
#40766 = CARTESIAN_POINT ( 'NONE',  ( -336.3521761649654422, -155.6724726690323450, 49.48329383994676078 ) ) ;
#40767 = EDGE_CURVE ( 'NONE', #32626, #47580, #17982, .T. ) ;
#40768 = EDGE_CURVE ( 'NONE', #10121, #20252, #30834, .T. ) ;
#40769 = CARTESIAN_POINT ( 'NONE',  ( -72.72541169915514558, -193.5000000000000000, 121.6072260099955287 ) ) ;
#40770 = AXIS2_PLACEMENT_3D ( 'NONE', #26807, #18423, #42586 ) ;
#40771 = LINE ( 'NONE', #49202, #990 ) ;
#40772 = DIRECTION ( 'NONE',  ( 0.000000000000000000, 0.000000000000000000, 1.000000000000000000 ) ) ;
#40773 = FACE_OUTER_BOUND ( 'NONE', #496, .T. ) ;
#40774 = AXIS2_PLACEMENT_3D ( 'NONE', #45750, #37333, #9745 ) ;
#40775 = CIRCLE ( 'NONE', #14811, 125.0000000000000000 ) ;
#40776 = ORIENTED_EDGE ( 'NONE', *, *, #31033, .F. ) ;
#40777 = CARTESIAN_POINT ( 'NONE',  ( 61.22907552172956258, -193.5000000000000000, -57.79541595648221630 ) ) ;
#40778 = DIRECTION ( 'NONE',  ( 1.000000000000000000, 0.000000000000000000, 0.000000000000000000 ) ) ;
#40779 = EDGE_LOOP ( 'NONE', ( #39771, #12067 ) ) ;
#40780 = ORIENTED_EDGE ( 'NONE', *, *, #1886, .T. ) ;
#40781 = EDGE_CURVE ( 'NONE', #41973, #29433, #37688, .T. ) ;
#40782 = VECTOR ( 'NONE', #1694, 1000.000000000000000 ) ;
#40783 = ORIENTED_EDGE ( 'NONE', *, *, #30282, .F. ) ;
#40784 = LINE ( 'NONE', #33694, #42668 ) ;
#40785 = AXIS2_PLACEMENT_3D ( 'NONE', #13251, #28735, #9313 ) ;
#40786 = EDGE_CURVE ( 'NONE', #33439, #47197, #26104, .T. ) ;
#40788 = AXIS2_PLACEMENT_3D ( 'NONE', #38100, #9743, #22611 ) ;
#40787 = DIRECTION ( 'NONE',  ( -0.8124868780056863082, 0.000000000000000000, 0.5829794791144649047 ) ) ;
#40789 = DIRECTION ( 'NONE',  ( -0.000000000000000000, 1.000000000000000000, -0.000000000000000000 ) ) ;
#40790 = VERTEX_POINT ( 'NONE', #50555 ) ;
#40791 = EDGE_LOOP ( 'NONE', ( #42466, #26405, #44057, #44243 ) ) ;
#40792 = ADVANCED_FACE ( 'NONE', ( #26875 ), #31594, .F. ) ;
#40793 = VECTOR ( 'NONE', #40024, 1000.000000000000000 ) ;
#40794 = DIRECTION ( 'NONE',  ( -0.9982437317643214625, 0.000000000000000000, -0.05924062789371441901 ) ) ;
#40796 = ORIENTED_EDGE ( 'NONE', *, *, #916, .T. ) ;
#40795 = PLANE ( 'NONE',  #20771 ) ;
#40797 = CARTESIAN_POINT ( 'NONE',  ( 7.859956736328458149, -175.3837268820161057, -111.5836353223468649 ) ) ;
#40798 = DIRECTION ( 'NONE',  ( 0.000000000000000000, 0.000000000000000000, 1.000000000000000000 ) ) ;
#40799 = VERTEX_POINT ( 'NONE', #15850 ) ;
#40800 = DIRECTION ( 'NONE',  ( -0.7378332790417239107, 0.000000000000000000, -0.6749830015182142207 ) ) ;
#40801 = ORIENTED_EDGE ( 'NONE', *, *, #43214, .T. ) ;
#40802 = LINE ( 'NONE', #47930, #26577 ) ;
#40803 = DIRECTION ( 'NONE',  ( 5.399917434947259359E-17, 1.000000000000000000, -0.000000000000000000 ) ) ;
#40804 = FACE_OUTER_BOUND ( 'NONE', #34915, .T. ) ;
#40805 = ORIENTED_EDGE ( 'NONE', *, *, #9075, .F. ) ;
#40806 = VECTOR ( 'NONE', #4646, 999.9999999999998863 ) ;
#40807 = ORIENTED_EDGE ( 'NONE', *, *, #35189, .F. ) ;
#40808 = DIRECTION ( 'NONE',  ( 0.000000000000000000, 0.000000000000000000, -1.000000000000000000 ) ) ;
#40809 = VECTOR ( 'NONE', #28737, 1000.000000000000000 ) ;
#40810 = DIRECTION ( 'NONE',  ( 0.000000000000000000, 0.7485107481710977506, -0.6631226582407989678 ) ) ;
#40811 = ORIENTED_EDGE ( 'NONE', *, *, #30340, .F. ) ;
#40812 = CARTESIAN_POINT ( 'NONE',  ( -48.47912675150885065, -183.6283474603465606, 6.938893903907228378E-15 ) ) ;
#40813 = AXIS2_PLACEMENT_3D ( 'NONE', #17653, #1075, #17127 ) ;
#40814 = DIRECTION ( 'NONE',  ( -0.000000000000000000, 1.000000000000000000, -0.000000000000000000 ) ) ;
#40815 = VERTEX_POINT ( 'NONE', #2967 ) ;
#40816 = FACE_OUTER_BOUND ( 'NONE', #4172, .T. ) ;
#40817 = DIRECTION ( 'NONE',  ( 0.000000000000000000, 1.251313867337936767E-13, 1.000000000000000000 ) ) ;
#40818 = ORIENTED_EDGE ( 'NONE', *, *, #41705, .T. ) ;
#40819 = FACE_OUTER_BOUND ( 'NONE', #24048, .T. ) ;
#40820 = ORIENTED_EDGE ( 'NONE', *, *, #16642, .F. ) ;
#40821 = FACE_BOUND ( 'NONE', #45264, .T. ) ;
#40822 = VECTOR ( 'NONE', #48721, 1000.000000000000000 ) ;
#40823 = VECTOR ( 'NONE', #42306, 1000.000000000000000 ) ;
#40824 = CARTESIAN_POINT ( 'NONE',  ( -332.3517673607765914, -142.2945752170892035, 56.98038208374156000 ) ) ;
#40825 = ORIENTED_EDGE ( 'NONE', *, *, #42382, .F. ) ;
#40826 = VECTOR ( 'NONE', #49901, 999.9999999999998863 ) ;
#40827 = AXIS2_PLACEMENT_3D ( 'NONE', #9430, #45438, #5497 ) ;
#40828 = DIRECTION ( 'NONE',  ( -0.9473263538541923934, 0.000000000000000000, 0.3202698538628350744 ) ) ;
#40829 = DIRECTION ( 'NONE',  ( 0.9995608365087940150, 0.000000000000000000, 0.02963332782257007206 ) ) ;
#40830 = PLANE ( 'NONE',  #13144 ) ;
#40831 = EDGE_CURVE ( 'NONE', #7741, #3888, #34653, .T. ) ;
#40832 = ADVANCED_FACE ( 'NONE', ( #11876 ), #31863, .T. ) ;
#40833 = CIRCLE ( 'NONE', #39149, 125.0000000000000000 ) ;
#40834 = CARTESIAN_POINT ( 'NONE',  ( -336.3521761649654422, -121.8677111499054320, 59.00000000000001421 ) ) ;
#40835 = EDGE_LOOP ( 'NONE', ( #12088, #17187, #17574, #31342 ) ) ;
#40837 = VECTOR ( 'NONE', #32406, 1000.000000000000000 ) ;
#40836 = CARTESIAN_POINT ( 'NONE',  ( -112.7586829773731267, -189.7472609257535510, -107.2060569716373379 ) ) ;
#40838 = ORIENTED_EDGE ( 'NONE', *, *, #30331, .T. ) ;
#40839 = EDGE_LOOP ( 'NONE', ( #42412, #10274, #24370, #42120 ) ) ;
#40840 = DIRECTION ( 'NONE',  ( -0.8757349421956310831, 0.000000000000000000, -0.4827922027307550712 ) ) ;
#40842 = ORIENTED_EDGE ( 'NONE', *, *, #24348, .T. ) ;
#40841 = CARTESIAN_POINT ( 'NONE',  ( -49.25565061422688728, -175.3837268820161057, -0.6300878435817132139 ) ) ;
#40843 = ORIENTED_EDGE ( 'NONE', *, *, #43583, .F. ) ;
#40844 = CARTESIAN_POINT ( 'NONE',  ( -339.1964088526558498, -84.00150778970699150, 43.83057281297409702 ) ) ;
#40845 = PLANE ( 'NONE',  #795 ) ;
#40846 = AXIS2_PLACEMENT_3D ( 'NONE', #37739, #2517, #34561 ) ;
#40847 = VECTOR ( 'NONE', #647, 999.9999999999998863 ) ;
#40848 = ORIENTED_EDGE ( 'NONE', *, *, #13820, .T. ) ;
#40849 = CARTESIAN_POINT ( 'NONE',  ( -336.3521761649654422, -176.9651911376907094, -25.08789112700655721 ) ) ;
#40850 = EDGE_CURVE ( 'NONE', #9326, #21927, #6918, .T. ) ;
#40851 = ORIENTED_EDGE ( 'NONE', *, *, #38686, .F. ) ;
#40852 = CARTESIAN_POINT ( 'NONE',  ( 31.28129687248616619, -183.6283474603465606, 96.24590808611479531 ) ) ;
#40853 = FACE_OUTER_BOUND ( 'NONE', #33132, .T. ) ;
#40854 = AXIS2_PLACEMENT_3D ( 'NONE', #14303, #38965, #6163 ) ;
#40855 = DIRECTION ( 'NONE',  ( -0.000000000000000000, -1.000000000000000000, 0.000000000000000000 ) ) ;
#40856 = DIRECTION ( 'NONE',  ( 0.000000000000000000, 0.000000000000000000, 1.000000000000000000 ) ) ;
#40857 = VERTEX_POINT ( 'NONE', #32114 ) ;
#40858 = ORIENTED_EDGE ( 'NONE', *, *, #587, .F. ) ;
#40859 = EDGE_CURVE ( 'NONE', #11734, #14384, #11991, .T. ) ;
#40860 = ORIENTED_EDGE ( 'NONE', *, *, #45942, .T. ) ;
#40861 = DIRECTION ( 'NONE',  ( -0.000000000000000000, -0.8229838658936575735, -0.5680647467311540355 ) ) ;
#40862 = DIRECTION ( 'NONE',  ( 0.9151456172430153524, 0.000000000000000000, 0.4031234292879792847 ) ) ;
#40863 = AXIS2_PLACEMENT_3D ( 'NONE', #37440, #8804, #41129 ) ;
#40864 = VECTOR ( 'NONE', #15877, 1000.000000000000000 ) ;
#40865 = CARTESIAN_POINT ( 'NONE',  ( -490.0000000000001137, -78.50000000000002842, -14.36509618646847386 ) ) ;
#40866 = VECTOR ( 'NONE', #31565, 1000.000000000000000 ) ;
#40868 = VECTOR ( 'NONE', #5047, 1000.000000000000000 ) ;
#40867 = FACE_BOUND ( 'NONE', #901, .T. ) ;
#40869 = DIRECTION ( 'NONE',  ( 0.000000000000000000, 0.4647231720437755564, 0.8854560256532062468 ) ) ;
#40870 = ORIENTED_EDGE ( 'NONE', *, *, #5789, .F. ) ;
#40871 = VECTOR ( 'NONE', #12106, 1000.000000000000227 ) ;
#40872 = AXIS2_PLACEMENT_3D ( 'NONE', #23680, #48660, #36285 ) ;
#40873 = EDGE_LOOP ( 'NONE', ( #33026, #27036, #7659, #49844 ) ) ;
#40875 = ORIENTED_EDGE ( 'NONE', *, *, #36139, .T. ) ;
#40874 = DIRECTION ( 'NONE',  ( -1.000000000000000000, 0.000000000000000000, 0.000000000000000000 ) ) ;
#40876 = ORIENTED_EDGE ( 'NONE', *, *, #18836, .F. ) ;
#40877 = CARTESIAN_POINT ( 'NONE',  ( -49.44376233341720450, -177.1207230881787780, -0.2635871660690713436 ) ) ;
#40878 = DIRECTION ( 'NONE',  ( 0.000000000000000000, 0.000000000000000000, 1.000000000000000000 ) ) ;
#40879 = CARTESIAN_POINT ( 'NONE',  ( -332.3517673607765914, -123.5000000000000284, 0.000000000000000000 ) ) ;
#40880 = DIRECTION ( 'NONE',  ( 0.000000000000000000, 1.000000000000000000, -0.000000000000000000 ) ) ;
#40881 = ORIENTED_EDGE ( 'NONE', *, *, #48094, .F. ) ;
#40882 = PLANE ( 'NONE',  #38457 ) ;
#40883 = ORIENTED_EDGE ( 'NONE', *, *, #13203, .F. ) ;
#40884 = ADVANCED_FACE ( 'NONE', ( #15581 ), #39479, .T. ) ;
#40885 = EDGE_LOOP ( 'NONE', ( #5881, #35784, #37001, #50292 ) ) ;
#40886 = CARTESIAN_POINT ( 'NONE',  ( 51.65665342072240662, -193.5000000000000000, 74.81861753132422166 ) ) ;
#40887 = CIRCLE ( 'NONE', #38386, 125.0000000000000000 ) ;
#40888 = VECTOR ( 'NONE', #2645, 1000.000000000000000 ) ;
#40889 = DIRECTION ( 'NONE',  ( 0.000000000000000000, 1.000000000000000000, 0.000000000000000000 ) ) ;
#40890 = DIRECTION ( 'NONE',  ( 0.000000000000000000, 0.000000000000000000, -1.000000000000000000 ) ) ;
#40891 = VECTOR ( 'NONE', #35616, 1000.000000000000227 ) ;
#40892 = DIRECTION ( 'NONE',  ( 0.000000000000000000, 0.000000000000000000, 1.000000000000000000 ) ) ;
#40893 = CARTESIAN_POINT ( 'NONE',  ( 8.448131207122532516, -175.3837268820161057, 111.2847127925100352 ) ) ;
#40894 = CARTESIAN_POINT ( 'NONE',  ( -154.0877180371535360, -189.7472609257535510, -66.87170886601934683 ) ) ;
#40895 = EDGE_CURVE ( 'NONE', #38101, #22193, #43063, .T. ) ;
#40896 = VERTEX_POINT ( 'NONE', #11358 ) ;
#40897 = CARTESIAN_POINT ( 'NONE',  ( -336.3521761649654422, -123.5000000000000284, 0.000000000000000000 ) ) ;
#40898 = DIRECTION ( 'NONE',  ( 0.000000000000000000, 0.000000000000000000, -1.000000000000000000 ) ) ;
#40899 = CARTESIAN_POINT ( 'NONE',  ( -129.5578577291867646, -189.7472609257535510, 93.82025162278060293 ) ) ;
#40900 = FACE_BOUND ( 'NONE', #50287, .T. ) ;
#40901 = ORIENTED_EDGE ( 'NONE', *, *, #18309, .F. ) ;
#40902 = AXIS2_PLACEMENT_3D ( 'NONE', #6942, #42423, #38487 ) ;
#40903 = EDGE_CURVE ( 'NONE', #25927, #14590, #22950, .T. ) ;
#40904 = VECTOR ( 'NONE', #15283, 1000.000000000000000 ) ;
#40905 = FACE_OUTER_BOUND ( 'NONE', #48384, .T. ) ;
#40906 = VERTEX_POINT ( 'NONE', #11632 ) ;
#40907 = CIRCLE ( 'NONE', #24984, 5.000000000000001776 ) ;
#40908 = DIRECTION ( 'NONE',  ( 0.000000000000000000, 0.9927088740980534176, -0.1205366802553268502 ) ) ;
#40909 = ORIENTED_EDGE ( 'NONE', *, *, #50630, .T. ) ;
#40910 = CARTESIAN_POINT ( 'NONE',  ( -238.7407812814481076, -213.5000000000000000, 10.00000000000000178 ) ) ;
#40911 = VECTOR ( 'NONE', #39142, 1000.000000000000000 ) ;
#40912 = ORIENTED_EDGE ( 'NONE', *, *, #50440, .F. ) ;
#40913 = VECTOR ( 'NONE', #32321, 1000.000000000000000 ) ;
#40914 = DIRECTION ( 'NONE',  ( -0.8757349421956345248, 0.000000000000000000, -0.4827922027307490205 ) ) ;
#40915 = DIRECTION ( 'NONE',  ( 0.000000000000000000, 0.000000000000000000, 1.000000000000000000 ) ) ;
#40917 = EDGE_LOOP ( 'NONE', ( #22556, #36694, #28435, #39745 ) ) ;
#40916 = CARTESIAN_POINT ( 'NONE',  ( -336.3521761649654422, -65.82380048139334860, 12.53476669029061519 ) ) ;
#40918 = ADVANCED_FACE ( 'NONE', ( #19763 ), #16100, .F. ) ;
#40919 = EDGE_CURVE ( 'NONE', #50197, #12264, #27909, .T. ) ;
#40920 = DIRECTION ( 'NONE',  ( 0.000000000000000000, 1.000000000000000000, 0.000000000000000000 ) ) ;
#40921 = ORIENTED_EDGE ( 'NONE', *, *, #50072, .T. ) ;
#40922 = ORIENTED_EDGE ( 'NONE', *, *, #42830, .T. ) ;
#40923 = ORIENTED_EDGE ( 'NONE', *, *, #11762, .F. ) ;
#40924 = DIRECTION ( 'NONE',  ( -0.000000000000000000, -1.000000000000000000, 0.000000000000000000 ) ) ;
#40925 = AXIS2_PLACEMENT_3D ( 'NONE', #47171, #30346, #6458 ) ;
#40926 = CARTESIAN_POINT ( 'NONE',  ( -18.54723674587610560, -189.7472609257535510, 120.3332351033025702 ) ) ;
#40927 = VECTOR ( 'NONE', #27570, 999.9999999999998863 ) ;
#40928 = ORIENTED_EDGE ( 'NONE', *, *, #15580, .T. ) ;
#40929 = PLANE ( 'NONE',  #46926 ) ;
#40930 = CARTESIAN_POINT ( 'NONE',  ( 46.00000000000000711, -43.50000000000000000, -41.99999999999999289 ) ) ;
#40931 = CARTESIAN_POINT ( 'NONE',  ( 65.79610465833508215, -177.1207230881787780, -50.65739320401928580 ) ) ;
#40932 = AXIS2_PLACEMENT_3D ( 'NONE', #51345, #11376, #27411 ) ;
#40933 = FACE_OUTER_BOUND ( 'NONE', #45777, .T. ) ;
#40934 = DIRECTION ( 'NONE',  ( 0.000000000000000000, -0.9927088740980530845, 0.1205366802553303196 ) ) ;
#40935 = ORIENTED_EDGE ( 'NONE', *, *, #51638, .F. ) ;
#40938 = EDGE_LOOP ( 'NONE', ( #15673, #32125, #22215, #21204 ) ) ;
#40937 = LINE ( 'NONE', #43837, #10482 ) ;
#40936 = CARTESIAN_POINT ( 'NONE',  ( -167.6453766917639427, -183.6283474603465606, 37.74128873232411507 ) ) ;
#40939 = VECTOR ( 'NONE', #30573, 999.9999999999998863 ) ;
#40940 = ORIENTED_EDGE ( 'NONE', *, *, #15698, .F. ) ;
#40941 = CARTESIAN_POINT ( 'NONE',  ( -180.0000000000000568, -115.7896721143442278, -60.00000000000000711 ) ) ;
#40942 = EDGE_LOOP ( 'NONE', ( #26095, #16798, #47843, #4400 ) ) ;
#40943 = DIRECTION ( 'NONE',  ( 1.000000000000000000, 0.000000000000000000, -6.978251959525016136E-17 ) ) ;
#40944 = EDGE_CURVE ( 'NONE', #10598, #42603, #23470, .T. ) ;
#40945 = ORIENTED_EDGE ( 'NONE', *, *, #15766, .T. ) ;
#40946 = EDGE_CURVE ( 'NONE', #51787, #48702, #35034, .T. ) ;
#40947 = CARTESIAN_POINT ( 'NONE',  ( -33.86391487983341619, -175.3837268820161057, 124.1426420773540542 ) ) ;
#40948 = DIRECTION ( 'NONE',  ( 0.000000000000000000, 0.000000000000000000, -1.000000000000000000 ) ) ;
#40949 = EDGE_LOOP ( 'NONE', ( #51458, #11525, #269, #33905 ) ) ;
#40950 = CARTESIAN_POINT ( 'NONE',  ( -48.47912675150885065, -183.6283474603465606, 6.938893903907228378E-15 ) ) ;
#40951 = VERTEX_POINT ( 'NONE', #7689 ) ;
#40952 = VECTOR ( 'NONE', #45742, 1000.000000000000000 ) ;
#40953 = VERTEX_POINT ( 'NONE', #11105 ) ;
#40954 = CARTESIAN_POINT ( 'NONE',  ( -330.4913330509368166, -64.50000000000000000, 0.4999999999999551470 ) ) ;
#40955 = PLANE ( 'NONE',  #5544 ) ;
#40956 = PLANE ( 'NONE',  #24695 ) ;
#40957 = PLANE ( 'NONE',  #33391 ) ;
#40958 = VERTEX_POINT ( 'NONE', #31337 ) ;
#40959 = CARTESIAN_POINT ( 'NONE',  ( -170.0000000000000284, -123.5000000000000284, 6.938893903907228378E-15 ) ) ;
#40960 = APPLICATION_PROTOCOL_DEFINITION ( 'draft international standard', 'automotive_design', 1998, #10557 ) ;
#40961 = DIRECTION ( 'NONE',  ( 0.000000000000000000, 1.000000000000000000, -0.000000000000000000 ) ) ;
#40962 = EDGE_CURVE ( 'NONE', #21654, #48787, #27133, .T. ) ;
#40963 = DIRECTION ( 'NONE',  ( 0.7765238627180437447, 0.000000000000000000, -0.6300878435817094392 ) ) ;
#40964 = DIRECTION ( 'NONE',  ( -1.000000000000000000, 0.000000000000000000, 0.000000000000000000 ) ) ;
#40965 = ADVANCED_FACE ( 'NONE', ( #39232 ), #47900, .T. ) ;
#40966 = EDGE_CURVE ( 'NONE', #16634, #15304, #39699, .T. ) ;
#40967 = DIRECTION ( 'NONE',  ( 0.000000000000000000, 0.000000000000000000, 1.000000000000000000 ) ) ;
#40968 = ORIENTED_EDGE ( 'NONE', *, *, #41678, .T. ) ;
#40969 = ORIENTED_EDGE ( 'NONE', *, *, #7568, .T. ) ;
#40970 = CIRCLE ( 'NONE', #18328, 125.0000000000000000 ) ;
#40971 = EDGE_CURVE ( 'NONE', #50838, #8505, #19276, .T. ) ;
#40972 = FACE_OUTER_BOUND ( 'NONE', #29010, .T. ) ;
#40973 = VECTOR ( 'NONE', #2926, 1000.000000000000000 ) ;
#40974 = EDGE_CURVE ( 'NONE', #19921, #43567, #13194, .T. ) ;
#40975 = VECTOR ( 'NONE', #10298, 1000.000000000000000 ) ;
#40976 = PLANE ( 'NONE',  #11790 ) ;
#40977 = CARTESIAN_POINT ( 'NONE',  ( -330.4913330509368166, -175.9742670995615015, -26.97593913775547136 ) ) ;
#40978 = ORIENTED_EDGE ( 'NONE', *, *, #5411, .F. ) ;
#40979 = ORIENTED_EDGE ( 'NONE', *, *, #12262, .F. ) ;
#40980 = ORIENTED_EDGE ( 'NONE', *, *, #2532, .T. ) ;
#40981 = VECTOR ( 'NONE', #31875, 1000.000000000000114 ) ;
#40982 = CARTESIAN_POINT ( 'NONE',  ( 31.28129687248616619, -183.6283474603465606, 96.24590808611479531 ) ) ;
#40983 = CARTESIAN_POINT ( 'NONE',  ( 64.86941505090324256, -177.1207230881787780, -50.28156562190505241 ) ) ;
#40984 = DIRECTION ( 'NONE',  ( -8.718379230999707126E-17, 0.8854560256532110207, 0.4647231720437664526 ) ) ;
#40985 = CARTESIAN_POINT ( 'NONE',  ( -146.2338470511239450, -183.6283474603465606, 76.29032973288700248 ) ) ;
#40986 = ORIENTED_EDGE ( 'NONE', *, *, #51794, .T. ) ;
#40987 = DIRECTION ( 'NONE',  ( 0.000000000000000000, 0.000000000000000000, 1.000000000000000000 ) ) ;
#40988 = CARTESIAN_POINT ( 'NONE',  ( -91.22542124915045747, -189.7472609257535510, 117.4638425504669925 ) ) ;
#40989 = ORIENTED_EDGE ( 'NONE', *, *, #33557, .F. ) ;
#40990 = CIRCLE ( 'NONE', #44348, 124.9999999999999858 ) ;
#40991 = DIRECTION ( 'NONE',  ( -0.000000000000000000, -1.000000000000000000, -0.000000000000000000 ) ) ;
#40992 = ORIENTED_EDGE ( 'NONE', *, *, #12038, .F. ) ;
#40993 = FACE_OUTER_BOUND ( 'NONE', #34726, .T. ) ;
#40994 = ORIENTED_EDGE ( 'NONE', *, *, #30757, .T. ) ;
#40995 = DIRECTION ( 'NONE',  ( -0.000000000000000000, -1.000000000000000000, 0.000000000000000000 ) ) ;
#40996 = DIRECTION ( 'NONE',  ( -0.000000000000000000, 1.000000000000000000, -0.000000000000000000 ) ) ;
#40997 = CARTESIAN_POINT ( 'NONE',  ( -65.65563056894595206, -183.6283474603465606, 123.8142468240612857 ) ) ;
#41000 = ORIENTED_EDGE ( 'NONE', *, *, #10908, .F. ) ;
#40999 = CARTESIAN_POINT ( 'NONE',  ( -49.46816693883101124, -183.6283474603465606, -0.1476465640024848536 ) ) ;
#40998 = CARTESIAN_POINT ( 'NONE',  ( -80.17897391495031911, -183.6283474603465606, 120.9136869416132498 ) ) ;
#41001 = VECTOR ( 'NONE', #46091, 1000.000000000000000 ) ;
#41002 = LINE ( 'NONE', #4494, #6346 ) ;
#41003 = ORIENTED_EDGE ( 'NONE', *, *, #19143, .F. ) ;
#41004 = CARTESIAN_POINT ( 'NONE',  ( -48.47912675150885065, -175.3837268820161057, 6.938893903907228378E-15 ) ) ;
#41006 = AXIS2_PLACEMENT_3D ( 'NONE', #12024, #44094, #40153 ) ;
#41005 = LINE ( 'NONE', #18071, #25788 ) ;
#41007 = ORIENTED_EDGE ( 'NONE', *, *, #7337, .T. ) ;
#41008 = ADVANCED_FACE ( 'NONE', ( #8993 ), #20285, .F. ) ;
#41009 = EDGE_CURVE ( 'NONE', #38856, #11608, #16355, .T. ) ;
#41010 = EDGE_CURVE ( 'NONE', #41489, #31192, #43884, .T. ) ;
#41011 = LINE ( 'NONE', #17386, #19136 ) ;
#41013 = DIRECTION ( 'NONE',  ( -0.7765238627180482966, 0.000000000000000000, 0.6300878435817038881 ) ) ;
#41012 = CARTESIAN_POINT ( 'NONE',  ( 6.443011874827243801, -183.6283474603465606, 112.2878385610370771 ) ) ;
#41014 = ORIENTED_EDGE ( 'NONE', *, *, #11224, .F. ) ;
#41015 = EDGE_CURVE ( 'NONE', #46251, #48376, #9502, .T. ) ;
#41016 = VECTOR ( 'NONE', #32937, 1000.000000000000000 ) ;
#41017 = CARTESIAN_POINT ( 'NONE',  ( -305.0000000000000568, -63.52220716707010695, -1.632288850093980725 ) ) ;
#41018 = CARTESIAN_POINT ( 'NONE',  ( -336.3521761649654422, -141.9604555052315220, 56.09938080879057765 ) ) ;
#41019 = FACE_OUTER_BOUND ( 'NONE', #38140, .T. ) ;
#41020 = EDGE_LOOP ( 'NONE', ( #24022, #26990, #10212, #16362 ) ) ;
#41021 = FILL_AREA_STYLE_COLOUR ( '', #31649 ) ;
#41022 = EDGE_CURVE ( 'NONE', #13401, #46759, #19580, .T. ) ;
#41023 = CARTESIAN_POINT ( 'NONE',  ( -112.2501518587239104, -193.5000000000000000, -106.3450133598699665 ) ) ;
#41024 = CARTESIAN_POINT ( 'NONE',  ( -33.98218805075476467, -189.7472609257535510, 123.1496609813405456 ) ) ;
#41025 = ORIENTED_EDGE ( 'NONE', *, *, #24088, .F. ) ;
#41026 = ADVANCED_FACE ( 'NONE', ( #49199 ), #17140, .T. ) ;
#41027 = FACE_OUTER_BOUND ( 'NONE', #18244, .T. ) ;
#41028 = EDGE_CURVE ( 'NONE', #39766, #44661, #27938, .T. ) ;
#41029 = AXIS2_PLACEMENT_3D ( 'NONE', #942, #48541, #16987 ) ;
#41030 = DIRECTION ( 'NONE',  ( -0.5586467658036594619, 0.000000000000000000, 0.8294056854501971054 ) ) ;
#41031 = EDGE_LOOP ( 'NONE', ( #639, #63, #17838, #9813 ) ) ;
#41032 = ADVANCED_FACE ( 'NONE', ( #45272 ), #48938, .T. ) ;
#41033 = DIRECTION ( 'NONE',  ( -0.5586467658036415873, 0.000000000000000000, -0.8294056854502090959 ) ) ;
#41034 = CARTESIAN_POINT ( 'NONE',  ( -339.1964088526558498, -123.5000000000000284, 0.000000000000000000 ) ) ;
#41035 = EDGE_CURVE ( 'NONE', #34925, #49907, #37091, .T. ) ;
#41036 = CARTESIAN_POINT ( 'NONE',  ( -170.2790847791494855, -193.5000000000000000, -28.10285082451569494 ) ) ;
#41037 = DIRECTION ( 'NONE',  ( 1.000000000000000000, -0.000000000000000000, 0.000000000000000000 ) ) ;
#41038 = DIRECTION ( 'NONE',  ( 0.000000000000000000, 0.000000000000000000, 1.000000000000000000 ) ) ;
#41039 = VECTOR ( 'NONE', #44933, 1000.000000000000000 ) ;
#41040 = CARTESIAN_POINT ( 'NONE',  ( -167.4530144994566285, -177.1207230881787780, -34.94873081740328757 ) ) ;
#41041 = CARTESIAN_POINT ( 'NONE',  ( -339.1964088526558498, -180.6659093959932250, 14.60509510167942437 ) ) ;
#41043 = ORIENTED_EDGE ( 'NONE', *, *, #20498, .T. ) ;
#41042 = DIRECTION ( 'NONE',  ( -0.000000000000000000, 1.000000000000000000, -0.000000000000000000 ) ) ;
#41044 = AXIS2_PLACEMENT_3D ( 'NONE', #5149, #37900, #32207 ) ;
#41045 = EDGE_LOOP ( 'NONE', ( #1809, #1674, #16299, #35757 ) ) ;
#41046 = FACE_OUTER_BOUND ( 'NONE', #15416, .T. ) ;
#41047 = EDGE_CURVE ( 'NONE', #35050, #45987, #9256, .T. ) ;
#41048 = CARTESIAN_POINT ( 'NONE',  ( -44.48323084606168720, -183.6283474603465606, 124.9361149384469769 ) ) ;
#41049 = ORIENTED_EDGE ( 'NONE', *, *, #45926, .T. ) ;
#41050 = CIRCLE ( 'NONE', #19232, 60.00000000000000000 ) ;
#41051 = EDGE_LOOP ( 'NONE', ( #11406, #49380, #16143, #38446 ) ) ;
#41052 = VERTEX_POINT ( 'NONE', #20546 ) ;
#41053 = CARTESIAN_POINT ( 'NONE',  ( -106.4764934152196645, -193.5000000000000000, -110.7307791902282474 ) ) ;
#41054 = DIRECTION ( 'NONE',  ( 0.000000000000000000, 0.000000000000000000, 1.000000000000000000 ) ) ;
#41055 = DIRECTION ( 'NONE',  ( 0.000000000000000000, -1.000000000000000000, -0.000000000000000000 ) ) ;
#41056 = ORIENTED_EDGE ( 'NONE', *, *, #39538, .F. ) ;
#41057 = ORIENTED_EDGE ( 'NONE', *, *, #4115, .F. ) ;
#41058 = AXIS2_PLACEMENT_3D ( 'NONE', #48205, #21589, #12903 ) ;
#41059 = EDGE_CURVE ( 'NONE', #50918, #36788, #7800, .T. ) ;
#41060 = DIRECTION ( 'NONE',  ( 0.000000000000000000, -0.000000000000000000, -1.000000000000000000 ) ) ;
#41062 = ORIENTED_EDGE ( 'NONE', *, *, #10116, .T. ) ;
#41061 = DIRECTION ( 'NONE',  ( -0.5338233779648003940, 0.000000000000000000, 0.8455960035018199594 ) ) ;
#41063 = CARTESIAN_POINT ( 'NONE',  ( 74.13662511985246795, -193.5000000000000000, 18.47640724094592457 ) ) ;
#41064 = ORIENTED_EDGE ( 'NONE', *, *, #1459, .F. ) ;
#41065 = CARTESIAN_POINT ( 'NONE',  ( -336.3521761649654422, -146.8829211657874794, -54.23253582808848705 ) ) ;
#41066 = ORIENTED_EDGE ( 'NONE', *, *, #49818, .F. ) ;
#41067 = ADVANCED_FACE ( 'NONE', ( #12918 ), #16629, .T. ) ;
#41068 = EDGE_CURVE ( 'NONE', #30276, #15240, #12655, .T. ) ;
#41069 = EDGE_CURVE ( 'NONE', #33404, #2064, #17909, .T. ) ;
#41070 = EDGE_CURVE ( 'NONE', #1407, #34403, #20820, .T. ) ;
#41071 = DIRECTION ( 'NONE',  ( 0.000000000000000000, -1.000000000000000000, 0.000000000000000000 ) ) ;
#41072 = CARTESIAN_POINT ( 'NONE',  ( -4.176930889631405464, -175.3837268820161057, 116.8859077982279615 ) ) ;
#41073 = PLANE ( 'NONE',  #34137 ) ;
#41074 = EDGE_CURVE ( 'NONE', #13416, #12178, #16882, .T. ) ;
#41075 = ORIENTED_EDGE ( 'NONE', *, *, #33944, .T. ) ;
#41076 = VERTEX_POINT ( 'NONE', #8209 ) ;
#41077 = LINE ( 'NONE', #17955, #14730 ) ;
#41079 = AXIS2_PLACEMENT_3D ( 'NONE', #35101, #50886, #38532 ) ;
#41078 = DIRECTION ( 'NONE',  ( -0.4031234292879792847, 0.000000000000000000, 0.9151456172430153524 ) ) ;
#41080 = VERTEX_POINT ( 'NONE', #40247 ) ;
#41081 = EDGE_CURVE ( 'NONE', #40102, #755, #25438, .T. ) ;
#41082 = EDGE_CURVE ( 'NONE', #1973, #50621, #25528, .T. ) ;
#41083 = DIRECTION ( 'NONE',  ( 0.2348860457809775482, 0.000000000000000000, 0.9720229140804121926 ) ) ;
#41084 = MECHANICAL_DESIGN_GEOMETRIC_PRESENTATION_REPRESENTATION (  '', ( #13294 ), #38458 ) ;
#41085 = CARTESIAN_POINT ( 'NONE',  ( -339.1964088526558498, -123.5000000000000284, 0.000000000000000000 ) ) ;
#41086 = VERTEX_POINT ( 'NONE', #42075 ) ;
#41087 = CARTESIAN_POINT ( 'NONE',  ( -81.14588623932559130, -193.5000000000000000, 120.6560517527618117 ) ) ;
#41088 = ADVANCED_FACE ( 'NONE', ( #2127, #33925 ), #1629, .F. ) ;
#41089 = CARTESIAN_POINT ( 'NONE',  ( 47.80033453782772312, 28.88712326890129489, -48.86858413038775240 ) ) ;
#41090 = ADVANCED_FACE ( 'NONE', ( #22113 ), #5846, .F. ) ;
#41091 = EDGE_LOOP ( 'NONE', ( #18409, #48599, #33541, #47442 ) ) ;
#41092 = FACE_OUTER_BOUND ( 'NONE', #51616, .T. ) ;
#41093 = ORIENTED_EDGE ( 'NONE', *, *, #37827, .T. ) ;
#41094 = DIRECTION ( 'NONE',  ( -0.000000000000000000, 1.000000000000000000, -0.000000000000000000 ) ) ;
#41095 = EDGE_CURVE ( 'NONE', #28776, #48767, #37627, .T. ) ;
#41096 = CARTESIAN_POINT ( 'NONE',  ( 75.28414827670441412, -183.6283474603465606, -7.666780576874951514 ) ) ;
#41097 = ORIENTED_EDGE ( 'NONE', *, *, #36950, .F. ) ;
#41098 = EDGE_CURVE ( 'NONE', #22244, #14314, #21861, .T. ) ;
#41099 = DIRECTION ( 'NONE',  ( 0.000000000000000000, 1.000000000000000000, -0.000000000000000000 ) ) ;
#41100 = DIRECTION ( 'NONE',  ( 0.000000000000000000, -1.000000000000000000, 0.000000000000000000 ) ) ;
#41101 = DIRECTION ( 'NONE',  ( -1.000000000000000000, 0.000000000000000000, -0.000000000000000000 ) ) ;
#41102 = FACE_OUTER_BOUND ( 'NONE', #27004, .T. ) ;
#41103 = ADVANCED_FACE ( 'NONE', ( #37877 ), #26303, .T. ) ;
#41104 = VECTOR ( 'NONE', #3570, 1000.000000000000000 ) ;
#41105 = ORIENTED_EDGE ( 'NONE', *, *, #39632, .T. ) ;
#41106 = DIRECTION ( 'NONE',  ( 0.000000000000000000, 0.000000000000000000, 1.000000000000000000 ) ) ;
#41107 = VERTEX_POINT ( 'NONE', #30255 ) ;
#41108 = APPLICATION_CONTEXT ( 'automotive_design' ) ;
#41109 = ORIENTED_EDGE ( 'NONE', *, *, #41799, .F. ) ;
#41110 = LINE ( 'NONE', #17730, #31038 ) ;
#41112 = ORIENTED_EDGE ( 'NONE', *, *, #15400, .T. ) ;
#41111 = CARTESIAN_POINT ( 'NONE',  ( -38.66762320617017679, -183.6283474603465606, -124.6143426664033740 ) ) ;
#41113 = ORIENTED_EDGE ( 'NONE', *, *, #7628, .F. ) ;
#41114 = PLANE ( 'NONE',  #6418 ) ;
#41115 = ADVANCED_FACE ( 'NONE', ( #17917 ), #29724, .F. ) ;
#41116 = LINE ( 'NONE', #17211, #19565 ) ;
#41117 = FACE_OUTER_BOUND ( 'NONE', #11099, .T. ) ;
#41118 = ORIENTED_EDGE ( 'NONE', *, *, #5910, .F. ) ;
#41119 = VECTOR ( 'NONE', #51036, 1000.000000000000000 ) ;
#41120 = DIRECTION ( 'NONE',  ( 0.000000000000000000, 0.000000000000000000, -1.000000000000000000 ) ) ;
#41121 = ORIENTED_EDGE ( 'NONE', *, *, #39092, .F. ) ;
#41122 = FACE_OUTER_BOUND ( 'NONE', #3032, .T. ) ;
#41123 = LINE ( 'NONE', #13785, #5734 ) ;
#41124 = DIRECTION ( 'NONE',  ( -0.5586467658036476935, 0.000000000000000000, -0.8294056854502049880 ) ) ;
#41125 = CARTESIAN_POINT ( 'NONE',  ( -48.47912675150885065, -177.1207230881787780, 6.938893903907228378E-15 ) ) ;
#41126 = VERTEX_POINT ( 'NONE', #38125 ) ;
#41127 = VERTEX_POINT ( 'NONE', #29466 ) ;
#41128 = VERTEX_POINT ( 'NONE', #29997 ) ;
#41129 = DIRECTION ( 'NONE',  ( 0.000000000000000000, -0.5680647467311656929, -0.8229838658936495799 ) ) ;
#41130 = DIRECTION ( 'NONE',  ( 0.000000000000000000, 0.000000000000000000, -1.000000000000000000 ) ) ;
#41131 = LINE ( 'NONE', #6118, #30134 ) ;
#41132 = FACE_BOUND ( 'NONE', #23054, .T. ) ;
#41133 = CARTESIAN_POINT ( 'NONE',  ( -48.47912675150885065, -193.5000000000000000, 125.0000000000000000 ) ) ;
#41134 = ORIENTED_EDGE ( 'NONE', *, *, #50822, .T. ) ;
#41135 = ADVANCED_FACE ( 'NONE', ( #42331 ), #6093, .F. ) ;
#41136 = EDGE_CURVE ( 'NONE', #17733, #15597, #22104, .T. ) ;
#41137 = VECTOR ( 'NONE', #2733, 999.9999999999998863 ) ;
#41138 = VECTOR ( 'NONE', #23210, 1000.000000000000227 ) ;
#41139 = ORIENTED_EDGE ( 'NONE', *, *, #19388, .T. ) ;
#41141 = ORIENTED_EDGE ( 'NONE', *, *, #5081, .F. ) ;
#41140 = DIRECTION ( 'NONE',  ( -0.000000000000000000, 1.000000000000000000, -0.000000000000000000 ) ) ;
#41142 = ORIENTED_EDGE ( 'NONE', *, *, #26947, .T. ) ;
#41143 = DIRECTION ( 'NONE',  ( 0.000000000000000000, 0.000000000000000000, -1.000000000000000000 ) ) ;
#41144 = DIRECTION ( 'NONE',  ( -0.9646355819083556327, 0.000000000000000000, -0.2635871660690782825 ) ) ;
#41145 = CARTESIAN_POINT ( 'NONE',  ( -305.0000000000000568, -130.2355952558264107, 59.62073260661670560 ) ) ;
#41146 = DIRECTION ( 'NONE',  ( 0.000000000000000000, 0.000000000000000000, 1.000000000000000000 ) ) ;
#41147 = CARTESIAN_POINT ( 'NONE',  ( -330.4913330509368166, -123.5000000000000284, 0.000000000000000000 ) ) ;
#41148 = ORIENTED_EDGE ( 'NONE', *, *, #42039, .T. ) ;
#41149 = LINE ( 'NONE', #45630, #29229 ) ;
#41150 = VERTEX_POINT ( 'NONE', #38394 ) ;
#41151 = ORIENTED_EDGE ( 'NONE', *, *, #38966, .F. ) ;
#41152 = DIRECTION ( 'NONE',  ( 0.000000000000000000, 0.000000000000000000, -1.000000000000000000 ) ) ;
#41153 = CONICAL_SURFACE ( 'NONE', #46201, 15.00000000000000000, 0.7853981633974526089 ) ;
#41154 = ADVANCED_FACE ( 'NONE', ( #18434 ), #34450, .T. ) ;
#41155 = CARTESIAN_POINT ( 'NONE',  ( -330.4913330509368166, -108.8949048983204904, 57.16590939599316812 ) ) ;
#41156 = DIRECTION ( 'NONE',  ( -0.05924062789370006937, 0.000000000000000000, -0.9982437317643222396 ) ) ;
#41157 = DIRECTION ( 'NONE',  ( -0.000000000000000000, 1.000000000000000000, 0.000000000000000000 ) ) ;
#41158 = CARTESIAN_POINT ( 'NONE',  ( 71.18041382641611392, -193.5000000000000000, -32.52067927015754378 ) ) ;
#41159 = ORIENTED_EDGE ( 'NONE', *, *, #33469, .F. ) ;
#41160 = DIRECTION ( 'NONE',  ( 0.9929810960135178055, 0.000000000000000000, -0.1182731709213592358 ) ) ;
#41161 = CARTESIAN_POINT ( 'NONE',  ( -118.1688136093591908, -193.5000000000000000, -103.7706487676296661 ) ) ;
#41162 = ADVANCED_FACE ( 'NONE', ( #49476 ), #9508, .F. ) ;
#41163 = LINE ( 'NONE', #5183, #24470 ) ;
#41164 = FACE_BOUND ( 'NONE', #22262, .T. ) ;
#41165 = VERTEX_POINT ( 'NONE', #16532 ) ;
#41166 = CARTESIAN_POINT ( 'NONE',  ( 72.82672500347334221, -175.3837268820161057, 25.70779184431858866 ) ) ;
#41167 = EDGE_LOOP ( 'NONE', ( #49136, #38014, #20255, #25765 ) ) ;
#41168 = DIRECTION ( 'NONE',  ( 1.000000000000000000, -0.000000000000000000, -0.000000000000000000 ) ) ;
#41169 = PLANE ( 'NONE',  #38858 ) ;
#41170 = ORIENTED_EDGE ( 'NONE', *, *, #21374, .T. ) ;
#41171 = AXIS2_PLACEMENT_3D ( 'NONE', #48115, #19468, #39190 ) ;
#41172 = VECTOR ( 'NONE', #20752, 1000.000000000000000 ) ;
#41173 = LINE ( 'NONE', #33559, #37743 ) ;
#41174 = CARTESIAN_POINT ( 'NONE',  ( -339.1964088526558498, -143.9541802141663709, 55.34326076196097688 ) ) ;
#41176 = VERTEX_POINT ( 'NONE', #48597 ) ;
#41175 = DIRECTION ( 'NONE',  ( -1.000000000000000000, 0.000000000000000000, 0.000000000000000000 ) ) ;
#41177 = CARTESIAN_POINT ( 'NONE',  ( -305.0000000000000568, -143.2422018649890276, 56.65902810251888155 ) ) ;
#41178 = VERTEX_POINT ( 'NONE', #8628 ) ;
#41179 = VERTEX_POINT ( 'NONE', #24930 ) ;
#41180 = ORIENTED_EDGE ( 'NONE', *, *, #31408, .T. ) ;
#41181 = PLANE ( 'NONE',  #6635 ) ;
#41182 = LINE ( 'NONE', #1508, #26837 ) ;
#41183 = CIRCLE ( 'NONE', #3413, 125.0000000000000000 ) ;
#41184 = VERTEX_POINT ( 'NONE', #33586 ) ;
#41185 = PLANE ( 'NONE',  #47169 ) ;
#41186 = LINE ( 'NONE', #25940, #40600 ) ;
#41187 = EDGE_LOOP ( 'NONE', ( #9419, #37565, #34363, #8095 ) ) ;
#41188 = ADVANCED_FACE ( 'NONE', ( #4693, #28849 ), #20453, .F. ) ;
#41189 = CARTESIAN_POINT ( 'NONE',  ( -47.57632892154311577, -193.5000000000000000, 0.4300652022765314997 ) ) ;
#41190 = DIRECTION ( 'NONE',  ( -0.000000000000000000, -0.7485107481710953081, 0.6631226582408016323 ) ) ;
#41191 = ORIENTED_EDGE ( 'NONE', *, *, #7214, .F. ) ;
#41194 = ORIENTED_EDGE ( 'NONE', *, *, #28137, .F. ) ;
#41193 = DIRECTION ( 'NONE',  ( -0.000000000000000000, 1.000000000000000000, -0.000000000000000000 ) ) ;
#41192 = FACE_OUTER_BOUND ( 'NONE', #33797, .T. ) ;
#41195 = ORIENTED_EDGE ( 'NONE', *, *, #14446, .F. ) ;
#41196 = FACE_OUTER_BOUND ( 'NONE', #21129, .T. ) ;
#41197 = ORIENTED_EDGE ( 'NONE', *, *, #34984, .T. ) ;
#41198 = CARTESIAN_POINT ( 'NONE',  ( -152.8713435144644848, -183.6283474603465606, -68.75510947788595217 ) ) ;
#41199 = CIRCLE ( 'NONE', #11821, 125.0000000000000000 ) ;
#41200 = EDGE_LOOP ( 'NONE', ( #19331, #160, #26712, #38058 ) ) ;
#41201 = DIRECTION ( 'NONE',  ( -0.8896570909947467687, 0.000000000000000000, -0.4566292373937140270 ) ) ;
#41202 = DIRECTION ( 'NONE',  ( 0.5338233779647826305, 0.000000000000000000, 0.8455960035018311727 ) ) ;
#41203 = ORIENTED_EDGE ( 'NONE', *, *, #49630, .T. ) ;
#41204 = DIRECTION ( 'NONE',  ( 0.000000000000000000, 0.000000000000000000, 1.000000000000000000 ) ) ;
#41205 = ORIENTED_EDGE ( 'NONE', *, *, #42570, .F. ) ;
#41206 = CIRCLE ( 'NONE', #28598, 125.0000000000000000 ) ;
#41207 = ORIENTED_EDGE ( 'NONE', *, *, #305, .T. ) ;
#41208 = DIRECTION ( 'NONE',  ( -0.000000000000000000, 1.000000000000000000, -0.000000000000000000 ) ) ;
#41209 = CARTESIAN_POINT ( 'NONE',  ( 64.01121016852529522, -193.5000000000000000, -54.50618404930953176 ) ) ;
#41210 = EDGE_CURVE ( 'NONE', #5856, #20039, #33061, .T. ) ;
#41211 = PLANE ( 'NONE',  #40619 ) ;
#41212 = SURFACE_STYLE_USAGE ( .BOTH. , #41470 ) ;
#41213 = ORIENTED_EDGE ( 'NONE', *, *, #497, .T. ) ;
#41214 = DIRECTION ( 'NONE',  ( 0.000000000000000000, 0.000000000000000000, 1.000000000000000000 ) ) ;
#41215 = APPLICATION_PROTOCOL_DEFINITION ( 'draft international standard', 'automotive_design', 1998, #6200 ) ;
#41216 = DIRECTION ( 'NONE',  ( 0.000000000000000000, 1.000000000000000000, 0.000000000000000000 ) ) ;
#41217 = CARTESIAN_POINT ( 'NONE',  ( -48.47912675150885065, -173.5000000000000284, 15.00000000000000711 ) ) ;
#41218 = DIRECTION ( 'NONE',  ( -1.000000000000000000, 0.000000000000000000, 0.000000000000000000 ) ) ;
#41219 = DIRECTION ( 'NONE',  ( -1.000000000000000000, 0.000000000000000000, 0.000000000000000000 ) ) ;
#41220 = CARTESIAN_POINT ( 'NONE',  ( 10.73478887071926202, -177.1207230881787780, -110.0850225811106924 ) ) ;
#41221 = ADVANCED_FACE ( 'NONE', ( #44389 ), #13610, .T. ) ;
#41222 = ORIENTED_EDGE ( 'NONE', *, *, #14961, .F. ) ;
#41223 = CIRCLE ( 'NONE', #11841, 125.0000000000000000 ) ;
#41224 = DIRECTION ( 'NONE',  ( 1.000000000000000000, 0.000000000000000000, -0.000000000000000000 ) ) ;
#41225 = DIRECTION ( 'NONE',  ( 0.000000000000000000, 0.7485107481710934207, -0.6631226582408039638 ) ) ;
#41226 = VERTEX_POINT ( 'NONE', #40412 ) ;
#41227 = DIRECTION ( 'NONE',  ( 0.000000000000000000, -0.9709418174260534551, -0.2393156642875516327 ) ) ;
#41228 = ADVANCED_FACE ( 'NONE', ( #29375 ), #36472, .T. ) ;
#41229 = VERTEX_POINT ( 'NONE', #49374 ) ;
#41230 = CARTESIAN_POINT ( 'NONE',  ( 9.336583202542586335, -175.3837268820161057, 110.8257356506556164 ) ) ;
#41231 = DIRECTION ( 'NONE',  ( 0.000000000000000000, -1.000000000000000000, -0.000000000000000000 ) ) ;
#41232 = DIRECTION ( 'NONE',  ( -0.000000000000000000, 1.000000000000000000, -0.000000000000000000 ) ) ;
#41233 = DIRECTION ( 'NONE',  ( -0.6965510290630033685, 0.000000000000000000, 0.7175072570443249420 ) ) ;
#41234 = VECTOR ( 'NONE', #51646, 999.9999999999998863 ) ;
#41235 = ORIENTED_EDGE ( 'NONE', *, *, #42022, .F. ) ;
#41236 = ADVANCED_FACE ( 'NONE', ( #753 ), #32548, .F. ) ;
#41237 = DIRECTION ( 'NONE',  ( -0.000000000000000000, 1.000000000000000000, 0.000000000000000000 ) ) ;
#41238 = AXIS2_PLACEMENT_3D ( 'NONE', #16476, #32496, #37210 ) ;
#41239 = DIRECTION ( 'NONE',  ( -0.000000000000000000, 1.000000000000000000, -0.000000000000000000 ) ) ;
#41240 = AXIS2_PLACEMENT_3D ( 'NONE', #963, #17016, #47126 ) ;
#41241 = PLANE ( 'NONE',  #7193 ) ;
#41242 = EDGE_CURVE ( 'NONE', #16977, #14631, #27144, .T. ) ;
#41243 = ORIENTED_EDGE ( 'NONE', *, *, #6112, .F. ) ;
#41244 = DIRECTION ( 'NONE',  ( 1.000000000000000000, 0.000000000000000000, 0.000000000000000000 ) ) ;
#41245 = ORIENTED_EDGE ( 'NONE', *, *, #1352, .F. ) ;
#41246 = CARTESIAN_POINT ( 'NONE',  ( -49.21696003055057389, -177.1207230881787780, -0.6749830015182127774 ) ) ;
#41247 = ADVANCED_FACE ( 'NONE', ( #49624 ), #21502, .T. ) ;
#41248 = VECTOR ( 'NONE', #16824, 1000.000000000000000 ) ;
#41249 = EDGE_CURVE ( 'NONE', #10587, #23438, #17057, .T. ) ;
#41250 = CARTESIAN_POINT ( 'NONE',  ( -48.47912675150885065, -189.7472609257535510, 6.938893903907228378E-15 ) ) ;
#41251 = CARTESIAN_POINT ( 'NONE',  ( -131.8938452225253855, -183.6283474603465606, 93.09664195018557109 ) ) ;
#41252 = EDGE_LOOP ( 'NONE', ( #24599, #27356, #15747, #6212 ) ) ;
#41255 = ORIENTED_EDGE ( 'NONE', *, *, #32435, .T. ) ;
#41254 = DIRECTION ( 'NONE',  ( 0.000000000000000000, -1.000000000000000000, 0.000000000000000000 ) ) ;
#41253 = LINE ( 'NONE', #13412, #49341 ) ;
#41256 = EDGE_CURVE ( 'NONE', #37730, #44450, #29117, .T. ) ;
#41257 = AXIS2_PLACEMENT_3D ( 'NONE', #14772, #30785, #46829 ) ;
#41258 = CARTESIAN_POINT ( 'NONE',  ( -336.3521761649654422, -148.5878911270064009, 53.46519113769075204 ) ) ;
#41259 = ORIENTED_EDGE ( 'NONE', *, *, #42728, .T. ) ;
#41260 = DIRECTION ( 'NONE',  ( 0.000000000000000000, 0.000000000000000000, -1.000000000000000000 ) ) ;
#41261 = DIRECTION ( 'NONE',  ( 0.000000000000000000, 1.000000000000000000, 0.000000000000000000 ) ) ;
#41262 = VERTEX_POINT ( 'NONE', #45180 ) ;
#41263 = LINE ( 'NONE', #5290, #12399 ) ;
#41266 = EDGE_LOOP ( 'NONE', ( #28706, #4184, #18345, #27362 ) ) ;
#41265 = CARTESIAN_POINT ( 'NONE',  ( -365.0000000000001137, -168.5000000000000284, 0.000000000000000000 ) ) ;
#41264 = DIRECTION ( 'NONE',  ( 0.000000000000000000, 1.000000000000000000, -0.000000000000000000 ) ) ;
#41267 = VERTEX_POINT ( 'NONE', #21247 ) ;
#41268 = CARTESIAN_POINT ( 'NONE',  ( -162.3451783319732442, -193.5000000000000000, 51.57055649762783389 ) ) ;
#41269 = CARTESIAN_POINT ( 'NONE',  ( 51.78320179844650539, -193.5000000000000000, -72.96212019587142095 ) ) ;
#41270 = CARTESIAN_POINT ( 'NONE',  ( -332.3517673607765914, -105.0395444947681369, -56.09938080879045685 ) ) ;
#41271 = ORIENTED_EDGE ( 'NONE', *, *, #6510, .T. ) ;
#41272 = EDGE_CURVE ( 'NONE', #10210, #15063, #40670, .T. ) ;
#41273 = DIRECTION ( 'NONE',  ( -1.000000000000000000, 0.000000000000000000, -0.000000000000000000 ) ) ;
#41274 = FILL_AREA_STYLE_COLOUR ( '', #24030 ) ;
#41275 = DIRECTION ( 'NONE',  ( -0.3482016354343928088, 0.000000000000000000, -0.9374196611341231167 ) ) ;
#41276 = CIRCLE ( 'NONE', #46326, 125.0000000000000000 ) ;
#41277 = LINE ( 'NONE', #1616, #45048 ) ;
#41278 = ORIENTED_EDGE ( 'NONE', *, *, #26121, .F. ) ;
#41279 = VECTOR ( 'NONE', #12188, 1000.000000000000114 ) ;
#41280 = CARTESIAN_POINT ( 'NONE',  ( -170.8336150310144887, -175.3837268820161057, 25.58083653558494319 ) ) ;
#41281 = DIRECTION ( 'NONE',  ( -1.000000000000000000, 0.000000000000000000, 0.000000000000000000 ) ) ;
#41282 = AXIS2_PLACEMENT_3D ( 'NONE', #35285, #28425, #27911 ) ;
#41283 = CARTESIAN_POINT ( 'NONE',  ( -48.47912675150885065, -193.5000000000000000, 124.0000000000000142 ) ) ;
#41284 = EDGE_LOOP ( 'NONE', ( #36471, #40703, #2450, #48999 ) ) ;
#41285 = DIRECTION ( 'NONE',  ( -0.000000000000000000, 1.000000000000000000, -0.000000000000000000 ) ) ;
#41286 = FACE_OUTER_BOUND ( 'NONE', #34597, .T. ) ;
#41287 = PLANE ( 'NONE',  #5106 ) ;
#41288 = CARTESIAN_POINT ( 'NONE',  ( 26.70958190211001337, -193.5000000000000000, -99.85818990449013199 ) ) ;
#41289 = AXIS2_PLACEMENT_3D ( 'NONE', #18176, #49480, #34203 ) ;
#41290 = DIRECTION ( 'NONE',  ( 0.000000000000000000, 1.000000000000000000, -0.000000000000000000 ) ) ;
#41291 = AXIS2_PLACEMENT_3D ( 'NONE', #45445, #12844, #9436 ) ;
#41292 = VECTOR ( 'NONE', #7719, 1000.000000000000000 ) ;
#41293 = DIRECTION ( 'NONE',  ( 0.000000000000000000, 0.000000000000000000, 1.000000000000000000 ) ) ;
#41294 = CYLINDRICAL_SURFACE ( 'NONE', #48039, 125.0000000000000000 ) ;
#41296 = VERTEX_POINT ( 'NONE', #48853 ) ;
#41295 = LINE ( 'NONE', #49980, #18643 ) ;
#41297 = VERTEX_POINT ( 'NONE', #20723 ) ;
#41298 = EDGE_CURVE ( 'NONE', #13171, #39625, #40571, .T. ) ;
#41299 = EDGE_CURVE ( 'NONE', #38717, #49425, #13361, .T. ) ;
#41300 = DIRECTION ( 'NONE',  ( -0.000000000000000000, 1.000000000000000000, -0.000000000000000000 ) ) ;
#41301 = CARTESIAN_POINT ( 'NONE',  ( -64.08700758308647494, -175.3837268820161057, -124.0217483183786840 ) ) ;
#41303 = ORIENTED_EDGE ( 'NONE', *, *, #46863, .T. ) ;
#41302 = CARTESIAN_POINT ( 'NONE',  ( -4.525132525065792777, -175.3837268820161057, 115.9484881370938325 ) ) ;
#41304 = VERTEX_POINT ( 'NONE', #24402 ) ;
#41305 = ORIENTED_EDGE ( 'NONE', *, *, #21997, .F. ) ;
#41306 = DIRECTION ( 'NONE',  ( 0.000000000000000000, -0.000000000000000000, 1.000000000000000000 ) ) ;
#41307 = VECTOR ( 'NONE', #42774, 1000.000000000000000 ) ;
#41308 = EDGE_CURVE ( 'NONE', #43501, #29348, #4435, .T. ) ;
#41309 = CARTESIAN_POINT ( 'NONE',  ( -238.7407812814481076, -193.5000000000000000, -41.45482488023466061 ) ) ;
#41310 = CARTESIAN_POINT ( 'NONE',  ( -339.1964088526558498, -109.6270296344165160, -58.37414404713479854 ) ) ;
#41311 = VERTEX_POINT ( 'NONE', #50404 ) ;
#41312 = EDGE_CURVE ( 'NONE', #50099, #37367, #2563, .T. ) ;
#41313 = VECTOR ( 'NONE', #19978, 1000.000000000000000 ) ;
#41314 = LINE ( 'NONE', #16654, #49562 ) ;
#41316 = EDGE_LOOP ( 'NONE', ( #18578, #48507, #18140, #31233 ) ) ;
#41315 = DIRECTION ( 'NONE',  ( 0.7175072570443348230, 0.000000000000000000, -0.6965510290629933765 ) ) ;
#41317 = ADVANCED_FACE ( 'NONE', ( #2314 ), #25957, .T. ) ;
#41318 = CARTESIAN_POINT ( 'NONE',  ( -168.8371699641976704, -189.7472609257535510, 33.74820638215506108 ) ) ;
#41319 = ORIENTED_EDGE ( 'NONE', *, *, #51631, .T. ) ;
#41320 = LINE ( 'NONE', #1388, #31404 ) ;
#41321 = EDGE_CURVE ( 'NONE', #1001, #15941, #18591, .T. ) ;
#41322 = VERTEX_POINT ( 'NONE', #49880 ) ;
#41323 = CARTESIAN_POINT ( 'NONE',  ( -163.3872488209693756, -183.6283474603465606, -49.20491319441543254 ) ) ;
#41324 = CARTESIAN_POINT ( 'NONE',  ( 68.59638248015004081, -193.5000000000000000, -43.79868877201405297 ) ) ;
#41325 = CARTESIAN_POINT ( 'NONE',  ( -128.2395503755045638, -177.1207230881787780, -96.24590808611419845 ) ) ;
#41326 = AXIS2_PLACEMENT_3D ( 'NONE', #10216, #17356, #9452 ) ;
#41327 = VECTOR ( 'NONE', #20328, 1000.000000000000000 ) ;
#41328 = VERTEX_POINT ( 'NONE', #18348 ) ;
#41329 = EDGE_CURVE ( 'NONE', #19650, #46727, #46456, .T. ) ;
#41330 = CIRCLE ( 'NONE', #32103, 125.0000000000000000 ) ;
#41331 = VERTEX_POINT ( 'NONE', #34364 ) ;
#41332 = AXIS2_PLACEMENT_3D ( 'NONE', #45823, #49772, #14025 ) ;
#41333 = CARTESIAN_POINT ( 'NONE',  ( -48.53836737940255119, -177.1207230881787780, -0.9982437317643153563 ) ) ;
#41334 = LINE ( 'NONE', #37918, #40101 ) ;
#41335 = EDGE_LOOP ( 'NONE', ( #6580, #9463, #39161, #43233 ) ) ;
#41336 = DIRECTION ( 'NONE',  ( -0.6965510290629982615, 0.000000000000000000, 0.7175072570443298270 ) ) ;
#41337 = ORIENTED_EDGE ( 'NONE', *, *, #9309, .T. ) ;
#41338 = DIRECTION ( 'NONE',  ( -0.000000000000000000, 1.000000000000000000, -0.000000000000000000 ) ) ;
#41339 = AXIS2_PLACEMENT_3D ( 'NONE', #18376, #7565, #30690 ) ;
#41340 = DIRECTION ( 'NONE',  ( 0.000000000000000000, 0.000000000000000000, 1.000000000000000000 ) ) ;
#41341 = VERTEX_POINT ( 'NONE', #29633 ) ;
#41342 = CARTESIAN_POINT ( 'NONE',  ( -23.01747912075237679, -183.6283474603465606, -122.3793467049370776 ) ) ;
#41343 = EDGE_LOOP ( 'NONE', ( #15833, #29712, #30243, #22161 ) ) ;
#41344 = DIRECTION ( 'NONE',  ( 0.000000000000000000, 0.000000000000000000, 1.000000000000000000 ) ) ;
#41345 = DIRECTION ( 'NONE',  ( 0.000000000000000000, 0.000000000000000000, 1.000000000000000000 ) ) ;
#41346 = EDGE_LOOP ( 'NONE', ( #22446, #2154, #42274, #1510 ) ) ;
#41347 = VECTOR ( 'NONE', #51702, 1000.000000000000000 ) ;
#41348 = CARTESIAN_POINT ( 'NONE',  ( -47.60339180931321579, -193.5000000000000000, 0.4827922027307559594 ) ) ;
#41349 = DIRECTION ( 'NONE',  ( -0.000000000000000000, -0.1205366802553130001, 0.9927088740980551940 ) ) ;
#41350 = DIRECTION ( 'NONE',  ( 0.000000000000000000, 0.1205366802553337752, 0.9927088740980526405 ) ) ;
#41351 = LINE ( 'NONE', #45328, #1396 ) ;
#41352 = AXIS2_PLACEMENT_3D ( 'NONE', #12604, #8667, #24691 ) ;
#41353 = ORIENTED_EDGE ( 'NONE', *, *, #11455, .F. ) ;
#41354 = LINE ( 'NONE', #549, #12721 ) ;
#41355 = EDGE_LOOP ( 'NONE', ( #152, #26191, #19835, #34837 ) ) ;
#41356 = EDGE_CURVE ( 'NONE', #36397, #4130, #29667, .T. ) ;
#41357 = ORIENTED_EDGE ( 'NONE', *, *, #10218, .T. ) ;
#41358 = DIRECTION ( 'NONE',  ( -1.000000000000000000, 0.000000000000000000, 0.000000000000000000 ) ) ;
#41360 = ORIENTED_EDGE ( 'NONE', *, *, #7959, .F. ) ;
#41359 = DIRECTION ( 'NONE',  ( 0.000000000000000000, -1.000000000000000000, 0.000000000000000000 ) ) ;
#41361 = EDGE_CURVE ( 'NONE', #27201, #29477, #26464, .T. ) ;
#41362 = ORIENTED_EDGE ( 'NONE', *, *, #250, .F. ) ;
#41363 = ADVANCED_FACE ( 'NONE', ( #14395 ), #46714, .T. ) ;
#41364 = DIRECTION ( 'NONE',  ( -0.000000000000000000, 0.1205366802553337752, 0.9927088740980526405 ) ) ;
#41365 = EDGE_CURVE ( 'NONE', #41564, #19062, #9673, .T. ) ;
#41366 = VECTOR ( 'NONE', #22626, 1000.000000000000000 ) ;
#41367 = VECTOR ( 'NONE', #22582, 1000.000000000000000 ) ;
#41368 = EDGE_CURVE ( 'NONE', #34268, #3435, #33761, .T. ) ;
#41369 = PLANE ( 'NONE',  #43051 ) ;
#41370 = AXIS2_PLACEMENT_3D ( 'NONE', #25029, #44473, #1090 ) ;
#41371 = ORIENTED_EDGE ( 'NONE', *, *, #15210, .F. ) ;
#41372 = DIRECTION ( 'NONE',  ( 0.000000000000000000, -0.1205366802553199113, 0.9927088740980544168 ) ) ;
#41373 = EDGE_CURVE ( 'NONE', #30848, #2316, #22549, .T. ) ;
#41374 = ORIENTED_EDGE ( 'NONE', *, *, #3980, .T. ) ;
#41375 = DIRECTION ( 'NONE',  ( 0.000000000000000000, 2.775557561562891351E-15, 1.000000000000000000 ) ) ;
#41376 = DIRECTION ( 'NONE',  ( 1.000000000000000000, 0.000000000000000000, 0.000000000000000000 ) ) ;
#41377 = VECTOR ( 'NONE', #27778, 1000.000000000000000 ) ;
#41378 = EDGE_CURVE ( 'NONE', #26043, #15315, #29896, .T. ) ;
#41379 = DIRECTION ( 'NONE',  ( -0.000000000000000000, 1.000000000000000000, -0.000000000000000000 ) ) ;
#41380 = CARTESIAN_POINT ( 'NONE',  ( -332.3517673607765914, -160.6539403396202772, 45.90766452162722544 ) ) ;
#41381 = VERTEX_POINT ( 'NONE', #6250 ) ;
#41382 = ORIENTED_EDGE ( 'NONE', *, *, #39729, .F. ) ;
#41383 = EDGE_CURVE ( 'NONE', #7384, #1606, #45955, .T. ) ;
#41384 = EDGE_LOOP ( 'NONE', ( #4609, #50662, #29702, #40087 ) ) ;
#41385 = DIRECTION ( 'NONE',  ( 0.3758275821142292861, 0.000000000000000000, 0.9266896074318371479 ) ) ;
#41386 = DIRECTION ( 'NONE',  ( -0.1476465640024779702, 0.000000000000000000, -0.9890401873221644768 ) ) ;
#41387 = EDGE_CURVE ( 'NONE', #27746, #41391, #41981, .T. ) ;
#41388 = LINE ( 'NONE', #49296, #50546 ) ;
#41389 = CARTESIAN_POINT ( 'NONE',  ( -114.1105527140175155, -183.6283474603465606, 106.3838142112217611 ) ) ;
#41390 = AXIS2_PLACEMENT_3D ( 'NONE', #16152, #40043, #39005 ) ;
#41391 = VERTEX_POINT ( 'NONE', #17819 ) ;
#41392 = EDGE_CURVE ( 'NONE', #23203, #25253, #5991, .T. ) ;
#41393 = ADVANCED_FACE ( 'NONE', ( #2035 ), #50922, .T. ) ;
#41394 = CIRCLE ( 'NONE', #11152, 125.0000000000000000 ) ;
#41395 = EDGE_CURVE ( 'NONE', #46485, #47175, #18077, .T. ) ;
#41396 = ORIENTED_EDGE ( 'NONE', *, *, #23448, .T. ) ;
#41398 = ORIENTED_EDGE ( 'NONE', *, *, #51304, .F. ) ;
#41397 = PLANE ( 'NONE',  #22303 ) ;
#41399 = EDGE_LOOP ( 'NONE', ( #26948, #6842, #19262, #29961 ) ) ;
#41400 = DIRECTION ( 'NONE',  ( 0.000000000000000000, -1.000000000000000000, -0.000000000000000000 ) ) ;
#41401 = DIRECTION ( 'NONE',  ( 0.000000000000000000, 0.000000000000000000, 1.000000000000000000 ) ) ;
#41402 = DIRECTION ( 'NONE',  ( 0.7765238627180393038, 0.000000000000000000, 0.6300878435817147682 ) ) ;
#41403 = DIRECTION ( 'NONE',  ( 0.9027978299657446470, 0.000000000000000000, -0.4300652022765183435 ) ) ;
#41404 = ORIENTED_EDGE ( 'NONE', *, *, #6704, .T. ) ;
#41405 = DIRECTION ( 'NONE',  ( -0.000000000000000000, 1.000000000000000000, -0.000000000000000000 ) ) ;
#41406 = AXIS2_PLACEMENT_3D ( 'NONE', #50263, #41847, #5863 ) ;
#41407 = ORIENTED_EDGE ( 'NONE', *, *, #12826, .F. ) ;
#41408 = ADVANCED_FACE ( 'NONE', ( #14149 ), #2813, .T. ) ;
#41409 = EDGE_LOOP ( 'NONE', ( #6512, #38946, #22163, #8672 ) ) ;
#41410 = PLANE ( 'NONE',  #10299 ) ;
#41411 = VECTOR ( 'NONE', #18842, 1000.000000000000000 ) ;
#41412 = DIRECTION ( 'NONE',  ( -0.000000000000000000, 1.000000000000000000, -0.000000000000000000 ) ) ;
#41413 = ORIENTED_EDGE ( 'NONE', *, *, #47195, .F. ) ;
#41414 = LINE ( 'NONE', #1482, #30659 ) ;
#41415 = CARTESIAN_POINT ( 'NONE',  ( -28.86423599357335590, -193.5000000000000000, 122.4396006697296002 ) ) ;
#41416 = DIRECTION ( 'NONE',  ( 0.000000000000000000, 0.000000000000000000, -1.000000000000000000 ) ) ;
#41417 = CARTESIAN_POINT ( 'NONE',  ( -336.3521761649654422, -66.84438072661991725, -16.67542351306652648 ) ) ;
#41418 = DIRECTION ( 'NONE',  ( 1.000000000000000000, -0.000000000000000000, -0.000000000000000000 ) ) ;
#41419 = FACE_BOUND ( 'NONE', #3591, .T. ) ;
#41420 = ORIENTED_EDGE ( 'NONE', *, *, #29783, .T. ) ;
#41421 = CARTESIAN_POINT ( 'NONE',  ( -48.47912675150885065, -183.6283474603465606, 6.938893903907228378E-15 ) ) ;
#41422 = ORIENTED_EDGE ( 'NONE', *, *, #34227, .T. ) ;
#41423 = CIRCLE ( 'NONE', #49017, 15.00000000000000000 ) ;
#41424 = EDGE_CURVE ( 'NONE', #17362, #34406, #43543, .T. ) ;
#41425 = ORIENTED_EDGE ( 'NONE', *, *, #47873, .F. ) ;
#41426 = ADVANCED_FACE ( 'NONE', ( #43789 ), #19368, .T. ) ;
#41427 = DIRECTION ( 'NONE',  ( 0.000000000000000000, -0.5680647467311457088, 0.8229838658936633466 ) ) ;
#41428 = ORIENTED_EDGE ( 'NONE', *, *, #15984, .T. ) ;
#41429 = VECTOR ( 'NONE', #6787, 1000.000000000000000 ) ;
#41430 = ADVANCED_FACE ( 'NONE', ( #51188 ), #26983, .T. ) ;
#41431 = EDGE_CURVE ( 'NONE', #1552, #4433, #23325, .T. ) ;
#41432 = LINE ( 'NONE', #37751, #21775 ) ;
#41433 = DIRECTION ( 'NONE',  ( 0.000000000000000000, 0.000000000000000000, 1.000000000000000000 ) ) ;
#41435 = ORIENTED_EDGE ( 'NONE', *, *, #45786, .F. ) ;
#41434 = DIRECTION ( 'NONE',  ( -0.6965510290629882695, 0.000000000000000000, -0.7175072570443395970 ) ) ;
#41437 = VECTOR ( 'NONE', #11772, 1000.000000000000227 ) ;
#41436 = DIRECTION ( 'NONE',  ( 0.000000000000000000, 1.000000000000000000, -0.000000000000000000 ) ) ;
#41438 = ORIENTED_EDGE ( 'NONE', *, *, #43281, .F. ) ;
#41439 = ORIENTED_EDGE ( 'NONE', *, *, #45564, .T. ) ;
#41440 = ORIENTED_EDGE ( 'NONE', *, *, #5689, .T. ) ;
#41441 = DIRECTION ( 'NONE',  ( 0.000000000000000000, 0.000000000000000000, -1.000000000000000000 ) ) ;
#41442 = CARTESIAN_POINT ( 'NONE',  ( 74.77174840718836890, -177.1207230881787780, 20.83798868929603998 ) ) ;
#41443 = EDGE_CURVE ( 'NONE', #3937, #38180, #46980, .T. ) ;
#41444 = ORIENTED_EDGE ( 'NONE', *, *, #13016, .F. ) ;
#41445 = LINE ( 'NONE', #5731, #10207 ) ;
#41446 = DIRECTION ( 'NONE',  ( -0.000000000000000000, 1.000000000000000000, -0.000000000000000000 ) ) ;
#41447 = ORIENTED_EDGE ( 'NONE', *, *, #33949, .F. ) ;
#41448 = ADVANCED_FACE ( 'NONE', ( #35382 ), #35644, .F. ) ;
#41449 = DIRECTION ( 'NONE',  ( -0.000000000000000000, 0.8854560256532093554, -0.4647231720437695057 ) ) ;
#41450 = DIRECTION ( 'NONE',  ( 0.4031234292879600778, 0.000000000000000000, 0.9151456172430237901 ) ) ;
#41452 = ORIENTED_EDGE ( 'NONE', *, *, #25963, .T. ) ;
#41451 = DIRECTION ( 'NONE',  ( -0.000000000000000000, 1.000000000000000000, -0.000000000000000000 ) ) ;
#41453 = VERTEX_POINT ( 'NONE', #14925 ) ;
#41454 = VERTEX_POINT ( 'NONE', #39064 ) ;
#41455 = CARTESIAN_POINT ( 'NONE',  ( -47.48307690889363641, -175.3837268820161057, -0.08879589532292464504 ) ) ;
#41456 = CARTESIAN_POINT ( 'NONE',  ( -238.7407812814481076, -193.5000000000000000, 10.00000000000000178 ) ) ;
#41457 = CIRCLE ( 'NONE', #30542, 125.0000000000000000 ) ;
#41458 = EDGE_LOOP ( 'NONE', ( #40825, #27521, #19877, #11889 ) ) ;
#41459 = AXIS2_PLACEMENT_3D ( 'NONE', #24415, #11552, #4445 ) ;
#41460 = DIRECTION ( 'NONE',  ( 0.000000000000000000, -0.000000000000000000, -1.000000000000000000 ) ) ;
#41461 = LINE ( 'NONE', #25701, #51931 ) ;
#41462 = ORIENTED_EDGE ( 'NONE', *, *, #6029, .F. ) ;
#41463 = DIRECTION ( 'NONE',  ( 0.000000000000000000, 0.000000000000000000, 1.000000000000000000 ) ) ;
#41464 = ORIENTED_EDGE ( 'NONE', *, *, #3448, .F. ) ;
#41465 = AXIS2_PLACEMENT_3D ( 'NONE', #29845, #21966, #37987 ) ;
#41466 = EDGE_LOOP ( 'NONE', ( #49949, #34285, #47959, #48353 ) ) ;
#41467 = DIRECTION ( 'NONE',  ( 0.000000000000000000, 0.000000000000000000, 1.000000000000000000 ) ) ;
#41468 = LINE ( 'NONE', #33072, #34074 ) ;
#41469 = CARTESIAN_POINT ( 'NONE',  ( -330.4913330509368166, -64.86990808808705822, 6.615309698014281814 ) ) ;
#41470 = SURFACE_SIDE_STYLE ('',( #41746 ) ) ;
#41471 = VERTEX_POINT ( 'NONE', #48000 ) ;
#41472 = CARTESIAN_POINT ( 'NONE',  ( -238.7407812814481076, -213.5000000000000000, -41.45482488023466061 ) ) ;
#41473 = DIRECTION ( 'NONE',  ( 0.000000000000000000, 0.000000000000000000, -1.000000000000000000 ) ) ;
#41474 = ITEM_DEFINED_TRANSFORMATION ( 'NONE', 'NONE', #4105,  #31742 ) ;
#41475 = EDGE_CURVE ( 'NONE', #30907, #34863, #7542, .T. ) ;
#41476 = DIRECTION ( 'NONE',  ( -0.000000000000000000, 1.000000000000000000, -0.000000000000000000 ) ) ;
#41477 = FACE_OUTER_BOUND ( 'NONE', #37610, .T. ) ;
#41478 = AXIS2_PLACEMENT_3D ( 'NONE', #42694, #22477, #26132 ) ;
#41479 = FACE_OUTER_BOUND ( 'NONE', #13732, .T. ) ;
#41480 = DIRECTION ( 'NONE',  ( -0.000000000000000000, 1.000000000000000000, -0.000000000000000000 ) ) ;
#41481 = FACE_OUTER_BOUND ( 'NONE', #30651, .T. ) ;
#41482 = ORIENTED_EDGE ( 'NONE', *, *, #48303, .T. ) ;
#41483 = DIRECTION ( 'NONE',  ( -0.02963332782257007553, 0.000000000000000000, 0.9995608365087941261 ) ) ;
#41484 = CARTESIAN_POINT ( 'NONE',  ( -48.30223647638628393, -183.6283474603465606, 0.9842305779476049343 ) ) ;
#41485 = EDGE_LOOP ( 'NONE', ( #12112, #44441, #8888, #6155 ) ) ;
#41486 = EDGE_CURVE ( 'NONE', #4051, #47336, #36164, .T. ) ;
#41487 = EDGE_CURVE ( 'NONE', #25456, #13663, #15438, .T. ) ;
#41488 = EDGE_LOOP ( 'NONE', ( #8507, #32892, #19654, #33980 ) ) ;
#41489 = VERTEX_POINT ( 'NONE', #47487 ) ;
#41490 = CARTESIAN_POINT ( 'NONE',  ( -130.0559183202350084, -175.3837268820161057, -93.38753978496592367 ) ) ;
#41491 = CARTESIAN_POINT ( 'NONE',  ( 18.00181100848376303, -177.1207230881787780, -105.8550183720733742 ) ) ;
#41492 = LINE ( 'NONE', #8931, #48917 ) ;
#41493 = LINE ( 'NONE', #29410, #27025 ) ;
#41494 = VECTOR ( 'NONE', #40220, 1000.000000000000000 ) ;
#41495 = AXIS2_PLACEMENT_3D ( 'NONE', #28351, #44404, #8389 ) ;
#41496 = LINE ( 'NONE', #4737, #29992 ) ;
#41497 = FACE_OUTER_BOUND ( 'NONE', #38937, .T. ) ;
#41498 = VERTEX_POINT ( 'NONE', #11470 ) ;
#41499 = VECTOR ( 'NONE', #50809, 1000.000000000000227 ) ;
#41500 = LINE ( 'NONE', #40719, #48307 ) ;
#41501 = ORIENTED_EDGE ( 'NONE', *, *, #39701, .T. ) ;
#41502 = DIRECTION ( 'NONE',  ( 0.000000000000000000, 0.000000000000000000, -1.000000000000000000 ) ) ;
#41503 = VERTEX_POINT ( 'NONE', #43016 ) ;
#41504 = EDGE_CURVE ( 'NONE', #14763, #22171, #19881, .T. ) ;
#41505 = CARTESIAN_POINT ( 'NONE',  ( -336.3521761649654422, -80.42027357919624819, -40.34602258462219027 ) ) ;
#41506 = ORIENTED_EDGE ( 'NONE', *, *, #21099, .T. ) ;
#41507 = AXIS2_PLACEMENT_3D ( 'NONE', #12680, #12938, #28966 ) ;
#41508 = EDGE_CURVE ( 'NONE', #51805, #15063, #6203, .T. ) ;
#41509 = PRODUCT_DEFINITION_SHAPE ( 'NONE', 'NONE',  #1043 ) ;
#41510 = CARTESIAN_POINT ( 'NONE',  ( -332.3517673607765914, -97.97423230103774472, -54.29949524055093946 ) ) ;
#41511 = ORIENTED_EDGE ( 'NONE', *, *, #34958, .T. ) ;
#41514 = VERTEX_POINT ( 'NONE', #39832 ) ;
#41513 = DIRECTION ( 'NONE',  ( 0.000000000000000000, 0.000000000000000000, 1.000000000000000000 ) ) ;
#41512 = CARTESIAN_POINT ( 'NONE',  ( -330.4913330509368166, -108.8949048983213004, -57.16590939599337418 ) ) ;
#41515 = CARTESIAN_POINT ( 'NONE',  ( -330.4913330509368166, -167.3305728129748786, -39.49849221029221269 ) ) ;
#41516 = ORIENTED_EDGE ( 'NONE', *, *, #33675, .T. ) ;
#41517 = DIRECTION ( 'NONE',  ( 0.5586467658036476935, 0.000000000000000000, 0.8294056854502049880 ) ) ;
#41518 = ORIENTED_EDGE ( 'NONE', *, *, #40768, .F. ) ;
#41519 = EDGE_CURVE ( 'NONE', #51413, #46129, #25474, .T. ) ;
#41520 = DIRECTION ( 'NONE',  ( 0.000000000000000000, 1.000000000000000000, 0.000000000000000000 ) ) ;
#41523 = VERTEX_POINT ( 'NONE', #11981 ) ;
#41522 = CARTESIAN_POINT ( 'NONE',  ( 4.109287492203100634, -183.6283474603465606, -113.3995532942336979 ) ) ;
#41521 = CARTESIAN_POINT ( 'NONE',  ( 71.73509643893275722, -177.1207230881787780, -30.40954281680804172 ) ) ;
#41524 = ORIENTED_EDGE ( 'NONE', *, *, #33684, .T. ) ;
#41525 = CARTESIAN_POINT ( 'NONE',  ( -339.1964088526558498, -175.9742670995615015, -26.97593913775538965 ) ) ;
#41526 = FACE_OUTER_BOUND ( 'NONE', #7126, .T. ) ;
#41527 = AXIS2_PLACEMENT_3D ( 'NONE', #41209, #20995, #37016 ) ;
#41528 = CARTESIAN_POINT ( 'NONE',  ( -58.29063029684667185, -183.6283474603465606, 124.6143426664034877 ) ) ;
#41529 = VERTEX_POINT ( 'NONE', #28012 ) ;
#41530 = CARTESIAN_POINT ( 'NONE',  ( -339.1964088526558498, -123.9999999999993747, 59.00000000000002132 ) ) ;
#41531 = PLANE ( 'NONE',  #25138 ) ;
#41532 = AXIS2_PLACEMENT_3D ( 'NONE', #41198, #49372, #1529 ) ;
#41533 = CARTESIAN_POINT ( 'NONE',  ( 21.49274850782853363, -189.7472609257535510, -103.5805805771126415 ) ) ;
#41534 = AXIS2_PLACEMENT_3D ( 'NONE', #13893, #14940, #30947 ) ;
#41535 = VERTEX_POINT ( 'NONE', #15175 ) ;
#41536 = CARTESIAN_POINT ( 'NONE',  ( -41.24387117724851493, -193.5000000000000000, 124.7904286264581231 ) ) ;
#41538 = CIRCLE ( 'NONE', #42365, 125.0000000000000000 ) ;
#41537 = DIRECTION ( 'NONE',  ( -0.000000000000000000, -1.000000000000000000, -0.000000000000000000 ) ) ;
#41539 = EDGE_CURVE ( 'NONE', #8243, #29433, #2807, .T. ) ;
#41540 = CARTESIAN_POINT ( 'NONE',  ( 0.000000000000000000, 106.9200652401092526, -109.8944711476178213 ) ) ;
#41541 = ORIENTED_EDGE ( 'NONE', *, *, #11888, .F. ) ;
#41542 = CARTESIAN_POINT ( 'NONE',  ( -336.3521761649653854, -114.6500883362968892, 59.34373651485599055 ) ) ;
#41543 = LINE ( 'NONE', #22363, #16875 ) ;
#41544 = AXIS2_PLACEMENT_3D ( 'NONE', #38086, #50460, #34156 ) ;
#41545 = VECTOR ( 'NONE', #37176, 999.9999999999998863 ) ;
#41546 = DIRECTION ( 'NONE',  ( -0.000000000000000000, 1.000000000000000000, -0.000000000000000000 ) ) ;
#41547 = DIRECTION ( 'NONE',  ( -0.5338233779647887367, 0.000000000000000000, -0.8455960035018273979 ) ) ;
#41548 = EDGE_CURVE ( 'NONE', #40230, #45352, #31187, .T. ) ;
#41549 = CIRCLE ( 'NONE', #49974, 125.0000000000000000 ) ;
#41550 = DIRECTION ( 'NONE',  ( 0.000000000000000000, 1.000000000000000000, 0.000000000000000000 ) ) ;
#41551 = AXIS2_PLACEMENT_3D ( 'NONE', #42283, #17629, #45477 ) ;
#41552 = EDGE_CURVE ( 'NONE', #24129, #48198, #43274, .T. ) ;
#41553 = DIRECTION ( 'NONE',  ( -0.000000000000000000, -0.000000000000000000, 1.000000000000000000 ) ) ;
#41554 = CARTESIAN_POINT ( 'NONE',  ( -47.82630463331833681, -189.7472609257535510, 0.7575112421616305713 ) ) ;
#41556 = ORIENTED_EDGE ( 'NONE', *, *, #44039, .F. ) ;
#41555 = CARTESIAN_POINT ( 'NONE',  ( 2.669657140899374337, -189.7472609257535510, 114.0561348912355868 ) ) ;
#41557 = VERTEX_POINT ( 'NONE', #1189 ) ;
#41558 = CARTESIAN_POINT ( 'NONE',  ( -336.3521761649654422, -180.3949349376675855, 15.70448169564087770 ) ) ;
#41559 = CARTESIAN_POINT ( 'NONE',  ( -166.9790462269951945, -177.1207230881787780, 36.52255268223134266 ) ) ;
#41561 = ORIENTED_EDGE ( 'NONE', *, *, #3184, .T. ) ;
#41560 = CARTESIAN_POINT ( 'NONE',  ( -49.32472275501068282, -183.6283474603465606, 0.5338233779647895139 ) ) ;
#41562 = EDGE_LOOP ( 'NONE', ( #35515, #40123, #15625, #22232 ) ) ;
#41563 = AXIS2_PLACEMENT_3D ( 'NONE', #18929, #46800, #3158 ) ;
#41564 = VERTEX_POINT ( 'NONE', #17243 ) ;
#41565 = EDGE_CURVE ( 'NONE', #43598, #20384, #35543, .T. ) ;
#41566 = CARTESIAN_POINT ( 'NONE',  ( -123.4791267515088435, -173.5000000000000284, 70.00000000000000000 ) ) ;
#41567 = AXIS2_PLACEMENT_3D ( 'NONE', #42112, #2172, #25834 ) ;
#41568 = VECTOR ( 'NONE', #14231, 1000.000000000000000 ) ;
#41569 = CARTESIAN_POINT ( 'NONE',  ( -330.4913330509368166, -180.6659093959932250, 14.60509510167933556 ) ) ;
#41570 = DIRECTION ( 'NONE',  ( 0.000000000000000000, 0.000000000000000000, -1.000000000000000000 ) ) ;
#41571 = ORIENTED_EDGE ( 'NONE', *, *, #43586, .T. ) ;
#41572 = VECTOR ( 'NONE', #12005, 1000.000000000000000 ) ;
#41573 = DIRECTION ( 'NONE',  ( -0.000000000000000000, -1.000000000000000000, -0.000000000000000000 ) ) ;
#41575 = ORIENTED_EDGE ( 'NONE', *, *, #21450, .T. ) ;
#41574 = CARTESIAN_POINT ( 'NONE',  ( -47.82630463331832971, -177.1207230881787780, -0.7575112421616121416 ) ) ;
#41576 = AXIS2_PLACEMENT_3D ( 'NONE', #31435, #22787, #34598 ) ;
#41577 = AXIS2_PLACEMENT_3D ( 'NONE', #5008, #29163, #17618 ) ;
#41578 = DIRECTION ( 'NONE',  ( -0.000000000000000000, 1.000000000000000000, -0.000000000000000000 ) ) ;
#41579 = VERTEX_POINT ( 'NONE', #28279 ) ;
#41580 = DIRECTION ( 'NONE',  ( 0.000000000000000000, 1.000000000000000000, 0.000000000000000000 ) ) ;
#41581 = VERTEX_POINT ( 'NONE', #49309 ) ;
#41582 = LINE ( 'NONE', #41323, #3966 ) ;
#41583 = AXIS2_PLACEMENT_3D ( 'NONE', #10124, #34540, #43204 ) ;
#41584 = DIRECTION ( 'NONE',  ( -1.000000000000000000, -5.928974370888934796E-15, -8.589602288500814192E-15 ) ) ;
#41585 = CARTESIAN_POINT ( 'NONE',  ( 37.99238433767461487, -189.7472609257535510, -90.26448786734026442 ) ) ;
#41586 = AXIS2_PLACEMENT_3D ( 'NONE', #51125, #14855, #43200 ) ;
#41587 = VERTEX_POINT ( 'NONE', #28780 ) ;
#41588 = ORIENTED_EDGE ( 'NONE', *, *, #40971, .F. ) ;
#41589 = DIRECTION ( 'NONE',  ( 0.5338233779647826305, 0.000000000000000000, 0.8455960035018311727 ) ) ;
#41590 = DIRECTION ( 'NONE',  ( -0.000000000000000000, -0.4647231720437604574, 0.8854560256532141294 ) ) ;
#41591 = VERTEX_POINT ( 'NONE', #33266 ) ;
#41592 = CARTESIAN_POINT ( 'NONE',  ( -339.1964088526558498, -65.12585595286530804, -13.87297036558381080 ) ) ;
#41593 = EDGE_CURVE ( 'NONE', #44250, #25303, #32745, .T. ) ;
#41594 = ADVANCED_FACE ( 'NONE', ( #4905 ), #20931, .F. ) ;
#41595 = ORIENTED_EDGE ( 'NONE', *, *, #1585, .F. ) ;
#41596 = LINE ( 'NONE', #45566, #35948 ) ;
#41597 = CARTESIAN_POINT ( 'NONE',  ( -336.3521761649654422, -179.5993808087905279, -18.46045550523168899 ) ) ;
#41598 = ORIENTED_EDGE ( 'NONE', *, *, #46138, .T. ) ;
#41599 = DIRECTION ( 'NONE',  ( -0.000000000000000000, 0.5680647467311457088, -0.8229838658936633466 ) ) ;
#41600 = ORIENTED_EDGE ( 'NONE', *, *, #6080, .T. ) ;
#41601 = CIRCLE ( 'NONE', #1319, 125.0000000000000000 ) ;
#41602 = FACE_OUTER_BOUND ( 'NONE', #44444, .T. ) ;
#41603 = DIRECTION ( 'NONE',  ( -0.000000000000000000, 0.1205366802553303196, 0.9927088740980530845 ) ) ;
#41604 = DIRECTION ( 'NONE',  ( 0.000000000000000000, 0.000000000000000000, 1.000000000000000000 ) ) ;
#41605 = VERTEX_POINT ( 'NONE', #36414 ) ;
#41606 = VECTOR ( 'NONE', #47306, 1000.000000000000000 ) ;
#41607 = CONICAL_SURFACE ( 'NONE', #50896, 15.00000000000000000, 0.7853981633974526089 ) ;
#41608 = CARTESIAN_POINT ( 'NONE',  ( -336.3521761649654422, -123.5000000000000284, 0.000000000000000000 ) ) ;
#41609 = LINE ( 'NONE', #10596, #7923 ) ;
#41610 = DIRECTION ( 'NONE',  ( 0.000000000000000000, 0.9350162426854132791, -0.3546048870425396182 ) ) ;
#41611 = EDGE_CURVE ( 'NONE', #17341, #29772, #32183, .T. ) ;
#41612 = CARTESIAN_POINT ( 'NONE',  ( -117.8923552450418981, -175.3837268820161057, 102.7511748916629415 ) ) ;
#41613 = ADVANCED_FACE ( 'NONE', ( #25385 ), #37200, .F. ) ;
#41614 = VERTEX_POINT ( 'NONE', #24341 ) ;
#41615 = CARTESIAN_POINT ( 'NONE',  ( 61.38599058177057799, -193.5000000000000000, 59.62093586438192006 ) ) ;
#41616 = EDGE_LOOP ( 'NONE', ( #29188, #20513, #4908, #51462 ) ) ;
#41617 = ADVANCED_FACE ( 'NONE', ( #16741 ), #8559, .F. ) ;
#41618 = AXIS2_PLACEMENT_3D ( 'NONE', #45620, #29040, #25621 ) ;
#41619 = DIRECTION ( 'NONE',  ( -1.000000000000000000, 0.000000000000000000, 0.000000000000000000 ) ) ;
#41621 = ORIENTED_EDGE ( 'NONE', *, *, #46537, .T. ) ;
#41620 = DIRECTION ( 'NONE',  ( -0.000000000000000000, -0.4647231720437631775, 0.8854560256532126861 ) ) ;
#41622 = VECTOR ( 'NONE', #22167, 1000.000000000000000 ) ;
#41623 = ORIENTED_EDGE ( 'NONE', *, *, #14060, .F. ) ;
#41624 = CARTESIAN_POINT ( 'NONE',  ( -48.47912675150885065, -177.1207230881787780, 6.938893903907228378E-15 ) ) ;
#41625 = VECTOR ( 'NONE', #27044, 1000.000000000000000 ) ;
#41626 = CIRCLE ( 'NONE', #16473, 15.00000000000000000 ) ;
#41627 = DIRECTION ( 'NONE',  ( 0.000000000000000000, 0.000000000000000000, -1.000000000000000000 ) ) ;
#41628 = ORIENTED_EDGE ( 'NONE', *, *, #49954, .F. ) ;
#41629 = CARTESIAN_POINT ( 'NONE',  ( -1.230335819511603423, -193.5000000000000000, 115.7261930397108216 ) ) ;
#41630 = ORIENTED_EDGE ( 'NONE', *, *, #14374, .F. ) ;
#41631 = DIRECTION ( 'NONE',  ( -0.6528221181905119463, 0.000000000000000000, -0.7575112421616284619 ) ) ;
#41632 = CARTESIAN_POINT ( 'NONE',  ( -16.77927958806651887, -193.5000000000000000, -120.9136869416130082 ) ) ;
#41633 = CARTESIAN_POINT ( 'NONE',  ( -48.98765787015808115, -183.6283474603465606, 0.8610436117673582190 ) ) ;
#41634 = ORIENTED_EDGE ( 'NONE', *, *, #41487, .T. ) ;
#41635 = ORIENTED_EDGE ( 'NONE', *, *, #44006, .F. ) ;
#41636 = VERTEX_POINT ( 'NONE', #21179 ) ;
#41637 = CARTESIAN_POINT ( 'NONE',  ( -332.3517673607765914, -123.5000000000000284, 0.000000000000000000 ) ) ;
#41638 = PLANE ( 'NONE',  #44517 ) ;
#41639 = CIRCLE ( 'NONE', #43334, 125.0000000000000000 ) ;
#41640 = AXIS2_PLACEMENT_3D ( 'NONE', #51450, #11483, #7552 ) ;
#41641 = VECTOR ( 'NONE', #21904, 1000.000000000000341 ) ;
#41642 = CARTESIAN_POINT ( 'NONE',  ( -336.3521761649654422, -160.6539403396202772, 45.90766452162722544 ) ) ;
#41643 = LINE ( 'NONE', #25122, #47379 ) ;
#41644 = ORIENTED_EDGE ( 'NONE', *, *, #23748, .T. ) ;
#41645 = AXIS2_PLACEMENT_3D ( 'NONE', #34596, #30396, #50391 ) ;
#41646 = ORIENTED_EDGE ( 'NONE', *, *, #27334, .T. ) ;
#41648 = ORIENTED_EDGE ( 'NONE', *, *, #24628, .F. ) ;
#41647 = LINE ( 'NONE', #45362, #43310 ) ;
#41649 = PLANE ( 'NONE',  #35539 ) ;
#41650 = ORIENTED_EDGE ( 'NONE', *, *, #14164, .F. ) ;
#41651 = CIRCLE ( 'NONE', #27392, 125.0000000000000000 ) ;
#41652 = DIRECTION ( 'NONE',  ( 0.000000000000000000, -0.000000000000000000, -1.000000000000000000 ) ) ;
#41653 = AXIS2_PLACEMENT_3D ( 'NONE', #32869, #39967, #32093 ) ;
#41654 = DIRECTION ( 'NONE',  ( 0.000000000000000000, 0.000000000000000000, -1.000000000000000000 ) ) ;
#41655 = CIRCLE ( 'NONE', #1375, 125.0000000000000000 ) ;
#41656 = AXIS2_PLACEMENT_3D ( 'NONE', #4853, #28986, #48988 ) ;
#41657 = EDGE_CURVE ( 'NONE', #22956, #3706, #36691, .T. ) ;
#41658 = CARTESIAN_POINT ( 'NONE',  ( -48.47912675150885065, -189.7472609257535510, 6.938893903907228378E-15 ) ) ;
#41659 = EDGE_CURVE ( 'NONE', #51892, #26963, #44571, .T. ) ;
#41660 = EDGE_CURVE ( 'NONE', #40560, #34344, #5419, .T. ) ;
#41661 = DIRECTION ( 'NONE',  ( 0.000000000000000000, -0.000000000000000000, 1.000000000000000000 ) ) ;
#41662 = VERTEX_POINT ( 'NONE', #21434 ) ;
#41663 = DIRECTION ( 'NONE',  ( 0.000000000000000000, 1.063963731932441632E-14, 1.000000000000000000 ) ) ;
#41664 = AXIS2_PLACEMENT_3D ( 'NONE', #6176, #26386, #10361 ) ;
#41665 = ORIENTED_EDGE ( 'NONE', *, *, #13677, .T. ) ;
#41666 = EDGE_CURVE ( 'NONE', #33838, #27596, #12897, .T. ) ;
#41667 = AXIS2_PLACEMENT_3D ( 'NONE', #50785, #22407, #35252 ) ;
#41668 = ORIENTED_EDGE ( 'NONE', *, *, #27435, .T. ) ;
#41669 = CARTESIAN_POINT ( 'NONE',  ( -48.82732838694325750, -193.5000000000000000, 0.9374196611341252261 ) ) ;
#41670 = EDGE_CURVE ( 'NONE', #50927, #38934, #29049, .T. ) ;
#41671 = VECTOR ( 'NONE', #33112, 1000.000000000000000 ) ;
#41672 = DIRECTION ( 'NONE',  ( -0.000000000000000000, -1.000000000000000000, 0.000000000000000000 ) ) ;
#41673 = ORIENTED_EDGE ( 'NONE', *, *, #27600, .F. ) ;
#41674 = EDGE_CURVE ( 'NONE', #19289, #28248, #32919, .T. ) ;
#41675 = LINE ( 'NONE', #29060, #43273 ) ;
#41676 = DIRECTION ( 'NONE',  ( 0.6528221181905227155, 0.000000000000000000, -0.7575112421616191360 ) ) ;
#41677 = CARTESIAN_POINT ( 'NONE',  ( 76.09804998693969935, -175.3837268820161057, 10.27263529369908035 ) ) ;
#41678 = EDGE_CURVE ( 'NONE', #41503, #29039, #9456, .T. ) ;
#41679 = CARTESIAN_POINT ( 'NONE',  ( 0.000000000000000000, -137.6196241929661710, -57.28556722813703317 ) ) ;
#41680 = EDGE_CURVE ( 'NONE', #10587, #19788, #36951, .T. ) ;
#41681 = CARTESIAN_POINT ( 'NONE',  ( -94.25732089370191602, -183.6283474603465606, 116.3157639405754935 ) ) ;
#41682 = FACE_BOUND ( 'NONE', #39868, .T. ) ;
#41683 = EDGE_CURVE ( 'NONE', #2972, #21974, #24594, .T. ) ;
#41684 = VERTEX_POINT ( 'NONE', #20655 ) ;
#41685 = VECTOR ( 'NONE', #43745, 1000.000000000000000 ) ;
#41686 = AXIS2_PLACEMENT_3D ( 'NONE', #26363, #17196, #5372 ) ;
#41687 = EDGE_CURVE ( 'NONE', #51239, #6148, #32992, .T. ) ;
#41688 = LINE ( 'NONE', #45389, #3682 ) ;
#41689 = ORIENTED_EDGE ( 'NONE', *, *, #25722, .F. ) ;
#41690 = AXIS2_PLACEMENT_3D ( 'NONE', #49725, #37100, #17423 ) ;
#41691 = EDGE_CURVE ( 'NONE', #25127, #50038, #5686, .T. ) ;
#41692 = ORIENTED_EDGE ( 'NONE', *, *, #16841, .F. ) ;
#41693 = CARTESIAN_POINT ( 'NONE',  ( 74.00867759460086859, -175.3837268820161057, 24.93467037017223120 ) ) ;
#41694 = ORIENTED_EDGE ( 'NONE', *, *, #10965, .F. ) ;
#41695 = DIRECTION ( 'NONE',  ( -0.000000000000000000, 1.000000000000000000, -0.000000000000000000 ) ) ;
#41696 = VECTOR ( 'NONE', #40861, 1000.000000000000000 ) ;
#41697 = CARTESIAN_POINT ( 'NONE',  ( -47.55243714407702527, -177.1207230881787780, 0.3758275821142491591 ) ) ;
#41698 = AXIS2_PLACEMENT_3D ( 'NONE', #15353, #3269, #7718 ) ;
#41700 = VERTEX_POINT ( 'NONE', #21708 ) ;
#41699 = CARTESIAN_POINT ( 'NONE',  ( 39.18328161278951427, -189.7472609257535510, 89.10837311819236106 ) ) ;
#41701 = VECTOR ( 'NONE', #46848, 1000.000000000000114 ) ;
#41702 = CIRCLE ( 'NONE', #16550, 125.0000000000000000 ) ;
#41703 = VECTOR ( 'NONE', #38721, 1000.000000000000114 ) ;
#41704 = CARTESIAN_POINT ( 'NONE',  ( 33.75048693540708911, -189.7472609257535510, 94.14505102712816154 ) ) ;
#41705 = EDGE_CURVE ( 'NONE', #22275, #11192, #14081, .T. ) ;
#41706 = VERTEX_POINT ( 'NONE', #30097 ) ;
#41707 = ORIENTED_EDGE ( 'NONE', *, *, #6342, .T. ) ;
#41708 = ORIENTED_EDGE ( 'NONE', *, *, #14572, .T. ) ;
#41709 = AXIS2_PLACEMENT_3D ( 'NONE', #12629, #23941, #20516 ) ;
#41710 = DIRECTION ( 'NONE',  ( 0.000000000000000000, 0.000000000000000000, 1.000000000000000000 ) ) ;
#41711 = PLANE ( 'NONE',  #11723 ) ;
#41712 = VERTEX_POINT ( 'NONE', #1723 ) ;
#41713 = DIRECTION ( 'NONE',  ( 0.000000000000000000, 0.000000000000000000, 1.000000000000000000 ) ) ;
#41714 = FACE_OUTER_BOUND ( 'NONE', #22366, .T. ) ;
#41715 = ORIENTED_EDGE ( 'NONE', *, *, #48800, .F. ) ;
#41716 = CARTESIAN_POINT ( 'NONE',  ( 36.19006208304271155, -177.1207230881787780, 90.59430563621340582 ) ) ;
#41717 = ADVANCED_FACE ( 'NONE', ( #37976 ), #50341, .F. ) ;
#41718 = DIRECTION ( 'NONE',  ( 0.000000000000000000, 0.000000000000000000, 1.000000000000000000 ) ) ;
#41719 = EDGE_LOOP ( 'NONE', ( #23141, #37347, #8757, #24851 ) ) ;
#41721 = ORIENTED_EDGE ( 'NONE', *, *, #3112, .F. ) ;
#41720 = CARTESIAN_POINT ( 'NONE',  ( -172.0839188101925004, -175.3837268820161057, -18.62405380494756812 ) ) ;
#41722 = VECTOR ( 'NONE', #24338, 1000.000000000000114 ) ;
#41723 = EDGE_LOOP ( 'NONE', ( #41319, #28373, #29597, #21134 ) ) ;
#41724 = AXIS2_PLACEMENT_3D ( 'NONE', #41288, #37353, #33151 ) ;
#41725 = ORIENTED_EDGE ( 'NONE', *, *, #26229, .F. ) ;
#41726 = FACE_OUTER_BOUND ( 'NONE', #13278, .T. ) ;
#41727 = DIRECTION ( 'NONE',  ( -0.9929810960135169173, 0.000000000000000000, -0.1182731709213660498 ) ) ;
#41728 = ORIENTED_EDGE ( 'NONE', *, *, #6961, .F. ) ;
#41729 = AXIS2_PLACEMENT_3D ( 'NONE', #37703, #37179, #33755 ) ;
#41730 = EDGE_CURVE ( 'NONE', #29042, #30411, #44683, .T. ) ;
#41731 = DIRECTION ( 'NONE',  ( -0.000000000000000000, 0.5680647467311540355, -0.8229838658936575735 ) ) ;
#41732 = EDGE_CURVE ( 'NONE', #21321, #46459, #48894, .T. ) ;
#41733 = EDGE_CURVE ( 'NONE', #13063, #7058, #29832, .T. ) ;
#41734 = DIRECTION ( 'NONE',  ( 0.000000000000000000, 0.000000000000000000, -1.000000000000000000 ) ) ;
#41735 = ORIENTED_EDGE ( 'NONE', *, *, #1569, .T. ) ;
#41736 = CARTESIAN_POINT ( 'NONE',  ( -330.4913330509368166, -75.22798428563942252, 33.92731199008440512 ) ) ;
#41737 = ORIENTED_EDGE ( 'NONE', *, *, #19255, .F. ) ;
#41738 = ADVANCED_FACE ( 'NONE', ( #17763 ), #26143, .F. ) ;
#41739 = ORIENTED_EDGE ( 'NONE', *, *, #33427, .T. ) ;
#41740 = FACE_OUTER_BOUND ( 'NONE', #20173, .T. ) ;
#41741 = CIRCLE ( 'NONE', #35838, 125.0000000000000000 ) ;
#41742 = CARTESIAN_POINT ( 'NONE',  ( -121.5885020763900712, -183.6283474603465606, -101.3904297239421197 ) ) ;
#41743 = AXIS2_PLACEMENT_3D ( 'NONE', #30793, #46837, #26842 ) ;
#41744 = EDGE_CURVE ( 'NONE', #26309, #44752, #46398, .T. ) ;
#41745 = CARTESIAN_POINT ( 'NONE',  ( -332.3517673607765914, -176.5004679656469477, -25.97334715265976612 ) ) ;
#41746 = SURFACE_STYLE_FILL_AREA ( #33851 ) ;
#41747 = ORIENTED_EDGE ( 'NONE', *, *, #46257, .F. ) ;
#41748 = VECTOR ( 'NONE', #28278, 1000.000000000000000 ) ;
#41749 = PLANE ( 'NONE',  #1593 ) ;
#41750 = CARTESIAN_POINT ( 'NONE',  ( -165.1736796818183564, -193.5000000000000000, -41.93543928473608418 ) ) ;
#41751 = CARTESIAN_POINT ( 'NONE',  ( 72.71365293123227502, -183.6283474603465606, -30.61552143554913030 ) ) ;
#41752 = PLANE ( 'NONE',  #27033 ) ;
#41753 = CIRCLE ( 'NONE', #9830, 125.0000000000000000 ) ;
#41754 = EDGE_CURVE ( 'NONE', #24430, #20725, #26208, .T. ) ;
#41755 = ORIENTED_EDGE ( 'NONE', *, *, #14115, .T. ) ;
#41756 = DIRECTION ( 'NONE',  ( -0.000000000000000000, -0.5680647467311596976, -0.8229838658936536877 ) ) ;
#41757 = CARTESIAN_POINT ( 'NONE',  ( 74.18685885783125400, -193.5000000000000000, -18.13990644964002996 ) ) ;
#41758 = AXIS2_PLACEMENT_3D ( 'NONE', #40673, #16802, #48856 ) ;
#41759 = LINE ( 'NONE', #1551, #39949 ) ;
#41760 = ORIENTED_EDGE ( 'NONE', *, *, #36138, .F. ) ;
#41761 = EDGE_CURVE ( 'NONE', #33090, #45648, #34042, .T. ) ;
#41762 = CARTESIAN_POINT ( 'NONE',  ( -48.53836737940255119, -193.5000000000000000, -0.9982437317643153563 ) ) ;
#41763 = CARTESIAN_POINT ( 'NONE',  ( -305.0000000000000568, -123.5000000000000284, -60.00000000000000000 ) ) ;
#41764 = EDGE_CURVE ( 'NONE', #19780, #9360, #10379, .T. ) ;
#41765 = CARTESIAN_POINT ( 'NONE',  ( 76.09804998693969935, -175.3837268820161057, 10.27263529369908746 ) ) ;
#41766 = ORIENTED_EDGE ( 'NONE', *, *, #24643, .F. ) ;
#41767 = DIRECTION ( 'NONE',  ( -0.000000000000000000, 1.000000000000000000, -0.000000000000000000 ) ) ;
#41768 = ORIENTED_EDGE ( 'NONE', *, *, #24000, .T. ) ;
#41769 = EDGE_CURVE ( 'NONE', #46929, #33918, #37462, .T. ) ;
#41770 = AXIS2_PLACEMENT_3D ( 'NONE', #50019, #17453, #28977 ) ;
#41771 = DIRECTION ( 'NONE',  ( -0.000000000000000000, 1.000000000000000000, -0.000000000000000000 ) ) ;
#41772 = CIRCLE ( 'NONE', #45991, 15.00000000000000000 ) ;
#41773 = LINE ( 'NONE', #45715, #29541 ) ;
#41774 = LINE ( 'NONE', #29155, #3553 ) ;
#41775 = CIRCLE ( 'NONE', #14059, 60.00000000000000000 ) ;
#41776 = CARTESIAN_POINT ( 'NONE',  ( -336.3521761649653854, -117.8908635894569272, -59.73723787327232060 ) ) ;
#41777 = LINE ( 'NONE', #45721, #21856 ) ;
#41778 = ORIENTED_EDGE ( 'NONE', *, *, #1326, .T. ) ;
#41780 = ADVANCED_FACE ( 'NONE', ( #45881 ), #9873, .T. ) ;
#41779 = DIRECTION ( 'NONE',  ( -0.000000000000000000, -1.000000000000000000, -0.000000000000000000 ) ) ;
#41781 = ORIENTED_EDGE ( 'NONE', *, *, #40626, .T. ) ;
#41782 = FACE_OUTER_BOUND ( 'NONE', #29026, .T. ) ;
#41783 = AXIS2_PLACEMENT_3D ( 'NONE', #7768, #51414, #19346 ) ;
#41784 = ORIENTED_EDGE ( 'NONE', *, *, #24380, .F. ) ;
#41785 = DIRECTION ( 'NONE',  ( -0.9842305779475967187, 0.000000000000000000, -0.1768902751225733538 ) ) ;
#41786 = CIRCLE ( 'NONE', #11447, 125.0000000000000000 ) ;
#41787 = ORIENTED_EDGE ( 'NONE', *, *, #31778, .T. ) ;
#41788 = CIRCLE ( 'NONE', #38443, 125.0000000000000000 ) ;
#41789 =( NAMED_UNIT ( * ) PLANE_ANGLE_UNIT ( ) SI_UNIT ( $, .RADIAN. ) );
#41790 = CARTESIAN_POINT ( 'NONE',  ( -339.1964088526558498, -79.66942718702553350, -39.49849221029258928 ) ) ;
#41791 = VERTEX_POINT ( 'NONE', #18284 ) ;
#41794 = EDGE_LOOP ( 'NONE', ( #32457, #20177, #4959, #18852 ) ) ;
#41793 = DIRECTION ( 'NONE',  ( 0.000000000000000000, 0.000000000000000000, 1.000000000000000000 ) ) ;
#41792 = CARTESIAN_POINT ( 'NONE',  ( -2.245234434168357218, 57.57781898212405025, -16.67725351333963602 ) ) ;
#41795 = DIRECTION ( 'NONE',  ( -0.8455960035018234011, 0.000000000000000000, -0.5338233779647948429 ) ) ;
#41796 = VERTEX_POINT ( 'NONE', #42436 ) ;
#41797 = DIRECTION ( 'NONE',  ( 0.000000000000000000, 1.000000000000000000, 0.000000000000000000 ) ) ;
#41798 = VERTEX_POINT ( 'NONE', #18020 ) ;
#41799 = EDGE_CURVE ( 'NONE', #41579, #16540, #34301, .T. ) ;
#41800 = CARTESIAN_POINT ( 'NONE',  ( 46.00000000000000711, 35.00000000000000000, -55.00000000000000000 ) ) ;
#41803 = ORIENTED_EDGE ( 'NONE', *, *, #4725, .F. ) ;
#41802 = CARTESIAN_POINT ( 'NONE',  ( -339.1964088526558498, -71.49045607248255862, -27.86139516340906397 ) ) ;
#41801 = CARTESIAN_POINT ( 'NONE',  ( -77.43961373357963396, -175.3837268820161057, -120.5706864261535145 ) ) ;
#41804 = ORIENTED_EDGE ( 'NONE', *, *, #38929, .F. ) ;
#41805 = CARTESIAN_POINT ( 'NONE',  ( -160.7804753152582293, -175.3837268820161057, -52.57768177182448710 ) ) ;
#41806 = VECTOR ( 'NONE', #25318, 1000.000000000000000 ) ;
#41807 = CARTESIAN_POINT ( 'NONE',  ( -151.1459075827612537, -193.5000000000000000, 69.53890913632950799 ) ) ;
#41808 = AXIS2_PLACEMENT_3D ( 'NONE', #13881, #18351, #1535 ) ;
#41809 = CARTESIAN_POINT ( 'NONE',  ( 76.43863189440992301, -189.7472609257535510, -4.533605064403317009 ) ) ;
#41810 = ORIENTED_EDGE ( 'NONE', *, *, #37059, .T. ) ;
#41811 = CARTESIAN_POINT ( 'NONE',  ( -171.7300019102062549, -193.5000000000000000, -20.83798868929510562 ) ) ;
#41812 = FACE_OUTER_BOUND ( 'NONE', #45286, .T. ) ;
#41813 = CARTESIAN_POINT ( 'NONE',  ( -180.0000000000000568, -130.6726371812771959, 60.00000000000000711 ) ) ;
#41814 = VECTOR ( 'NONE', #6435, 1000.000000000000000 ) ;
#41815 = DIRECTION ( 'NONE',  ( -0.9982437317643222396, 0.000000000000000000, 0.05924062789370006937 ) ) ;
#41816 = ORIENTED_EDGE ( 'NONE', *, *, #27237, .T. ) ;
#41817 = DIRECTION ( 'NONE',  ( -0.000000000000000000, 1.000000000000000000, -0.000000000000000000 ) ) ;
#41818 = LINE ( 'NONE', #17656, #42395 ) ;
#41819 = PLANE ( 'NONE',  #19573 ) ;
#41820 = ORIENTED_EDGE ( 'NONE', *, *, #3739, .F. ) ;
#41821 = CIRCLE ( 'NONE', #48548, 15.24495751795539000 ) ;
#41822 = LINE ( 'NONE', #44996, #50820 ) ;
#41823 = CARTESIAN_POINT ( 'NONE',  ( -144.8751831225492026, -193.5000000000000000, 77.99872144864772849 ) ) ;
#41824 = EDGE_CURVE ( 'NONE', #32234, #2175, #6463, .T. ) ;
#41825 = DIRECTION ( 'NONE',  ( -0.000000000000000000, 1.000000000000000000, -0.000000000000000000 ) ) ;
#41826 = LINE ( 'NONE', #1871, #29989 ) ;
#41827 = ADVANCED_FACE ( 'NONE', ( #17519 ), #38505, .F. ) ;
#41829 = CIRCLE ( 'NONE', #28378, 125.0000000000000000 ) ;
#41828 = DIRECTION ( 'NONE',  ( -8.718379230999705894E-17, 0.7485107481710977506, -0.6631226582407989678 ) ) ;
#41830 = DIRECTION ( 'NONE',  ( 0.000000000000000000, -1.000000000000000000, 0.000000000000000000 ) ) ;
#41831 = FACE_OUTER_BOUND ( 'NONE', #24308, .T. ) ;
#41833 = VERTEX_POINT ( 'NONE', #13549 ) ;
#41832 = DIRECTION ( 'NONE',  ( 0.6965510290630033685, 0.000000000000000000, -0.7175072570443249420 ) ) ;
#41834 = ORIENTED_EDGE ( 'NONE', *, *, #4013, .F. ) ;
#41835 = CARTESIAN_POINT ( 'NONE',  ( -305.0000000000000568, -70.14212160686594189, 27.43969411971487560 ) ) ;
#41836 = CARTESIAN_POINT ( 'NONE',  ( -47.49008656418669005, -189.7472609257535510, 0.1476465640024920423 ) ) ;
#41838 = ORIENTED_EDGE ( 'NONE', *, *, #23168, .F. ) ;
#41837 = CARTESIAN_POINT ( 'NONE',  ( -339.1964088526558498, -138.1050951016792681, -57.16590939599323917 ) ) ;
#41839 = PRODUCT_DEFINITION_FORMATION_WITH_SPECIFIED_SOURCE ( 'ANY', '', #14281, .NOT_KNOWN. ) ;
#41840 = VECTOR ( 'NONE', #20330, 1000.000000000000000 ) ;
#41841 = ORIENTED_EDGE ( 'NONE', *, *, #33724, .T. ) ;
#41842 = VECTOR ( 'NONE', #14703, 1000.000000000000114 ) ;
#41843 = ORIENTED_EDGE ( 'NONE', *, *, #3702, .F. ) ;
#41844 = DIRECTION ( 'NONE',  ( 0.000000000000000000, 0.000000000000000000, -1.000000000000000000 ) ) ;
#41845 = AXIS2_PLACEMENT_3D ( 'NONE', #20500, #521, #36021 ) ;
#41846 = DIRECTION ( 'NONE',  ( -0.000000000000000000, 1.000000000000000000, -0.000000000000000000 ) ) ;
#41847 = DIRECTION ( 'NONE',  ( 0.000000000000000000, -1.000000000000000000, 0.000000000000000000 ) ) ;
#41848 = VERTEX_POINT ( 'NONE', #51380 ) ;
#41849 = CARTESIAN_POINT ( 'NONE',  ( 46.00000000000000711, 33.00000000000000000, -46.00000000000000000 ) ) ;
#41850 = AXIS2_PLACEMENT_3D ( 'NONE', #13589, #30141, #49604 ) ;
#41852 = ORIENTED_EDGE ( 'NONE', *, *, #7959, .T. ) ;
#41851 = DIRECTION ( 'NONE',  ( -0.000000000000000000, 0.000000000000000000, -1.000000000000000000 ) ) ;
#41853 = CARTESIAN_POINT ( 'NONE',  ( -114.4014177456970600, -177.1207230881787780, 105.0256126866236315 ) ) ;
#41854 = ORIENTED_EDGE ( 'NONE', *, *, #30859, .F. ) ;
#41855 = LINE ( 'NONE', #32913, #25523 ) ;
#41856 = ORIENTED_EDGE ( 'NONE', *, *, #2309, .F. ) ;
#41857 = EDGE_CURVE ( 'NONE', #9868, #27228, #30877, .T. ) ;
#41858 = LINE ( 'NONE', #17168, #19907 ) ;
#41859 = DIRECTION ( 'NONE',  ( 0.000000000000000000, 1.000000000000000000, 0.000000000000000000 ) ) ;
#41860 = CARTESIAN_POINT ( 'NONE',  ( 60.00000000000000000, -93.50000000000001421, -51.54700538379269403 ) ) ;
#41861 = AXIS2_PLACEMENT_3D ( 'NONE', #25134, #24344, #44574 ) ;
#41862 = ORIENTED_EDGE ( 'NONE', *, *, #26227, .T. ) ;
#41863 = EDGE_LOOP ( 'NONE', ( #47804, #15808, #35371, #17641 ) ) ;
#41864 = CARTESIAN_POINT ( 'NONE',  ( 70.98542830588607444, -177.1207230881787780, -36.78613984829961936 ) ) ;
#41865 = DIRECTION ( 'NONE',  ( 0.000000000000000000, -0.000000000000000000, -1.000000000000000000 ) ) ;
#41866 = ORIENTED_EDGE ( 'NONE', *, *, #22474, .F. ) ;
#41867 = DIRECTION ( 'NONE',  ( -0.000000000000000000, 1.000000000000000000, -0.000000000000000000 ) ) ;
#41868 = ADVANCED_FACE ( 'NONE', ( #22990 ), #7735, .F. ) ;
#41869 = ORIENTED_EDGE ( 'NONE', *, *, #50762, .F. ) ;
#41870 = LINE ( 'NONE', #33199, #9968 ) ;
#41871 = PLANE ( 'NONE',  #18057 ) ;
#41872 = EDGE_LOOP ( 'NONE', ( #25668, #3421, #44784, #46750 ) ) ;
#41873 = CARTESIAN_POINT ( 'NONE',  ( -330.4913330509368166, -74.65991953890832633, 33.10432812419081472 ) ) ;
#41874 = ORIENTED_EDGE ( 'NONE', *, *, #21838, .F. ) ;
#41875 = FACE_OUTER_BOUND ( 'NONE', #22424, .T. ) ;
#41876 = AXIS2_PLACEMENT_3D ( 'NONE', #13910, #29406, #2065 ) ;
#41877 = CARTESIAN_POINT ( 'NONE',  ( -339.1964088526558498, -96.52406086224443982, -52.47426709956138069 ) ) ;
#41878 = DIRECTION ( 'NONE',  ( -0.000000000000000000, 0.7485107481711089639, 0.6631226582407863113 ) ) ;
#41879 = EDGE_CURVE ( 'NONE', #46318, #34791, #11676, .T. ) ;
#41880 = VERTEX_POINT ( 'NONE', #11404 ) ;
#41881 = AXIS2_PLACEMENT_3D ( 'NONE', #22838, #38857, #17868 ) ;
#41882 = CARTESIAN_POINT ( 'NONE',  ( -169.0136227435421006, -175.3837268820161057, -33.11246405730811659 ) ) ;
#41883 = CARTESIAN_POINT ( 'NONE',  ( -330.4913330509368166, -130.1153096980145563, 58.63009191191294178 ) ) ;
#41884 = CARTESIAN_POINT ( 'NONE',  ( -336.3521761649654422, -133.2247606357419443, -58.25253621232173629 ) ) ;
#41885 = CARTESIAN_POINT ( 'NONE',  ( -336.3521761649654422, -123.5000000000000284, 0.000000000000000000 ) ) ;
#41886 = ORIENTED_EDGE ( 'NONE', *, *, #30437, .T. ) ;
#41887 = DIRECTION ( 'NONE',  ( 0.000000000000000000, -0.2393156642875615969, -0.9709418174260511236 ) ) ;
#41888 = EDGE_LOOP ( 'NONE', ( #30941, #50040, #48299, #42977 ) ) ;
#41889 = CIRCLE ( 'NONE', #48620, 60.00000000000000000 ) ;
#41890 = CARTESIAN_POINT ( 'NONE',  ( 64.72501964220592185, -193.5000000000000000, 53.00774697410174952 ) ) ;
#41892 = ORIENTED_EDGE ( 'NONE', *, *, #15954, .T. ) ;
#41891 = CYLINDRICAL_SURFACE ( 'NONE', #14449, 125.0000000000000000 ) ;
#41893 = ORIENTED_EDGE ( 'NONE', *, *, #14164, .T. ) ;
#41894 = AXIS2_PLACEMENT_3D ( 'NONE', #35578, #15631, #31645 ) ;
#41895 = DIRECTION ( 'NONE',  ( 0.000000000000000000, 0.000000000000000000, 1.000000000000000000 ) ) ;
#41896 = VERTEX_POINT ( 'NONE', #3283 ) ;
#41897 = CARTESIAN_POINT ( 'NONE',  ( -48.47912675150885065, -189.7472609257535510, 6.938893903907228378E-15 ) ) ;
#41898 = ORIENTED_EDGE ( 'NONE', *, *, #49004, .T. ) ;
#41899 = CARTESIAN_POINT ( 'NONE',  ( -48.47912675150885065, -177.1207230881787780, 6.938893903907228378E-15 ) ) ;
#41900 = DIRECTION ( 'NONE',  ( 1.000000000000000000, 0.000000000000000000, -0.000000000000000000 ) ) ;
#41901 = ADVANCED_FACE ( 'NONE', ( #23763 ), #35327, .F. ) ;
#41902 = LINE ( 'NONE', #9589, #36990 ) ;
#41903 = CARTESIAN_POINT ( 'NONE',  ( -180.0000000000000568, -123.5000000000000284, 6.938893903907228378E-15 ) ) ;
#41904 = ORIENTED_EDGE ( 'NONE', *, *, #1886, .F. ) ;
#41905 = ORIENTED_EDGE ( 'NONE', *, *, #14612, .F. ) ;
#41906 = VERTEX_POINT ( 'NONE', #39769 ) ;
#41907 = EDGE_CURVE ( 'NONE', #9601, #21200, #35076, .T. ) ;
#41908 = LINE ( 'NONE', #49290, #1410 ) ;
#41909 = CARTESIAN_POINT ( 'NONE',  ( 15.80042947435468470, -193.5000000000000000, 107.2060569716377927 ) ) ;
#41910 = CIRCLE ( 'NONE', #52020, 125.0000000000000000 ) ;
#41911 = CARTESIAN_POINT ( 'NONE',  ( -152.8713435144644848, -183.6283474603465606, -68.75510947788595217 ) ) ;
#41912 = CARTESIAN_POINT ( 'NONE',  ( -170.0000000000000284, -123.5000000000000284, -41.63467731922663972 ) ) ;
#41913 = ORIENTED_EDGE ( 'NONE', *, *, #33062, .F. ) ;
#41914 = CIRCLE ( 'NONE', #16730, 125.0000000000000000 ) ;
#41915 = ADVANCED_FACE ( 'NONE', ( #15628 ), #31902, .F. ) ;
#41916 = EDGE_CURVE ( 'NONE', #20898, #38913, #11921, .T. ) ;
#41917 = ORIENTED_EDGE ( 'NONE', *, *, #14619, .T. ) ;
#41919 = ORIENTED_EDGE ( 'NONE', *, *, #42936, .T. ) ;
#41918 = DIRECTION ( 'NONE',  ( 0.000000000000000000, -1.000000000000000000, -0.000000000000000000 ) ) ;
#41920 = ORIENTED_EDGE ( 'NONE', *, *, #29877, .F. ) ;
#41921 = ADVANCED_FACE ( 'NONE', ( #27955 ), #7221, .F. ) ;
#41922 = PLANE ( 'NONE',  #49353 ) ;
#41923 = DIRECTION ( 'NONE',  ( -0.000000000000000000, -1.000000000000000000, -0.000000000000000000 ) ) ;
#41924 = DIRECTION ( 'NONE',  ( -1.000000000000000000, -0.000000000000000000, -0.000000000000000000 ) ) ;
#41925 = DIRECTION ( 'NONE',  ( 0.000000000000000000, 0.8660254037844354880, -0.5000000000000054401 ) ) ;
#41926 = VERTEX_POINT ( 'NONE', #22732 ) ;
#41927 = CARTESIAN_POINT ( 'NONE',  ( -30.00000000000000000, 0.000000000000000000, -30.00000000000000711 ) ) ;
#41928 = VERTEX_POINT ( 'NONE', #3528 ) ;
#41929 = VECTOR ( 'NONE', #24911, 1000.000000000000000 ) ;
#41930 = ORIENTED_EDGE ( 'NONE', *, *, #10895, .T. ) ;
#41931 = DIRECTION ( 'NONE',  ( 0.000000000000000000, 1.000000000000000000, 0.000000000000000000 ) ) ;
#41932 = CARTESIAN_POINT ( 'NONE',  ( -339.1964088526558498, -71.49045607248213230, 27.86139516340826106 ) ) ;
#41933 = EDGE_CURVE ( 'NONE', #47240, #48128, #38742, .T. ) ;
#41934 = VERTEX_POINT ( 'NONE', #23262 ) ;
#41935 = LINE ( 'NONE', #21452, #50005 ) ;
#41936 = PLANE ( 'NONE',  #10405 ) ;
#41937 = PLANE ( 'NONE',  #29594 ) ;
#41938 = DIRECTION ( 'NONE',  ( -0.000000000000000000, 1.000000000000000000, -0.000000000000000000 ) ) ;
#41939 = LINE ( 'NONE', #50361, #122 ) ;
#41940 = CARTESIAN_POINT ( 'NONE',  ( -46.00000000000000711, 20.00000000000000000, 46.00000000000000000 ) ) ;
#41941 = ORIENTED_EDGE ( 'NONE', *, *, #10714, .T. ) ;
#41942 = AXIS2_PLACEMENT_3D ( 'NONE', #48362, #40205, #13138 ) ;
#41943 = CYLINDRICAL_SURFACE ( 'NONE', #27278, 125.0000000000000000 ) ;
#41944 = EDGE_LOOP ( 'NONE', ( #12052, #35488, #41760, #43038 ) ) ;
#41945 = VERTEX_POINT ( 'NONE', #31644 ) ;
#41946 = LINE ( 'NONE', #49849, #16219 ) ;
#41947 = ORIENTED_EDGE ( 'NONE', *, *, #40559, .F. ) ;
#41948 = PRODUCT ( 'Center Pivot Base Stud', 'Center Pivot Base Stud', '', ( #17333 ) ) ;
#41949 = DIRECTION ( 'NONE',  ( 0.000000000000000000, -6.036837696399288689E-14, 1.000000000000000000 ) ) ;
#41950 = DIRECTION ( 'NONE',  ( -0.9473263538541923934, 0.000000000000000000, 0.3202698538628350744 ) ) ;
#41952 = EDGE_LOOP ( 'NONE', ( #47983, #22667, #28845, #25777 ) ) ;
#41951 = LINE ( 'NONE', #41699, #36335 ) ;
#41953 = ADVANCED_FACE ( 'NONE', ( #39000 ), #42952, .T. ) ;
#41954 = EDGE_CURVE ( 'NONE', #41304, #29838, #31128, .T. ) ;
#41955 = DIRECTION ( 'NONE',  ( -0.000000000000000000, 1.000000000000000000, -0.000000000000000000 ) ) ;
#41956 = CARTESIAN_POINT ( 'NONE',  ( 57.31108707223382481, -175.3837268820161057, -66.58401203837755133 ) ) ;
#41957 = EDGE_LOOP ( 'NONE', ( #16721, #38543, #11896, #47769 ) ) ;
#41958 = ORIENTED_EDGE ( 'NONE', *, *, #15998, .F. ) ;
#41959 = AXIS2_PLACEMENT_3D ( 'NONE', #29816, #19034, #42691 ) ;
#41960 = ORIENTED_EDGE ( 'NONE', *, *, #49052, .F. ) ;
#41961 = FACE_OUTER_BOUND ( 'NONE', #10685, .T. ) ;
#41962 = CARTESIAN_POINT ( 'NONE',  ( -96.65280530915693191, -193.5000000000000000, -115.3442529744087466 ) ) ;
#41963 = CARTESIAN_POINT ( 'NONE',  ( 0.000000000000000000, -172.0560480877259408, -33.51582005713793677 ) ) ;
#41964 = LINE ( 'NONE', #5979, #15273 ) ;
#41965 = CARTESIAN_POINT ( 'NONE',  ( -160.0000000000000284, -123.5000000000000284, -41.63467731922663972 ) ) ;
#41966 = VERTEX_POINT ( 'NONE', #27443 ) ;
#41967 = EDGE_CURVE ( 'NONE', #17878, #12249, #27699, .T. ) ;
#41968 = ADVANCED_FACE ( 'NONE', ( #51136 ), #15121, .T. ) ;
#41969 = LINE ( 'NONE', #2024, #39979 ) ;
#41970 = ORIENTED_EDGE ( 'NONE', *, *, #26559, .T. ) ;
#41972 = EDGE_LOOP ( 'NONE', ( #855, #38784, #24114, #21024 ) ) ;
#41971 = DIRECTION ( 'NONE',  ( 0.000000000000000000, 0.000000000000000000, 1.000000000000000000 ) ) ;
#41973 = VERTEX_POINT ( 'NONE', #43485 ) ;
#41974 = ADVANCED_FACE ( 'NONE', ( #39276 ), #7489, .F. ) ;
#41975 = CIRCLE ( 'NONE', #23526, 125.0000000000000000 ) ;
#41976 = ORIENTED_EDGE ( 'NONE', *, *, #29495, .F. ) ;
#41977 = CARTESIAN_POINT ( 'NONE',  ( -173.2419626162308646, -193.5000000000000000, 7.696413904698416353 ) ) ;
#41978 = CARTESIAN_POINT ( 'NONE',  ( 74.80070215680143519, -193.5000000000000000, 13.35228579481200306 ) ) ;
#41979 = ORIENTED_EDGE ( 'NONE', *, *, #38805, .T. ) ;
#41980 = EDGE_CURVE ( 'NONE', #30123, #49231, #20868, .T. ) ;
#41981 = LINE ( 'NONE', #9940, #18758 ) ;
#41982 = DIRECTION ( 'NONE',  ( 0.000000000000000000, 0.000000000000000000, -1.000000000000000000 ) ) ;
#41983 = ORIENTED_EDGE ( 'NONE', *, *, #41368, .F. ) ;
#41984 = PLANE ( 'NONE',  #12411 ) ;
#41985 = EDGE_LOOP ( 'NONE', ( #22645, #25802, #45859, #29429 ) ) ;
#41986 = ORIENTED_EDGE ( 'NONE', *, *, #38466, .T. ) ;
#41987 = CARTESIAN_POINT ( 'NONE',  ( 68.24201764719070695, -177.1207230881787780, -44.73448837594909833 ) ) ;
#41988 = CARTESIAN_POINT ( 'NONE',  ( 67.04262753014327814, -193.5000000000000000, -47.74645837849745078 ) ) ;
#41989 = LINE ( 'NONE', #9953, #24474 ) ;
#41990 = DIRECTION ( 'NONE',  ( -0.9929810960135169173, 0.000000000000000000, -0.1182731709213660498 ) ) ;
#41991 = VERTEX_POINT ( 'NONE', #24799 ) ;
#41992 = CARTESIAN_POINT ( 'NONE',  ( 22.73247662810270597, -193.5000000000000000, -101.5140743725395254 ) ) ;
#41993 = DIRECTION ( 'NONE',  ( 0.9027978299657416494, 0.000000000000000000, 0.4300652022765245608 ) ) ;
#41994 = DIRECTION ( 'NONE',  ( -1.000000000000000000, 0.000000000000000000, 0.000000000000000000 ) ) ;
#41995 = DIRECTION ( 'NONE',  ( -0.000000000000000000, -0.9709418174260534551, -0.2393156642875516327 ) ) ;
#41996 = EDGE_LOOP ( 'NONE', ( #12273, #39813, #17469, #39499 ) ) ;
#41997 = DIRECTION ( 'NONE',  ( -0.000000000000000000, 1.000000000000000000, 0.000000000000000000 ) ) ;
#41998 = DIRECTION ( 'NONE',  ( 1.000000000000000000, 0.000000000000000000, 0.000000000000000000 ) ) ;
#41999 = AXIS2_PLACEMENT_3D ( 'NONE', #3971, #19992, #15812 ) ;
#42000 = AXIS2_PLACEMENT_3D ( 'NONE', #19271, #27904, #47375 ) ;
#42001 = CARTESIAN_POINT ( 'NONE',  ( -305.0000000000000568, -83.33976666098978114, 44.57752413667957825 ) ) ;
#42002 = EDGE_LOOP ( 'NONE', ( #51569, #29489, #48492, #8599 ) ) ;
#42003 = ORIENTED_EDGE ( 'NONE', *, *, #40655, .F. ) ;
#42004 = CARTESIAN_POINT ( 'NONE',  ( -48.47912675150885065, -189.7472609257535510, 6.938893903907228378E-15 ) ) ;
#42005 = LINE ( 'NONE', #41763, #24410 ) ;
#42006 = CARTESIAN_POINT ( 'NONE',  ( 75.43907105790114542, -189.7472609257535510, -4.503971736580769658 ) ) ;
#42007 = VERTEX_POINT ( 'NONE', #353 ) ;
#42008 = DIRECTION ( 'NONE',  ( 0.000000000000000000, 1.000000000000000000, -0.000000000000000000 ) ) ;
#42009 = ORIENTED_EDGE ( 'NONE', *, *, #29211, .F. ) ;
#42010 = ADVANCED_FACE ( 'NONE', ( #28212 ), #36893, .T. ) ;
#42011 = DIRECTION ( 'NONE',  ( 1.000000000000000000, -0.000000000000000000, -0.000000000000000000 ) ) ;
#42012 = VECTOR ( 'NONE', #6999, 1000.000000000000000 ) ;
#42013 = LINE ( 'NONE', #6027, #37948 ) ;
#42014 = LINE ( 'NONE', #6028, #34647 ) ;
#42015 = EDGE_CURVE ( 'NONE', #30281, #7649, #8499, .T. ) ;
#42016 = EDGE_CURVE ( 'NONE', #2925, #37502, #32159, .T. ) ;
#42017 = ADVANCED_FACE ( 'NONE', ( #40288 ), #48203, .T. ) ;
#42018 = DIRECTION ( 'NONE',  ( -0.000000000000000000, 0.000000000000000000, 1.000000000000000000 ) ) ;
#42019 = EDGE_CURVE ( 'NONE', #49683, #39625, #16403, .T. ) ;
#42020 = DIRECTION ( 'NONE',  ( 0.8757349421956310831, 0.000000000000000000, 0.4827922027307550712 ) ) ;
#42021 = ORIENTED_EDGE ( 'NONE', *, *, #41916, .T. ) ;
#42022 = EDGE_CURVE ( 'NONE', #45184, #9630, #4842, .T. ) ;
#42023 = FACE_OUTER_BOUND ( 'NONE', #13083, .T. ) ;
#42024 = ORIENTED_EDGE ( 'NONE', *, *, #22980, .F. ) ;
#42025 = CARTESIAN_POINT ( 'NONE',  ( -305.0000000000000568, -115.7716958700749643, 59.50019592636132160 ) ) ;
#42026 = ORIENTED_EDGE ( 'NONE', *, *, #23151, .T. ) ;
#42027 = EDGE_CURVE ( 'NONE', #41587, #12564, #2730, .T. ) ;
#42028 = DIRECTION ( 'NONE',  ( 0.000000000000000000, 0.000000000000000000, 1.000000000000000000 ) ) ;
#42029 = VECTOR ( 'NONE', #50491, 1000.000000000000114 ) ;
#42030 = EDGE_CURVE ( 'NONE', #6199, #44148, #8248, .T. ) ;
#42031 = EDGE_CURVE ( 'NONE', #30689, #24824, #5267, .T. ) ;
#42032 = CIRCLE ( 'NONE', #23581, 125.0000000000000000 ) ;
#42033 = DIRECTION ( 'NONE',  ( 0.000000000000000000, -0.000000000000000000, -1.000000000000000000 ) ) ;
#42034 = CARTESIAN_POINT ( 'NONE',  ( -332.3517673607765914, -174.5186198893880771, 29.74944317415823392 ) ) ;
#42035 = VERTEX_POINT ( 'NONE', #36625 ) ;
#42038 = ORIENTED_EDGE ( 'NONE', *, *, #28113, .T. ) ;
#42037 = DIRECTION ( 'NONE',  ( -8.718379230999707126E-17, 0.5680647467311510379, -0.8229838658936596829 ) ) ;
#42036 = CARTESIAN_POINT ( 'NONE',  ( -3.878716889882891650, 56.06915626585696089, -17.38004533314371969 ) ) ;
#42039 = EDGE_CURVE ( 'NONE', #33788, #10029, #16920, .T. ) ;
#42040 = DIRECTION ( 'NONE',  ( 0.000000000000000000, -1.000000000000000000, 0.000000000000000000 ) ) ;
#42041 = VERTEX_POINT ( 'NONE', #45049 ) ;
#42042 = PLANE ( 'NONE',  #11289 ) ;
#42043 = ORIENTED_EDGE ( 'NONE', *, *, #19191, .F. ) ;
#42044 = ADVANCED_FACE ( 'NONE', ( #32419 ), #48722, .F. ) ;
#42045 = CARTESIAN_POINT ( 'NONE',  ( -48.07600332222087758, -177.1207230881787780, -0.9151456172430111335 ) ) ;
#42048 = EDGE_LOOP ( 'NONE', ( #28392, #13605, #30927, #50830 ) ) ;
#42047 = DIRECTION ( 'NONE',  ( 0.000000000000000000, 0.000000000000000000, 1.000000000000000000 ) ) ;
#42046 = LINE ( 'NONE', #33125, #38368 ) ;
#42049 = EDGE_LOOP ( 'NONE', ( #26182, #6932, #46524, #9338 ) ) ;
#42050 = EDGE_CURVE ( 'NONE', #27166, #32896, #45553, .T. ) ;
#42051 = FACE_OUTER_BOUND ( 'NONE', #747, .T. ) ;
#42052 = ORIENTED_EDGE ( 'NONE', *, *, #49706, .F. ) ;
#42053 = DIRECTION ( 'NONE',  ( 0.000000000000000000, 1.000000000000000000, -0.000000000000000000 ) ) ;
#42055 = CIRCLE ( 'NONE', #8469, 60.00000000000000000 ) ;
#42054 = FACE_OUTER_BOUND ( 'NONE', #10502, .T. ) ;
#42056 = ORIENTED_EDGE ( 'NONE', *, *, #11312, .T. ) ;
#42057 = FACE_OUTER_BOUND ( 'NONE', #11590, .T. ) ;
#42058 = DIRECTION ( 'NONE',  ( 0.000000000000000000, 0.000000000000000000, 1.000000000000000000 ) ) ;
#42059 = CARTESIAN_POINT ( 'NONE',  ( -330.4913330509368166, -123.5000000000000284, 0.000000000000000000 ) ) ;
#42060 = CARTESIAN_POINT ( 'NONE',  ( -330.4913330509368166, -182.1300919119128423, 6.615309698015510165 ) ) ;
#42061 = DIRECTION ( 'NONE',  ( 0.000000000000000000, -0.8229838658936556861, 0.5680647467311569221 ) ) ;
#42062 = ORIENTED_EDGE ( 'NONE', *, *, #3115, .T. ) ;
#42063 = FACE_OUTER_BOUND ( 'NONE', #49785, .T. ) ;
#42064 = EDGE_CURVE ( 'NONE', #35839, #44743, #17179, .T. ) ;
#42065 = LINE ( 'NONE', #38635, #34882 ) ;
#42066 = ADVANCED_FACE ( 'NONE', ( #36361 ), #13240, .T. ) ;
#42067 = DIRECTION ( 'NONE',  ( 0.000000000000000000, 0.000000000000000000, 1.000000000000000000 ) ) ;
#42068 = ORIENTED_EDGE ( 'NONE', *, *, #11521, .T. ) ;
#42069 = CARTESIAN_POINT ( 'NONE',  ( -172.1767935149754294, -183.6283474603465606, 8.665274887906315726 ) ) ;
#42070 = DIRECTION ( 'NONE',  ( -0.000000000000000000, 1.000000000000000000, -0.000000000000000000 ) ) ;
#42071 = AXIS2_PLACEMENT_3D ( 'NONE', #36121, #15912, #15137 ) ;
#42072 = CARTESIAN_POINT ( 'NONE',  ( -48.47912675150885065, -189.7472609257535510, 6.938893903907228378E-15 ) ) ;
#42073 = DIRECTION ( 'NONE',  ( 1.000000000000000000, -0.000000000000000000, 0.000000000000000000 ) ) ;
#42074 = VECTOR ( 'NONE', #43169, 1000.000000000000000 ) ;
#42075 = CARTESIAN_POINT ( 'NONE',  ( 53.62339707355158680, -177.1207230881787780, -70.36529243996334060 ) ) ;
#42076 = CARTESIAN_POINT ( 'NONE',  ( -171.2727421180348415, -183.6283474603465606, 23.38221600314377113 ) ) ;
#42077 = FACE_OUTER_BOUND ( 'NONE', #35610, .T. ) ;
#42078 = CARTESIAN_POINT ( 'NONE',  ( 66.36634345758743336, -193.5000000000000000, 46.76022031560705017 ) ) ;
#42079 = VERTEX_POINT ( 'NONE', #8760 ) ;
#42080 = ADVANCED_FACE ( 'NONE', ( #7987 ), #16145, .T. ) ;
#42081 = EDGE_CURVE ( 'NONE', #19338, #32588, #50227, .T. ) ;
#42082 = CARTESIAN_POINT ( 'NONE',  ( 68.24201764719070695, -183.6283474603465606, -44.73448837594909833 ) ) ;
#42083 = CIRCLE ( 'NONE', #3478, 125.0000000000000000 ) ;
#42084 = ADVANCED_FACE ( 'NONE', ( #14219 ), #46528, .T. ) ;
#42085 = EDGE_CURVE ( 'NONE', #34424, #51547, #17166, .T. ) ;
#42086 = DIRECTION ( 'NONE',  ( 0.000000000000000000, 0.000000000000000000, -1.000000000000000000 ) ) ;
#42088 = ORIENTED_EDGE ( 'NONE', *, *, #16677, .T. ) ;
#42087 = FACE_OUTER_BOUND ( 'NONE', #17360, .T. ) ;
#42089 = ORIENTED_EDGE ( 'NONE', *, *, #17988, .T. ) ;
#42090 = CIRCLE ( 'NONE', #13546, 60.00000000000000000 ) ;
#42091 = ORIENTED_EDGE ( 'NONE', *, *, #49994, .F. ) ;
#42092 = LINE ( 'NONE', #51042, #10785 ) ;
#42093 = DIRECTION ( 'NONE',  ( -0.000000000000000000, -0.9709418174260502354, 0.2393156642875652051 ) ) ;
#42094 = CARTESIAN_POINT ( 'NONE',  ( 74.49773146996547268, -177.1207230881787780, -22.39848972532282190 ) ) ;
#42095 = ORIENTED_EDGE ( 'NONE', *, *, #7025, .F. ) ;
#42096 = CARTESIAN_POINT ( 'NONE',  ( -305.0000000000000568, -172.5932850007656043, 34.49419324804693332 ) ) ;
#42097 = DIRECTION ( 'NONE',  ( -0.5085311186492094127, 0.000000000000000000, -0.8610436117673619938 ) ) ;
#42099 = EDGE_LOOP ( 'NONE', ( #21844, #23042, #20025, #40057 ) ) ;
#42098 = LINE ( 'NONE', #18200, #5679 ) ;
#42100 = DIRECTION ( 'NONE',  ( 0.000000000000000000, 0.000000000000000000, 1.000000000000000000 ) ) ;
#42101 = EDGE_LOOP ( 'NONE', ( #36220, #25472, #28320, #17201 ) ) ;
#42102 = DIRECTION ( 'NONE',  ( -0.000000000000000000, 1.000000000000000000, -0.000000000000000000 ) ) ;
#42103 = AXIS2_PLACEMENT_3D ( 'NONE', #16607, #28136, #11853 ) ;
#42104 = ORIENTED_EDGE ( 'NONE', *, *, #33748, .F. ) ;
#42105 = CARTESIAN_POINT ( 'NONE',  ( 6.443011874827240248, -183.6283474603465606, 112.2878385610370771 ) ) ;
#42106 = LINE ( 'NONE', #26338, #31345 ) ;
#42107 = VECTOR ( 'NONE', #35857, 1000.000000000000114 ) ;
#42108 = CARTESIAN_POINT ( 'NONE',  ( -336.3521761649654422, -64.50000000000000000, -1.632288850093980725 ) ) ;
#42109 = EDGE_CURVE ( 'NONE', #48626, #10132, #26800, .T. ) ;
#42110 = VECTOR ( 'NONE', #13708, 1000.000000000000000 ) ;
#42111 = EDGE_LOOP ( 'NONE', ( #24854, #48398, #49066, #19820 ) ) ;
#42112 = CARTESIAN_POINT ( 'NONE',  ( -172.6359455740846442, -177.1207230881787780, -14.49428645563791562 ) ) ;
#42113 = CARTESIAN_POINT ( 'NONE',  ( 26.70958190211001337, -189.7472609257535510, -99.85818990449013199 ) ) ;
#42114 = ORIENTED_EDGE ( 'NONE', *, *, #21504, .F. ) ;
#42115 = CARTESIAN_POINT ( 'NONE',  ( -170.0000000000000284, -93.50000000000001421, -51.54700538379269403 ) ) ;
#42116 = VERTEX_POINT ( 'NONE', #10019 ) ;
#42117 = FACE_BOUND ( 'NONE', #28743, .T. ) ;
#42118 = CIRCLE ( 'NONE', #47166, 125.0000000000000000 ) ;
#42119 = CARTESIAN_POINT ( 'NONE',  ( -336.3521761649654422, -153.2494431741581025, -51.01861988938816950 ) ) ;
#42120 = ORIENTED_EDGE ( 'NONE', *, *, #36557, .F. ) ;
#42121 = DIRECTION ( 'NONE',  ( 0.7575112421616145841, 0.000000000000000000, 0.6528221181905280446 ) ) ;
#42122 = ORIENTED_EDGE ( 'NONE', *, *, #8262, .T. ) ;
#42123 = VECTOR ( 'NONE', #46308, 1000.000000000000114 ) ;
#42124 = VECTOR ( 'NONE', #35234, 1000.000000000000000 ) ;
#42125 = CARTESIAN_POINT ( 'NONE',  ( -43.48323084606168720, -183.6283474603465606, 123.9001241957026167 ) ) ;
#42126 = CARTESIAN_POINT ( 'NONE',  ( -118.9967449635792462, -175.3837268820161057, -103.2098131075562009 ) ) ;
#42127 = ORIENTED_EDGE ( 'NONE', *, *, #21305, .F. ) ;
#42128 = CARTESIAN_POINT ( 'NONE',  ( -169.9131040279660567, -177.1207230881787780, 29.64437826672837417 ) ) ;
#42129 = DIRECTION ( 'NONE',  ( -0.9890401873221644768, 0.000000000000000000, 0.1476465640024779702 ) ) ;
#42130 = DIRECTION ( 'NONE',  ( -0.000000000000000000, 1.000000000000000000, -0.000000000000000000 ) ) ;
#42131 = ORIENTED_EDGE ( 'NONE', *, *, #9575, .T. ) ;
#42132 = CARTESIAN_POINT ( 'NONE',  ( -330.4913330509368166, -180.9052250602809693, -13.63415328425256945 ) ) ;
#42133 = ORIENTED_EDGE ( 'NONE', *, *, #33005, .T. ) ;
#42134 = DIRECTION ( 'NONE',  ( -0.000000000000000000, 0.000000000000000000, 1.000000000000000000 ) ) ;
#42135 = DIRECTION ( 'NONE',  ( 0.000000000000000000, -0.8660254037844354880, -0.5000000000000054401 ) ) ;
#42137 = ORIENTED_EDGE ( 'NONE', *, *, #44486, .F. ) ;
#42136 = CARTESIAN_POINT ( 'NONE',  ( 76.01188277843579044, -193.5000000000000000, 11.26891947860284482 ) ) ;
#42138 = AXIS2_PLACEMENT_3D ( 'NONE', #12714, #4584, #29001 ) ;
#42139 = VERTEX_POINT ( 'NONE', #15242 ) ;
#42140 = EDGE_CURVE ( 'NONE', #34344, #12665, #30238, .T. ) ;
#42141 = DIRECTION ( 'NONE',  ( -0.000000000000000000, 1.000000000000000000, -0.000000000000000000 ) ) ;
#42142 = AXIS2_PLACEMENT_3D ( 'NONE', #41491, #44421, #24968 ) ;
#42143 = DIRECTION ( 'NONE',  ( -0.000000000000000000, 1.000000000000000000, -0.000000000000000000 ) ) ;
#42144 = ORIENTED_EDGE ( 'NONE', *, *, #10318, .T. ) ;
#42145 = CARTESIAN_POINT ( 'NONE',  ( 0.000000000000000000, -167.6621341420946578, 39.12423683620730230 ) ) ;
#42146 = ORIENTED_EDGE ( 'NONE', *, *, #39104, .F. ) ;
#42147 = DIRECTION ( 'NONE',  ( 0.000000000000000000, 0.000000000000000000, -1.000000000000000000 ) ) ;
#42148 = CARTESIAN_POINT ( 'NONE',  ( -332.3517673607765914, -72.01665693856799066, -28.86398714850468039 ) ) ;
#42149 = CARTESIAN_POINT ( 'NONE',  ( 69.88207517204676833, -175.3837268820161057, 40.19484891390057868 ) ) ;
#42150 = LINE ( 'NONE', #18765, #10651 ) ;
#42151 = ORIENTED_EDGE ( 'NONE', *, *, #31598, .T. ) ;
#42152 = AXIS2_PLACEMENT_3D ( 'NONE', #11820, #8932, #3956 ) ;
#42153 = EDGE_LOOP ( 'NONE', ( #51199, #31940, #14733, #4962 ) ) ;
#42154 = AXIS2_PLACEMENT_3D ( 'NONE', #22209, #14333, #34544 ) ;
#42155 = ORIENTED_EDGE ( 'NONE', *, *, #28624, .T. ) ;
#42156 = DIRECTION ( 'NONE',  ( 0.000000000000000000, 0.000000000000000000, 1.000000000000000000 ) ) ;
#42157 = LINE ( 'NONE', #10627, #2543 ) ;
#42158 = AXIS2_PLACEMENT_3D ( 'NONE', #31202, #31974, #11996 ) ;
#42159 = AXIS2_PLACEMENT_3D ( 'NONE', #24268, #20310, #15878 ) ;
#42160 = EDGE_CURVE ( 'NONE', #38437, #12857, #14474, .T. ) ;
#42161 = PLANE ( 'NONE',  #3557 ) ;
#42162 = LINE ( 'NONE', #6446, #28038 ) ;
#42163 = ORIENTED_EDGE ( 'NONE', *, *, #1352, .T. ) ;
#42164 = DIRECTION ( 'NONE',  ( -0.8124868780056783146, 0.000000000000000000, -0.5829794791144762289 ) ) ;
#42165 = VERTEX_POINT ( 'NONE', #31004 ) ;
#42167 = VERTEX_POINT ( 'NONE', #38105 ) ;
#42166 = CARTESIAN_POINT ( 'NONE',  ( -332.3517673607765914, -123.5000000000000284, 0.000000000000000000 ) ) ;
#42168 = CARTESIAN_POINT ( 'NONE',  ( -121.8391548840036620, -177.1207230881787780, -99.97252634603250954 ) ) ;
#42169 = CARTESIAN_POINT ( 'NONE',  ( -63.96873441216509093, -189.7472609257535510, -123.0287672223651612 ) ) ;
#42170 = VECTOR ( 'NONE', #3655, 1000.000000000000000 ) ;
#42171 = DIRECTION ( 'NONE',  ( 0.000000000000000000, 1.000000000000000000, 0.000000000000000000 ) ) ;
#42172 = CARTESIAN_POINT ( 'NONE',  ( -330.4913330509368166, -123.5000000000000284, 0.000000000000000000 ) ) ;
#42173 = VERTEX_POINT ( 'NONE', #2386 ) ;
#42175 = EDGE_CURVE ( 'NONE', #32017, #32388, #10507, .T. ) ;
#42174 = CARTESIAN_POINT ( 'NONE',  ( -98.62206515315352817, -189.7472609257535510, 113.4093733337831225 ) ) ;
#42176 = ORIENTED_EDGE ( 'NONE', *, *, #42019, .F. ) ;
#42177 = AXIS2_PLACEMENT_3D ( 'NONE', #6613, #42852, #42334 ) ;
#42178 = ORIENTED_EDGE ( 'NONE', *, *, #37819, .F. ) ;
#42179 = CARTESIAN_POINT ( 'NONE',  ( 70.68712318874649725, -183.6283474603465606, -37.74128873232327663 ) ) ;
#42180 = ADVANCED_FACE ( 'NONE', ( #38628 ), #27049, .F. ) ;
#42181 = DIRECTION ( 'NONE',  ( 0.000000000000000000, -1.000000000000000000, 0.000000000000000000 ) ) ;
#42182 = ORIENTED_EDGE ( 'NONE', *, *, #23134, .T. ) ;
#42183 = CARTESIAN_POINT ( 'NONE',  ( 18.49541618049843095, -177.1207230881787780, 105.5434062319798159 ) ) ;
#42184 = DIRECTION ( 'NONE',  ( -0.000000000000000000, 1.000000000000000000, -0.000000000000000000 ) ) ;
#42185 = DIRECTION ( 'NONE',  ( -0.6528221181905174975, 0.000000000000000000, -0.7575112421616236880 ) ) ;
#42186 = CARTESIAN_POINT ( 'NONE',  ( -127.6327502296859535, -183.6283474603465606, -95.45105364470086329 ) ) ;
#42187 = CIRCLE ( 'NONE', #3592, 125.0000000000000000 ) ;
#42188 = ADVANCED_FACE ( 'NONE', ( #42057 ), #43089, .T. ) ;
#42189 = CARTESIAN_POINT ( 'NONE',  ( -339.1964088526558498, -175.5095439275173135, 27.86139516340941213 ) ) ;
#42190 = ORIENTED_EDGE ( 'NONE', *, *, #4709, .F. ) ;
#42191 = AXIS2_PLACEMENT_3D ( 'NONE', #27465, #35347, #43232 ) ;
#42192 = AXIS2_PLACEMENT_3D ( 'NONE', #30308, #1688, #30057 ) ;
#42193 = FACE_OUTER_BOUND ( 'NONE', #30237, .T. ) ;
#42194 = EDGE_LOOP ( 'NONE', ( #38109, #35204, #30833, #50148 ) ) ;
#42195 = VERTEX_POINT ( 'NONE', #38885 ) ;
#42196 = DIRECTION ( 'NONE',  ( -1.000000000000000000, 0.000000000000000000, 0.000000000000000000 ) ) ;
#42197 = ADVANCED_FACE ( 'NONE', ( #50999 ), #7098, .T. ) ;
#42198 = AXIS2_PLACEMENT_3D ( 'NONE', #6801, #14428, #22823 ) ;
#42199 = ORIENTED_EDGE ( 'NONE', *, *, #40353, .F. ) ;
#42200 = ADVANCED_FACE ( 'NONE', ( #6069 ), #2887, .T. ) ;
#42201 = CARTESIAN_POINT ( 'NONE',  ( -60.00000000000000000, 20.00000000000000000, 60.00000000000000711 ) ) ;
#42202 = EDGE_CURVE ( 'NONE', #26145, #20663, #46029, .T. ) ;
#42203 = CARTESIAN_POINT ( 'NONE',  ( -336.3521761649654422, -119.0014323656137947, -58.88711093124865670 ) ) ;
#42204 = DIRECTION ( 'NONE',  ( -0.7378332790417333475, 0.000000000000000000, 0.6749830015182038956 ) ) ;
#42205 = ORIENTED_EDGE ( 'NONE', *, *, #31542, .F. ) ;
#42206 = LINE ( 'NONE', #46178, #31676 ) ;
#42207 = VECTOR ( 'NONE', #7548, 1000.000000000000000 ) ;
#42208 = CARTESIAN_POINT ( 'NONE',  ( 75.52097166332622180, -183.6283474603465606, -0.3215015308240974368 ) ) ;
#42209 = PLANE ( 'NONE',  #34899 ) ;
#42210 = EDGE_LOOP ( 'NONE', ( #28723, #15911, #34307, #35354 ) ) ;
#42211 = EDGE_LOOP ( 'NONE', ( #48246, #49076, #24032, #34178 ) ) ;
#42212 = CIRCLE ( 'NONE', #38013, 125.0000000000000000 ) ;
#42213 = ORIENTED_EDGE ( 'NONE', *, *, #262, .F. ) ;
#42214 = DIRECTION ( 'NONE',  ( -0.000000000000000000, 0.1205366802553199113, -0.9927088740980544168 ) ) ;
#42215 = DIRECTION ( 'NONE',  ( 0.000000000000000000, 0.000000000000000000, -1.000000000000000000 ) ) ;
#42216 = EDGE_CURVE ( 'NONE', #26081, #12481, #26279, .T. ) ;
#42217 = LINE ( 'NONE', #35898, #43564 ) ;
#42218 = CARTESIAN_POINT ( 'NONE',  ( 41.00573479224730988, -183.6283474603465606, -87.27805883780176543 ) ) ;
#42219 = CARTESIAN_POINT ( 'NONE',  ( -339.1964088526558498, -131.1080185721133660, -58.50955523165751515 ) ) ;
#42220 = ORIENTED_EDGE ( 'NONE', *, *, #7324, .T. ) ;
#42221 = AXIS2_PLACEMENT_3D ( 'NONE', #44133, #8139, #20221 ) ;
#42222 = VECTOR ( 'NONE', #3043, 1000.000000000000000 ) ;
#42223 = DIRECTION ( 'NONE',  ( 0.000000000000000000, -1.000000000000000000, 0.000000000000000000 ) ) ;
#42224 = ORIENTED_EDGE ( 'NONE', *, *, #10581, .F. ) ;
#42226 = ORIENTED_EDGE ( 'NONE', *, *, #22093, .T. ) ;
#42225 = CARTESIAN_POINT ( 'NONE',  ( 60.00000000000001421, -93.50000000000002842, 51.54700538379266561 ) ) ;
#42227 = AXIS2_PLACEMENT_3D ( 'NONE', #23714, #20031, #43944 ) ;
#42228 = ORIENTED_EDGE ( 'NONE', *, *, #42085, .T. ) ;
#42229 = LINE ( 'NONE', #8691, #27462 ) ;
#42230 = EDGE_LOOP ( 'NONE', ( #21246, #2465, #50926, #34225 ) ) ;
#42231 = CARTESIAN_POINT ( 'NONE',  ( -81.14588623932564815, -183.6283474603465606, 120.6560517527617833 ) ) ;
#42232 = EDGE_LOOP ( 'NONE', ( #37137, #26147, #17100, #30794 ) ) ;
#42233 = DIRECTION ( 'NONE',  ( -0.000000000000000000, -0.000000000000000000, 1.000000000000000000 ) ) ;
#42234 = VECTOR ( 'NONE', #18043, 1000.000000000000114 ) ;
#42235 = EDGE_LOOP ( 'NONE', ( #30723, #32380, #14852, #25705, #22553, #29834, #6290, #766 ) ) ;
#42236 = CARTESIAN_POINT ( 'NONE',  ( -18.31235070009513421, -193.5000000000000000, 121.3052580173829966 ) ) ;
#42237 = ORIENTED_EDGE ( 'NONE', *, *, #35945, .F. ) ;
#42238 = ORIENTED_EDGE ( 'NONE', *, *, #48371, .F. ) ;
#42239 = CARTESIAN_POINT ( 'NONE',  ( -73.94077438226447896, -193.5000000000000000, 122.3793467049372481 ) ) ;
#42240 = LINE ( 'NONE', #22280, #49081 ) ;
#42241 = CARTESIAN_POINT ( 'NONE',  ( -130.2106798473772642, -193.5000000000000000, 94.57776286494217288 ) ) ;
#42242 = DIRECTION ( 'NONE',  ( 0.000000000000000000, 1.000000000000000000, 0.000000000000000000 ) ) ;
#42243 = VERTEX_POINT ( 'NONE', #50732 ) ;
#42244 = FACE_OUTER_BOUND ( 'NONE', #48672, .T. ) ;
#42245 = VECTOR ( 'NONE', #11411, 1000.000000000000000 ) ;
#42246 = DIRECTION ( 'NONE',  ( -0.5085311186492273983, 0.000000000000000000, 0.8610436117673514467 ) ) ;
#42247 = EDGE_CURVE ( 'NONE', #19688, #39351, #6323, .T. ) ;
#42248 = EDGE_CURVE ( 'NONE', #8523, #22453, #23128, .T. ) ;
#42249 = ITEM_DEFINED_TRANSFORMATION ( 'NONE', 'NONE', #33483,  #31742 ) ;
#42250 = CARTESIAN_POINT ( 'NONE',  ( 14.43219681437621205, -193.5000000000000000, 106.8558168688117860 ) ) ;
#42251 = LINE ( 'NONE', #18361, #2734 ) ;
#42252 = ORIENTED_EDGE ( 'NONE', *, *, #31391, .T. ) ;
#42253 = FACE_OUTER_BOUND ( 'NONE', #29781, .T. ) ;
#42254 = FACE_OUTER_BOUND ( 'NONE', #46976, .T. ) ;
#42255 = CIRCLE ( 'NONE', #24623, 125.0000000000000000 ) ;
#42256 = CARTESIAN_POINT ( 'NONE',  ( -332.3517673607765914, -163.8460225846223466, -43.07972642080364523 ) ) ;
#42257 = ORIENTED_EDGE ( 'NONE', *, *, #7568, .F. ) ;
#42258 = DIRECTION ( 'NONE',  ( -0.000000000000000000, 1.000000000000000000, -0.000000000000000000 ) ) ;
#42259 = CARTESIAN_POINT ( 'NONE',  ( -180.0000000000000568, -123.5000000000000284, 0.000000000000000000 ) ) ;
#42260 = VERTEX_POINT ( 'NONE', #22347 ) ;
#42261 = DIRECTION ( 'NONE',  ( 0.000000000000000000, 0.000000000000000000, -1.000000000000000000 ) ) ;
#42262 = EDGE_CURVE ( 'NONE', #21231, #17420, #32283, .T. ) ;
#42263 = VECTOR ( 'NONE', #10833, 1000.000000000000227 ) ;
#42264 = ORIENTED_EDGE ( 'NONE', *, *, #16533, .F. ) ;
#42265 = ADVANCED_FACE ( 'NONE', ( #28348 ), #39393, .F. ) ;
#42266 = DIRECTION ( 'NONE',  ( 0.000000000000000000, 0.7485107481711000821, -0.6631226582407965253 ) ) ;
#42267 = VECTOR ( 'NONE', #10960, 1000.000000000000000 ) ;
#42268 = EDGE_CURVE ( 'NONE', #15701, #875, #48335, .T. ) ;
#42269 = FACE_OUTER_BOUND ( 'NONE', #37447, .T. ) ;
#42270 = LINE ( 'NONE', #22304, #22920 ) ;
#42271 = EDGE_CURVE ( 'NONE', #29853, #3, #47825, .T. ) ;
#42272 = DIRECTION ( 'NONE',  ( -0.000000000000000000, 1.000000000000000000, -0.000000000000000000 ) ) ;
#42273 = DIRECTION ( 'NONE',  ( -1.000000000000000000, 0.000000000000000000, 0.000000000000000000 ) ) ;
#42274 = ORIENTED_EDGE ( 'NONE', *, *, #10464, .F. ) ;
#42275 = FACE_OUTER_BOUND ( 'NONE', #1332, .T. ) ;
#42276 = ORIENTED_EDGE ( 'NONE', *, *, #14402, .F. ) ;
#42277 = DIRECTION ( 'NONE',  ( 0.9960498426152165630, 0.000000000000000000, 0.08879589532293852283 ) ) ;
#42278 = ORIENTED_EDGE ( 'NONE', *, *, #14260, .F. ) ;
#42279 = CARTESIAN_POINT ( 'NONE',  ( 12.99855592850622443, -193.5000000000000000, 108.8370090194294875 ) ) ;
#42280 = VECTOR ( 'NONE', #50943, 1000.000000000000114 ) ;
#42281 = AXIS2_PLACEMENT_3D ( 'NONE', #33278, #20942, #33009 ) ;
#42282 = CARTESIAN_POINT ( 'NONE',  ( -49.44376233341720450, -189.7472609257535510, -0.2635871660690713436 ) ) ;
#42283 = CARTESIAN_POINT ( 'NONE',  ( -48.47912675150885065, -175.3837268820161057, 6.938893903907228378E-15 ) ) ;
#42284 = VERTEX_POINT ( 'NONE', #7366 ) ;
#42287 = ORIENTED_EDGE ( 'NONE', *, *, #7454, .T. ) ;
#42286 = DIRECTION ( 'NONE',  ( -0.000000000000000000, 1.000000000000000000, -0.000000000000000000 ) ) ;
#42285 = PLANE ( 'NONE',  #16630 ) ;
#42288 = DIRECTION ( 'NONE',  ( -0.000000000000000000, -0.5680647467311510379, 0.8229838658936596829 ) ) ;
#42289 = EDGE_LOOP ( 'NONE', ( #30620, #13606, #44977, #45893 ) ) ;
#42290 = CARTESIAN_POINT ( 'NONE',  ( -48.41988612361514299, -175.3837268820161057, -0.9982437317643144681 ) ) ;
#42291 = ORIENTED_EDGE ( 'NONE', *, *, #20144, .F. ) ;
#42292 = CARTESIAN_POINT ( 'NONE',  ( 2.449293598294706513E-15, -63.50000000000000000, 20.00000000000000000 ) ) ;
#42295 = EDGE_LOOP ( 'NONE', ( #31212, #22675, #32966, #36535 ) ) ;
#42294 = PLANE ( 'NONE',  #43454 ) ;
#42293 = DIRECTION ( 'NONE',  ( -0.000000000000000000, 1.000000000000000000, -0.000000000000000000 ) ) ;
#42296 = VECTOR ( 'NONE', #49359, 999.9999999999998863 ) ;
#42297 = ORIENTED_EDGE ( 'NONE', *, *, #2754, .T. ) ;
#42298 = CARTESIAN_POINT ( 'NONE',  ( -48.47912675150885065, -175.3837268820161057, 6.938893903907228378E-15 ) ) ;
#42299 = ORIENTED_EDGE ( 'NONE', *, *, #17605, .F. ) ;
#42300 = CARTESIAN_POINT ( 'NONE',  ( -305.0000000000000568, -173.1613497474965300, 33.67120938215357739 ) ) ;
#42301 = DIRECTION ( 'NONE',  ( -8.718379230999707126E-17, -1.000000000000000000, 1.047444401652940007E-14 ) ) ;
#42302 = ORIENTED_EDGE ( 'NONE', *, *, #16231, .F. ) ;
#42303 = EDGE_CURVE ( 'NONE', #51141, #11736, #23388, .T. ) ;
#42304 = DIRECTION ( 'NONE',  ( -0.000000000000000000, 1.000000000000000000, -0.000000000000000000 ) ) ;
#42305 = FACE_OUTER_BOUND ( 'NONE', #23429, .T. ) ;
#42306 = DIRECTION ( 'NONE',  ( -0.000000000000000000, 1.000000000000000000, -0.000000000000000000 ) ) ;
#42307 = CYLINDRICAL_SURFACE ( 'NONE', #21754, 125.0000000000000000 ) ;
#42308 = FACE_OUTER_BOUND ( 'NONE', #42486, .T. ) ;
#42309 = EDGE_CURVE ( 'NONE', #16252, #30647, #3658, .T. ) ;
#42310 = EDGE_CURVE ( 'NONE', #10147, #14417, #1169, .T. ) ;
#42311 = ORIENTED_EDGE ( 'NONE', *, *, #2511, .T. ) ;
#42312 = EDGE_CURVE ( 'NONE', #18236, #27224, #44400, .T. ) ;
#42313 =( NAMED_UNIT ( * ) PLANE_ANGLE_UNIT ( ) SI_UNIT ( $, .RADIAN. ) );
#42314 = CARTESIAN_POINT ( 'NONE',  ( -114.1105527140175155, -183.6283474603465606, 106.3838142112217611 ) ) ;
#42315 = LINE ( 'NONE', #23138, #28120 ) ;
#42316 = EDGE_CURVE ( 'NONE', #21288, #18537, #5397, .T. ) ;
#42317 = DIRECTION ( 'NONE',  ( 0.8838680338115290080, 0.000000000000000000, -0.4677363560876381943 ) ) ;
#42318 = VERTEX_POINT ( 'NONE', #40426 ) ;
#42319 = DIRECTION ( 'NONE',  ( -0.000000000000000000, 1.000000000000000000, -0.000000000000000000 ) ) ;
#42320 = ADVANCED_FACE ( 'NONE', ( #31254 ), #12048, .F. ) ;
#42321 = DIRECTION ( 'NONE',  ( 0.8858462335218260097, 0.000000000000000000, -0.4639789333096864810 ) ) ;
#42322 = EDGE_CURVE ( 'NONE', #25437, #47778, #35450, .T. ) ;
#42323 = AXIS2_PLACEMENT_3D ( 'NONE', #29064, #40623, #17263 ) ;
#42324 = VECTOR ( 'NONE', #38306, 1000.000000000000000 ) ;
#42325 = DIRECTION ( 'NONE',  ( -0.000000000000000000, 1.000000000000000000, 0.000000000000000000 ) ) ;
#42326 = CARTESIAN_POINT ( 'NONE',  ( -332.3517673607765914, -183.4777928329299357, 1.632288850093980725 ) ) ;
#42327 = VERTEX_POINT ( 'NONE', #51768 ) ;
#42328 = ADVANCED_FACE ( 'NONE', ( #27821 ), #23886, .F. ) ;
#42329 = AXIS2_PLACEMENT_3D ( 'NONE', #51391, #39532, #43497 ) ;
#42330 = EDGE_CURVE ( 'NONE', #42476, #47980, #16023, .T. ) ;
#42331 = FACE_OUTER_BOUND ( 'NONE', #39514, .T. ) ;
#42332 = EDGE_CURVE ( 'NONE', #24982, #23338, #24169, .T. ) ;
#42333 = CARTESIAN_POINT ( 'NONE',  ( -336.3521761649654422, -183.4422309845877805, 2.632288850093980503 ) ) ;
#42334 = DIRECTION ( 'NONE',  ( 0.000000000000000000, -0.000000000000000000, -1.000000000000000000 ) ) ;
#42335 = CARTESIAN_POINT ( 'NONE',  ( -305.0000000000000568, -64.66963335249506883, 11.78931550685348206 ) ) ;
#42336 = ADVANCED_FACE ( 'NONE', ( #227 ), #16270, .T. ) ;
#42337 = ORIENTED_EDGE ( 'NONE', *, *, #39008, .T. ) ;
#42338 = AXIS2_PLACEMENT_3D ( 'NONE', #35066, #38218, #38491 ) ;
#42339 = CARTESIAN_POINT ( 'NONE',  ( -163.4524646452520926, -175.3837268820161057, 46.44493303993096589 ) ) ;
#42340 = EDGE_CURVE ( 'NONE', #39776, #32877, #43973, .T. ) ;
#42341 = CARTESIAN_POINT ( 'NONE',  ( -48.47912675150885065, -183.6283474603465606, 6.938893903907228378E-15 ) ) ;
#42343 = ORIENTED_EDGE ( 'NONE', *, *, #44786, .F. ) ;
#42342 = DIRECTION ( 'NONE',  ( -6.978251959525016136E-17, 0.000000000000000000, 1.000000000000000000 ) ) ;
#42344 = VERTEX_POINT ( 'NONE', #20463 ) ;
#42345 = ORIENTED_EDGE ( 'NONE', *, *, #21600, .T. ) ;
#42346 = LINE ( 'NONE', #51283, #35122 ) ;
#42347 = DIRECTION ( 'NONE',  ( -0.000000000000000000, 1.000000000000000000, -0.000000000000000000 ) ) ;
#42348 = CARTESIAN_POINT ( 'NONE',  ( -55.05561436132770581, -175.3837268820161057, 124.8268793598474105 ) ) ;
#42349 = VERTEX_POINT ( 'NONE', #43358 ) ;
#42350 = EDGE_CURVE ( 'NONE', #12857, #4717, #27579, .T. ) ;
#42351 = DIRECTION ( 'NONE',  ( 0.000000000000000000, -1.000000000000000000, -0.000000000000000000 ) ) ;
#42352 = CARTESIAN_POINT ( 'NONE',  ( 70.02079272397770637, -177.1207230881787780, -36.52255268223056106 ) ) ;
#42355 = VERTEX_POINT ( 'NONE', #33073 ) ;
#42354 = CARTESIAN_POINT ( 'NONE',  ( -336.3521761649654422, -153.2494431741581025, -51.01861988938816950 ) ) ;
#42353 = CARTESIAN_POINT ( 'NONE',  ( -47.92047998570519951, -189.7472609257535510, -0.8294056854501942189 ) ) ;
#42356 = DIRECTION ( 'NONE',  ( -1.000000000000000000, -1.043714542225393381E-14, 3.644109847259164491E-29 ) ) ;
#42357 = VECTOR ( 'NONE', #14980, 1000.000000000000114 ) ;
#42358 = EDGE_LOOP ( 'NONE', ( #18766, #36134, #39406, #25782 ) ) ;
#42359 = LINE ( 'NONE', #11070, #46542 ) ;
#42360 = ORIENTED_EDGE ( 'NONE', *, *, #48777, .T. ) ;
#42361 = AXIS2_PLACEMENT_3D ( 'NONE', #24672, #17589, #17070 ) ;
#42362 = DIRECTION ( 'NONE',  ( 0.9027978299657416494, 0.000000000000000000, 0.4300652022765245608 ) ) ;
#42363 = DIRECTION ( 'NONE',  ( 0.000000000000000000, 0.000000000000000000, 1.000000000000000000 ) ) ;
#42364 = CARTESIAN_POINT ( 'NONE',  ( -48.30223647638628393, -175.3837268820161057, 0.9842305779476049343 ) ) ;
#42365 = AXIS2_PLACEMENT_3D ( 'NONE', #3611, #51459, #6796 ) ;
#42366 = EDGE_CURVE ( 'NONE', #44602, #50728, #20997, .T. ) ;
#42367 = VERTEX_POINT ( 'NONE', #45694 ) ;
#42368 = DIRECTION ( 'NONE',  ( -0.000000000000000000, 1.000000000000000000, -0.000000000000000000 ) ) ;
#42369 = LINE ( 'NONE', #6389, #30059 ) ;
#42370 = ORIENTED_EDGE ( 'NONE', *, *, #39759, .F. ) ;
#42371 = AXIS2_PLACEMENT_3D ( 'NONE', #28840, #465, #209 ) ;
#42372 = DIRECTION ( 'NONE',  ( -0.000000000000000000, 0.9709418174260553425, 0.2393156642875449158 ) ) ;
#42373 = CIRCLE ( 'NONE', #9671, 4.999999999999997335 ) ;
#42374 = CARTESIAN_POINT ( 'NONE',  ( -25.55153130240594450, -189.7472609257535510, 122.8793122007210599 ) ) ;
#42375 = ADVANCED_FACE ( 'NONE', ( #9176 ), #41211, .F. ) ;
#42376 = EDGE_CURVE ( 'NONE', #33013, #46176, #5763, .T. ) ;
#42377 = VERTEX_POINT ( 'NONE', #21256 ) ;
#42378 = EDGE_CURVE ( 'NONE', #36303, #49241, #37789, .T. ) ;
#42379 = FACE_BOUND ( 'NONE', #30629, .T. ) ;
#42380 = AXIS2_PLACEMENT_3D ( 'NONE', #21357, #36874, #1386 ) ;
#42381 = DIRECTION ( 'NONE',  ( -8.718379230999708359E-17, -0.4647231720437573488, 0.8854560256532157947 ) ) ;
#42382 = EDGE_CURVE ( 'NONE', #1918, #38465, #1013, .T. ) ;
#42383 = ORIENTED_EDGE ( 'NONE', *, *, #6154, .T. ) ;
#42384 = CARTESIAN_POINT ( 'NONE',  ( -330.4913330509368166, -156.6043281241909995, 48.84008046109159551 ) ) ;
#42385 = EDGE_LOOP ( 'NONE', ( #24290, #48964, #16745, #21258 ) ) ;
#42386 = CARTESIAN_POINT ( 'NONE',  ( -140.5933766095837427, -189.7472609257535510, -84.49831343337066869 ) ) ;
#42387 = CARTESIAN_POINT ( 'NONE',  ( -121.0298553105864130, -183.6283474603465606, -100.5610240384919223 ) ) ;
#42388 = EDGE_LOOP ( 'NONE', ( #16968, #49919, #1783, #23502 ) ) ;
#42389 = DIRECTION ( 'NONE',  ( -0.000000000000000000, -1.000000000000000000, 0.000000000000000000 ) ) ;
#42390 = DIRECTION ( 'NONE',  ( -0.000000000000000000, -1.000000000000000000, 0.000000000000000000 ) ) ;
#42391 = DIRECTION ( 'NONE',  ( -0.000000000000000000, 1.000000000000000000, -0.000000000000000000 ) ) ;
#42392 = ORIENTED_EDGE ( 'NONE', *, *, #42813, .T. ) ;
#42393 = DIRECTION ( 'NONE',  ( -0.000000000000000000, 0.3546048870425331789, -0.9350162426854158326 ) ) ;
#42394 = ORIENTED_EDGE ( 'NONE', *, *, #45012, .T. ) ;
#42395 = VECTOR ( 'NONE', #8977, 1000.000000000000000 ) ;
#42396 = ADVANCED_FACE ( 'NONE', ( #40680 ), #40956, .T. ) ;
#42397 = LINE ( 'NONE', #15084, #18559 ) ;
#42398 = CARTESIAN_POINT ( 'NONE',  ( -332.3517673607765914, -123.5000000000000284, 0.000000000000000000 ) ) ;
#42400 = ORIENTED_EDGE ( 'NONE', *, *, #6734, .F. ) ;
#42399 = CARTESIAN_POINT ( 'NONE',  ( -87.28630321566649286, -177.1207230881787780, 118.8234112238818341 ) ) ;
#42401 = VECTOR ( 'NONE', #2871, 1000.000000000000114 ) ;
#42402 = VECTOR ( 'NONE', #50029, 1000.000000000000000 ) ;
#42403 = EDGE_CURVE ( 'NONE', #20203, #10838, #17584, .T. ) ;
#42404 = ORIENTED_EDGE ( 'NONE', *, *, #4867, .T. ) ;
#42405 = CARTESIAN_POINT ( 'NONE',  ( -164.6073096293132494, -183.6283474603465606, 43.47841891815207305 ) ) ;
#42406 = CIRCLE ( 'NONE', #48300, 125.0000000000000000 ) ;
#42407 = EDGE_CURVE ( 'NONE', #44579, #47358, #2857, .T. ) ;
#42408 = FACE_OUTER_BOUND ( 'NONE', #38861, .T. ) ;
#42409 = EDGE_LOOP ( 'NONE', ( #50132, #29618, #10811, #5924 ) ) ;
#42410 = CARTESIAN_POINT ( 'NONE',  ( -280.0000000000000000, -63.50000000000000000, -60.00000000000000711 ) ) ;
#42411 = AXIS2_PLACEMENT_3D ( 'NONE', #29567, #13013, #13543 ) ;
#42412 = ORIENTED_EDGE ( 'NONE', *, *, #29821, .T. ) ;
#42413 = DIRECTION ( 'NONE',  ( -0.000000000000000000, 1.000000000000000000, -0.000000000000000000 ) ) ;
#42414 = LINE ( 'NONE', #46372, #26688 ) ;
#42415 = CIRCLE ( 'NONE', #50833, 60.00000000000000000 ) ;
#42417 = VECTOR ( 'NONE', #43842, 1000.000000000000000 ) ;
#42416 = LINE ( 'NONE', #35300, #7650 ) ;
#42418 = LINE ( 'NONE', #2484, #36644 ) ;
#42419 = ORIENTED_EDGE ( 'NONE', *, *, #38587, .F. ) ;
#42420 = EDGE_LOOP ( 'NONE', ( #3681, #14039, #1889, #22992 ) ) ;
#42421 = ORIENTED_EDGE ( 'NONE', *, *, #42268, .T. ) ;
#42422 = CIRCLE ( 'NONE', #49152, 125.0000000000000000 ) ;
#42423 = DIRECTION ( 'NONE',  ( 1.000000000000000000, -0.000000000000000000, -0.000000000000000000 ) ) ;
#42424 = CARTESIAN_POINT ( 'NONE',  ( -48.47912675150885065, -193.5000000000000000, 6.938893903907228378E-15 ) ) ;
#42425 = CARTESIAN_POINT ( 'NONE',  ( 62.86098202833237281, -193.5000000000000000, 56.81883646197908178 ) ) ;
#42426 = CARTESIAN_POINT ( 'NONE',  ( -48.47912675150885065, -175.3837268820161057, 6.938893903907228378E-15 ) ) ;
#42427 = ORIENTED_EDGE ( 'NONE', *, *, #472, .F. ) ;
#42428 = CYLINDRICAL_SURFACE ( 'NONE', #25689, 125.0000000000000000 ) ;
#42429 = ORIENTED_EDGE ( 'NONE', *, *, #26005, .T. ) ;
#42430 = ORIENTED_EDGE ( 'NONE', *, *, #24709, .F. ) ;
#42431 = AXIS2_PLACEMENT_3D ( 'NONE', #51262, #15249, #50235 ) ;
#42432 = DIRECTION ( 'NONE',  ( -0.000000000000000000, 1.000000000000000000, -0.000000000000000000 ) ) ;
#42433 = CARTESIAN_POINT ( 'NONE',  ( -48.47912675150885065, -183.6283474603465606, 6.938893903907228378E-15 ) ) ;
#42434 = VECTOR ( 'NONE', #24013, 1000.000000000000227 ) ;
#42435 = AXIS2_PLACEMENT_3D ( 'NONE', #26811, #42842, #46540 ) ;
#42436 = CARTESIAN_POINT ( 'NONE',  ( 75.46126020185812422, -189.7472609257535510, 3.844569333773204534 ) ) ;
#42437 = EDGE_CURVE ( 'NONE', #51204, #18822, #9587, .T. ) ;
#42439 = EDGE_CURVE ( 'NONE', #40265, #47080, #12838, .T. ) ;
#42438 = CARTESIAN_POINT ( 'NONE',  ( -365.0160704661291788, -113.5000000000000000, -40.00000000000001421 ) ) ;
#42440 = ORIENTED_EDGE ( 'NONE', *, *, #6428, .T. ) ;
#42441 = DIRECTION ( 'NONE',  ( 0.000000000000000000, 0.000000000000000000, 1.000000000000000000 ) ) ;
#42442 = ORIENTED_EDGE ( 'NONE', *, *, #13814, .F. ) ;
#42443 = DIRECTION ( 'NONE',  ( -0.05924062789370748011, 0.000000000000000000, -0.9982437317643217956 ) ) ;
#42444 = AXIS2_PLACEMENT_3D ( 'NONE', #41265, #13170, #29187 ) ;
#42445 = CARTESIAN_POINT ( 'NONE',  ( -48.30901192927175458, -175.3837268820161057, -124.9998842437354227 ) ) ;
#42446 = EDGE_LOOP ( 'NONE', ( #47004, #40923, #23818, #17756 ) ) ;
#42447 = VECTOR ( 'NONE', #10746, 1000.000000000000000 ) ;
#42448 = DIRECTION ( 'NONE',  ( 0.000000000000000000, 0.000000000000000000, 1.000000000000000000 ) ) ;
#42449 = CARTESIAN_POINT ( 'NONE',  ( -8.169009709621407822, -193.5000000000000000, 118.3219948448695504 ) ) ;
#42450 = DIRECTION ( 'NONE',  ( 0.000000000000000000, 0.000000000000000000, 1.000000000000000000 ) ) ;
#42451 = AXIS2_PLACEMENT_3D ( 'NONE', #51556, #3217, #31573 ) ;
#42452 = CARTESIAN_POINT ( 'NONE',  ( -336.3521761649654422, -66.60506506233235768, -15.70448169564047092 ) ) ;
#42454 = AXIS2_PLACEMENT_3D ( 'NONE', #3294, #39533, #30610 ) ;
#42453 = CARTESIAN_POINT ( 'NONE',  ( -47.78257572244586271, -193.5000000000000000, 0.7175072570443418174 ) ) ;
#42455 = VERTEX_POINT ( 'NONE', #36768 ) ;
#42456 = EDGE_CURVE ( 'NONE', #18178, #20840, #13787, .T. ) ;
#42457 = DIRECTION ( 'NONE',  ( 0.000000000000000000, 0.000000000000000000, 1.000000000000000000 ) ) ;
#42458 = ORIENTED_EDGE ( 'NONE', *, *, #27566, .F. ) ;
#42459 = VERTEX_POINT ( 'NONE', #9429 ) ;
#42460 = CARTESIAN_POINT ( 'NONE',  ( -339.1964088526558498, -180.6659093959934523, -14.60509510167853264 ) ) ;
#42461 = VERTEX_POINT ( 'NONE', #37277 ) ;
#42462 = EDGE_CURVE ( 'NONE', #14296, #26111, #23012, .T. ) ;
#42463 = PLANE ( 'NONE',  #36052 ) ;
#42464 = VECTOR ( 'NONE', #16816, 1000.000000000000000 ) ;
#42465 = VECTOR ( 'NONE', #7297, 1000.000000000000000 ) ;
#42466 = ORIENTED_EDGE ( 'NONE', *, *, #2798, .F. ) ;
#42467 = DIRECTION ( 'NONE',  ( -0.000000000000000000, -1.000000000000000000, 0.000000000000000000 ) ) ;
#42468 = LINE ( 'NONE', #11184, #44751 ) ;
#42469 = EDGE_LOOP ( 'NONE', ( #26979, #51114, #25887, #45155 ) ) ;
#42470 = DIRECTION ( 'NONE',  ( 0.000000000000000000, -1.000000000000000000, 0.000000000000000000 ) ) ;
#42471 = AXIS2_PLACEMENT_3D ( 'NONE', #35448, #31510, #11550 ) ;
#42472 = CIRCLE ( 'NONE', #27349, 125.0000000000000000 ) ;
#42473 = PLANE ( 'NONE',  #1731 ) ;
#42474 = CARTESIAN_POINT ( 'NONE',  ( -336.3521761649654422, -75.87119766449505676, -34.85916744524372746 ) ) ;
#42475 = EDGE_LOOP ( 'NONE', ( #26769, #36065, #9845, #24497 ) ) ;
#42476 = VERTEX_POINT ( 'NONE', #25710 ) ;
#42477 = VERTEX_POINT ( 'NONE', #41745 ) ;
#42478 = CARTESIAN_POINT ( 'NONE',  ( -330.4913330509368166, -144.8891964568517778, 54.98865587491845730 ) ) ;
#42479 = LINE ( 'NONE', #14636, #31037 ) ;
#42480 = VECTOR ( 'NONE', #41364, 1000.000000000000114 ) ;
#42481 = LINE ( 'NONE', #26187, #38539 ) ;
#42482 = CIRCLE ( 'NONE', #19821, 9.999999999999994671 ) ;
#42484 = STYLED_ITEM ( 'NONE', ( #1542 ), #18958 ) ;
#42483 = DIRECTION ( 'NONE',  ( 1.000000000000000000, -0.000000000000000000, -0.000000000000000000 ) ) ;
#42485 = FACE_OUTER_BOUND ( 'NONE', #36211, .T. ) ;
#42486 = EDGE_LOOP ( 'NONE', ( #16538, #11571, #47274, #13676 ) ) ;
#42487 = VECTOR ( 'NONE', #21313, 1000.000000000000000 ) ;
#42488 = EDGE_CURVE ( 'NONE', #21174, #41262, #32559, .T. ) ;
#42489 = AXIS2_PLACEMENT_3D ( 'NONE', #8180, #20790, #283 ) ;
#42490 = DIRECTION ( 'NONE',  ( -0.1182731709213730997, 0.000000000000000000, 0.9929810960135161402 ) ) ;
#42491 = ORIENTED_EDGE ( 'NONE', *, *, #3175, .T. ) ;
#42493 = ORIENTED_EDGE ( 'NONE', *, *, #14961, .T. ) ;
#42492 = FACE_OUTER_BOUND ( 'NONE', #21963, .T. ) ;
#42494 = ORIENTED_EDGE ( 'NONE', *, *, #42027, .F. ) ;
#42495 = PLANE ( 'NONE',  #36699 ) ;
#42496 = VERTEX_POINT ( 'NONE', #28602 ) ;
#42497 = FACE_OUTER_BOUND ( 'NONE', #8194, .T. ) ;
#42498 = DIRECTION ( 'NONE',  ( 0.000000000000000000, -1.000000000000000000, 0.000000000000000000 ) ) ;
#42499 = ADVANCED_FACE ( 'NONE', ( #32815 ), #37544, .T. ) ;
#42500 = DIRECTION ( 'NONE',  ( 0.4566292373937077542, 0.000000000000000000, 0.8896570909947499883 ) ) ;
#42501 = VERTEX_POINT ( 'NONE', #48865 ) ;
#42502 = CARTESIAN_POINT ( 'NONE',  ( -48.47912675150885065, -175.3837268820161057, 6.938893903907228378E-15 ) ) ;
#42503 = EDGE_LOOP ( 'NONE', ( #46951, #38796, #44216, #37006 ) ) ;
#42504 = ORIENTED_EDGE ( 'NONE', *, *, #26685, .T. ) ;
#42505 = DIRECTION ( 'NONE',  ( -0.000000000000000000, 0.5680647467311569221, 0.8229838658936556861 ) ) ;
#42506 = ADVANCED_FACE ( 'NONE', ( #1541 ), #44911, .T. ) ;
#42507 = VECTOR ( 'NONE', #23838, 1000.000000000000000 ) ;
#42508 = CARTESIAN_POINT ( 'NONE',  ( -172.4422607493951318, -177.1207230881787780, 16.06677968424543579 ) ) ;
#42509 = VECTOR ( 'NONE', #16693, 1000.000000000000000 ) ;
#42510 = CARTESIAN_POINT ( 'NONE',  ( -49.46816693883101834, -183.6283474603465606, 0.1476465640024780257 ) ) ;
#42511 = ORIENTED_EDGE ( 'NONE', *, *, #17747, .F. ) ;
#42512 = CARTESIAN_POINT ( 'NONE',  ( -168.8371699641976420, -175.3837268820161057, 33.74820638215509661 ) ) ;
#42513 = CARTESIAN_POINT ( 'NONE',  ( -100.6109117578262868, -193.5000000000000000, 112.5098962032393644 ) ) ;
#42514 = VECTOR ( 'NONE', #6511, 1000.000000000000000 ) ;
#42515 = CARTESIAN_POINT ( 'NONE',  ( -48.47912675150885065, -183.6283474603465606, 6.938893903907228378E-15 ) ) ;
#42516 = DIRECTION ( 'NONE',  ( 0.000000000000000000, 1.000000000000000000, 0.000000000000000000 ) ) ;
#42517 = VERTEX_POINT ( 'NONE', #4979 ) ;
#42518 = CARTESIAN_POINT ( 'NONE',  ( -166.1003692892502102, -183.6283474603465606, -42.31126686685032467 ) ) ;
#42519 = LINE ( 'NONE', #26749, #10588 ) ;
#42520 = DIRECTION ( 'NONE',  ( 1.000000000000000000, 0.000000000000000000, -0.000000000000000000 ) ) ;
#42521 = EDGE_LOOP ( 'NONE', ( #43482, #29764, #33978, #21566, #36800, #44685, #15409, #40457 ) ) ;
#42522 = VECTOR ( 'NONE', #10843, 1000.000000000000114 ) ;
#42523 = VECTOR ( 'NONE', #39260, 1000.000000000000000 ) ;
#42524 = ADVANCED_FACE ( 'NONE', ( #14660 ), #38044, .T. ) ;
#42525 = AXIS2_PLACEMENT_3D ( 'NONE', #10980, #14671, #50945 ) ;
#42526 = VECTOR ( 'NONE', #38693, 1000.000000000000000 ) ;
#42527 = CARTESIAN_POINT ( 'NONE',  ( -169.1033029113419559, -175.3837268820161057, 32.78426643622745473 ) ) ;
#42528 = ORIENTED_EDGE ( 'NONE', *, *, #14105, .T. ) ;
#42529 = CARTESIAN_POINT ( 'NONE',  ( 68.93474881819258826, -175.3837268820161057, 39.87457906003773900 ) ) ;
#42530 = CIRCLE ( 'NONE', #27402, 60.00000000000000000 ) ;
#42531 = ORIENTED_EDGE ( 'NONE', *, *, #6062, .F. ) ;
#42532 = VECTOR ( 'NONE', #21639, 1000.000000000000227 ) ;
#42533 = DIRECTION ( 'NONE',  ( -0.8757349421956379665, 0.000000000000000000, 0.4827922027307427477 ) ) ;
#42534 = CARTESIAN_POINT ( 'NONE',  ( -336.3521761649654422, -76.43926241122620979, -35.68215131113738181 ) ) ;
#42535 = DIRECTION ( 'NONE',  ( -0.000000000000000000, 1.000000000000000000, -0.000000000000000000 ) ) ;
#42536 = DIRECTION ( 'NONE',  ( 0.000000000000000000, -1.000000000000000000, 3.491481338843133355E-15 ) ) ;
#42537 = FACE_OUTER_BOUND ( 'NONE', #13202, .T. ) ;
#42538 = ORIENTED_EDGE ( 'NONE', *, *, #50762, .T. ) ;
#42539 = CARTESIAN_POINT ( 'NONE',  ( -332.3517673607765914, -123.5000000000000284, 0.000000000000000000 ) ) ;
#42540 = ORIENTED_EDGE ( 'NONE', *, *, #21802, .F. ) ;
#42541 = CARTESIAN_POINT ( 'NONE',  ( -168.4003408533108086, -177.1207230881787780, -35.26900067126609173 ) ) ;
#42542 = AXIS2_PLACEMENT_3D ( 'NONE', #12973, #21126, #21389 ) ;
#42543 = AXIS2_PLACEMENT_3D ( 'NONE', #10531, #46547, #15256 ) ;
#42544 = ORIENTED_EDGE ( 'NONE', *, *, #43744, .F. ) ;
#42545 = DIRECTION ( 'NONE',  ( -0.000000000000000000, 1.000000000000000000, -0.000000000000000000 ) ) ;
#42546 = AXIS2_PLACEMENT_3D ( 'NONE', #47388, #4270, #20292 ) ;
#42547 = EDGE_CURVE ( 'NONE', #38590, #5830, #6248, .T. ) ;
#42548 = EDGE_CURVE ( 'NONE', #3342, #17596, #29906, .T. ) ;
#42549 = DIRECTION ( 'NONE',  ( 0.000000000000000000, 1.000000000000000000, 0.000000000000000000 ) ) ;
#42550 = LINE ( 'NONE', #50205, #18083 ) ;
#42551 = EDGE_LOOP ( 'NONE', ( #43013, #48120, #40909, #47519 ) ) ;
#42554 = ORIENTED_EDGE ( 'NONE', *, *, #26880, .T. ) ;
#42553 = DIRECTION ( 'NONE',  ( 0.000000000000000000, 0.000000000000000000, 1.000000000000000000 ) ) ;
#42552 = CARTESIAN_POINT ( 'NONE',  ( -4.317676980897452665, 53.18341953714510595, -19.20431157105264219 ) ) ;
#42555 = AXIS2_PLACEMENT_3D ( 'NONE', #14625, #34336, #30133 ) ;
#42556 = CIRCLE ( 'NONE', #47643, 125.0000000000000000 ) ;
#42557 = AXIS2_PLACEMENT_3D ( 'NONE', #13740, #17446, #1660 ) ;
#42558 = CARTESIAN_POINT ( 'NONE',  ( -67.10529315269985773, -177.1207230881787780, -122.5936119678274423 ) ) ;
#42559 = EDGE_LOOP ( 'NONE', ( #12412, #13555, #36538, #25135 ) ) ;
#42560 = CARTESIAN_POINT ( 'NONE',  ( 55.10060313344061456, -183.6283474603465606, 68.17212999877223467 ) ) ;
#42561 = ORIENTED_EDGE ( 'NONE', *, *, #17473, .T. ) ;
#42562 = EDGE_CURVE ( 'NONE', #21060, #35361, #14935, .T. ) ;
#42563 = CONICAL_SURFACE ( 'NONE', #35031, 20.00000000000000355, 0.4363323129985833826 ) ;
#42564 = CARTESIAN_POINT ( 'NONE',  ( -339.1964088526558498, -175.9742670995610752, 26.97593913775620678 ) ) ;
#42567 = ORIENTED_EDGE ( 'NONE', *, *, #23560, .F. ) ;
#42566 = DIRECTION ( 'NONE',  ( -0.1768902751225592818, 0.000000000000000000, -0.9842305779475992722 ) ) ;
#42565 = CARTESIAN_POINT ( 'NONE',  ( -161.6832731452239784, -193.5000000000000000, -53.00774697410100345 ) ) ;
#42568 = VERTEX_POINT ( 'NONE', #43028 ) ;
#42569 = EDGE_CURVE ( 'NONE', #11314, #28854, #7035, .T. ) ;
#42570 = EDGE_CURVE ( 'NONE', #13751, #3383, #1789, .T. ) ;
#42571 = AXIS2_PLACEMENT_3D ( 'NONE', #51494, #43851, #15493 ) ;
#42572 = LINE ( 'NONE', #10014, #36597 ) ;
#42573 = ORIENTED_EDGE ( 'NONE', *, *, #14812, .F. ) ;
#42574 = DIRECTION ( 'NONE',  ( -1.000000000000000000, 0.000000000000000000, 0.000000000000000000 ) ) ;
#42575 = EDGE_CURVE ( 'NONE', #45145, #29008, #34373, .T. ) ;
#42576 = ORIENTED_EDGE ( 'NONE', *, *, #15999, .T. ) ;
#42577 = EDGE_CURVE ( 'NONE', #37376, #19422, #41989, .T. ) ;
#42578 = DIRECTION ( 'NONE',  ( -0.000000000000000000, 1.000000000000000000, -0.000000000000000000 ) ) ;
#42579 = DIRECTION ( 'NONE',  ( 0.000000000000000000, -0.6631226582407863113, 0.7485107481711089639 ) ) ;
#42580 = LINE ( 'NONE', #2889, #40823 ) ;
#42581 = FACE_OUTER_BOUND ( 'NONE', #21242, .T. ) ;
#42582 = LINE ( 'NONE', #26804, #50937 ) ;
#42583 = VERTEX_POINT ( 'NONE', #25969 ) ;
#42584 =( NAMED_UNIT ( * ) PLANE_ANGLE_UNIT ( ) SI_UNIT ( $, .RADIAN. ) );
#42585 = DIRECTION ( 'NONE',  ( -1.000000000000000000, 0.000000000000000000, 0.000000000000000000 ) ) ;
#42586 = DIRECTION ( 'NONE',  ( 0.000000000000000000, 0.000000000000000000, 1.000000000000000000 ) ) ;
#42587 = CARTESIAN_POINT ( 'NONE',  ( -339.1964088526558498, -84.00150778970699150, 43.83057281297409702 ) ) ;
#42588 = VERTEX_POINT ( 'NONE', #14158 ) ;
#42589 = VECTOR ( 'NONE', #47236, 1000.000000000000000 ) ;
#42590 = VECTOR ( 'NONE', #14987, 1000.000000000000000 ) ;
#42591 = DIRECTION ( 'NONE',  ( -0.000000000000000000, -0.1205366802553130001, 0.9927088740980551940 ) ) ;
#42592 = FACE_OUTER_BOUND ( 'NONE', #37662, .T. ) ;
#42593 = CIRCLE ( 'NONE', #14924, 125.0000000000000000 ) ;
#42594 = CARTESIAN_POINT ( 'NONE',  ( -48.47912675150885065, -177.1207230881787780, 6.938893903907228378E-15 ) ) ;
#42595 = DIRECTION ( 'NONE',  ( 0.9646355819083576311, 0.000000000000000000, 0.2635871660690715101 ) ) ;
#42596 = ORIENTED_EDGE ( 'NONE', *, *, #1912, .T. ) ;
#42597 = AXIS2_PLACEMENT_3D ( 'NONE', #22456, #30321, #14057 ) ;
#42598 = CIRCLE ( 'NONE', #22472, 125.0000000000000000 ) ;
#42599 = CARTESIAN_POINT ( 'NONE',  ( -40.90423906728906900, -189.7472609257535510, -124.7702732086912505 ) ) ;
#42600 = CARTESIAN_POINT ( 'NONE',  ( -131.1972941934623975, -177.1207230881787780, 92.37913469314123915 ) ) ;
#42601 = LINE ( 'NONE', #50755, #35427 ) ;
#42602 = AXIS2_PLACEMENT_3D ( 'NONE', #13874, #49875, #5988 ) ;
#42603 = VERTEX_POINT ( 'NONE', #6000 ) ;
#42604 = AXIS2_PLACEMENT_3D ( 'NONE', #21588, #26801, #14998 ) ;
#42605 = CARTESIAN_POINT ( 'NONE',  ( -47.97059563285962724, -193.5000000000000000, -0.8610436117673480050 ) ) ;
#42606 = VECTOR ( 'NONE', #38144, 1000.000000000000114 ) ;
#42607 = DIRECTION ( 'NONE',  ( 0.000000000000000000, 1.000000000000000000, -0.000000000000000000 ) ) ;
#42608 = ORIENTED_EDGE ( 'NONE', *, *, #8415, .F. ) ;
#42609 = VERTEX_POINT ( 'NONE', #30175 ) ;
#42610 = ORIENTED_EDGE ( 'NONE', *, *, #14125, .F. ) ;
#42611 = DIRECTION ( 'NONE',  ( 0.000000000000000000, 0.1205366802553233113, 0.9927088740980538617 ) ) ;
#42612 = EDGE_CURVE ( 'NONE', #12830, #5877, #14408, .T. ) ;
#42613 = ADVANCED_FACE ( 'NONE', ( #51977 ), #15963, .T. ) ;
#42614 = EDGE_CURVE ( 'NONE', #31046, #6126, #3599, .T. ) ;
#42615 = DIRECTION ( 'NONE',  ( 0.5085311186492216251, 0.000000000000000000, -0.8610436117673548884 ) ) ;
#42616 = DIRECTION ( 'NONE',  ( -0.000000000000000000, 1.000000000000000000, -0.000000000000000000 ) ) ;
#42617 = ORIENTED_EDGE ( 'NONE', *, *, #46613, .F. ) ;
#42618 = CARTESIAN_POINT ( 'NONE',  ( -160.3527926973206661, -175.3837268820161057, -53.48161459190840361 ) ) ;
#42619 = PLANE ( 'NONE',  #40293 ) ;
#42620 = VECTOR ( 'NONE', #23759, 1000.000000000000000 ) ;
#42623 = ORIENTED_EDGE ( 'NONE', *, *, #33303, .T. ) ;
#42622 = FACE_OUTER_BOUND ( 'NONE', #43372, .T. ) ;
#42621 = CARTESIAN_POINT ( 'NONE',  ( -48.47912675150885065, -189.7472609257535510, 6.938893903907228378E-15 ) ) ;
#42624 = CIRCLE ( 'NONE', #19968, 60.00000000000000000 ) ;
#42625 = EDGE_CURVE ( 'NONE', #4472, #37318, #48272, .T. ) ;
#42626 = PLANE ( 'NONE',  #27255 ) ;
#42627 = ORIENTED_EDGE ( 'NONE', *, *, #40096, .F. ) ;
#42628 = CYLINDRICAL_SURFACE ( 'NONE', #38148, 125.0000000000000000 ) ;
#42629 = AXIS2_PLACEMENT_3D ( 'NONE', #44746, #31876, #3495 ) ;
#42630 = VERTEX_POINT ( 'NONE', #15708 ) ;
#42631 = CARTESIAN_POINT ( 'NONE',  ( -133.0671220150036049, -183.6283474603465606, -92.03190238880749519 ) ) ;
#42632 = EDGE_CURVE ( 'NONE', #30980, #7704, #51198, .T. ) ;
#42633 = CARTESIAN_POINT ( 'NONE',  ( -47.49008656418669005, -193.5000000000000000, -0.1476465640024710591 ) ) ;
#42634 = CARTESIAN_POINT ( 'NONE',  ( -49.38192458147459263, -189.7472609257535510, -0.4300652022765235616 ) ) ;
#42635 = EDGE_CURVE ( 'NONE', #47506, #48534, #16213, .T. ) ;
#42636 = AXIS2_PLACEMENT_3D ( 'NONE', #23600, #15473, #38854 ) ;
#42637 = ORIENTED_EDGE ( 'NONE', *, *, #45255, .F. ) ;
#42638 = CARTESIAN_POINT ( 'NONE',  ( 4.109287492203097081, -183.6283474603465606, -113.3995532942337121 ) ) ;
#42639 = ADVANCED_FACE ( 'NONE', ( #23829 ), #15184, .T. ) ;
#42640 = LINE ( 'NONE', #22926, #5727 ) ;
#42641 = ORIENTED_EDGE ( 'NONE', *, *, #20939, .T. ) ;
#42642 = CARTESIAN_POINT ( 'NONE',  ( 69.14211578623219623, -193.5000000000000000, 42.31126686685117733 ) ) ;
#42643 = CARTESIAN_POINT ( 'NONE',  ( -330.4913330509368166, -143.9541802141664562, 55.34326076196094135 ) ) ;
#42644 = EDGE_CURVE ( 'NONE', #6231, #22760, #31724, .T. ) ;
#42645 = VERTEX_POINT ( 'NONE', #11992 ) ;
#42646 = FACE_BOUND ( 'NONE', #3740, .T. ) ;
#42647 = CARTESIAN_POINT ( 'NONE',  ( -305.0000000000000568, -70.14212160686619768, -27.43969411971536942 ) ) ;
#42648 = VECTOR ( 'NONE', #7838, 1000.000000000000000 ) ;
#42649 = VERTEX_POINT ( 'NONE', #28020 ) ;
#42650 = CARTESIAN_POINT ( 'NONE',  ( -162.9896759831413249, -193.5000000000000000, -50.12318939043961308 ) ) ;
#42651 = EDGE_LOOP ( 'NONE', ( #35542, #37519, #32910, #18789 ) ) ;
#42652 = CARTESIAN_POINT ( 'NONE',  ( -65.65563056894595206, -177.1207230881787780, 123.8142468240612857 ) ) ;
#42653 = LINE ( 'NONE', #9558, #40324 ) ;
#42654 = VERTEX_POINT ( 'NONE', #3084 ) ;
#42655 = LINE ( 'NONE', #45829, #50046 ) ;
#42656 = FACE_OUTER_BOUND ( 'NONE', #27145, .T. ) ;
#42657 = DIRECTION ( 'NONE',  ( -0.9890401873221623674, 0.000000000000000000, -0.1476465640024917925 ) ) ;
#42658 = ADVANCED_FACE ( 'NONE', ( #44061 ), #8065, .T. ) ;
#42659 = VERTEX_POINT ( 'NONE', #25394 ) ;
#42660 = CARTESIAN_POINT ( 'NONE',  ( 75.12566530717464275, -193.5000000000000000, 18.62405380494841367 ) ) ;
#42661 =( GEOMETRIC_REPRESENTATION_CONTEXT ( 3 ) GLOBAL_UNCERTAINTY_ASSIGNED_CONTEXT ( ( #33770 ) ) GLOBAL_UNIT_ASSIGNED_CONTEXT ( ( #6076, #22355, #46288 ) ) REPRESENTATION_CONTEXT ( 'NONE', 'WORKASPACE' ) );
#42662 = CIRCLE ( 'NONE', #1555, 124.9999999999999858 ) ;
#42663 = AXIS2_PLACEMENT_3D ( 'NONE', #45731, #40727, #13151 ) ;
#42664 = CARTESIAN_POINT ( 'NONE',  ( 14.37129481273059106, -193.5000000000000000, -108.0501018472328241 ) ) ;
#42665 = LINE ( 'NONE', #34762, #12590 ) ;
#42667 = ORIENTED_EDGE ( 'NONE', *, *, #38702, .F. ) ;
#42666 = LINE ( 'NONE', #39483, #32884 ) ;
#42668 = VECTOR ( 'NONE', #49732, 1000.000000000000000 ) ;
#42669 = VERTEX_POINT ( 'NONE', #28536 ) ;
#42670 = LINE ( 'NONE', #30843, #47596 ) ;
#42671 = EDGE_CURVE ( 'NONE', #4717, #42476, #10222, .T. ) ;
#42672 = DIRECTION ( 'NONE',  ( -8.718379230999705894E-17, -0.7485107481711069655, -0.6631226582407885317 ) ) ;
#42673 = CIRCLE ( 'NONE', #48579, 125.0000000000000000 ) ;
#42674 = ORIENTED_EDGE ( 'NONE', *, *, #5373, .F. ) ;
#42675 = CARTESIAN_POINT ( 'NONE',  ( 68.72094416275764672, -175.3837268820161057, -40.49875167738976955 ) ) ;
#42676 = ORIENTED_EDGE ( 'NONE', *, *, #51003, .F. ) ;
#42677 = CARTESIAN_POINT ( 'NONE',  ( -305.0000000000000568, -183.4422309845877805, 2.632288850093980503 ) ) ;
#42678 = DIRECTION ( 'NONE',  ( -0.000000000000000000, -0.9350162426854169428, -0.3546048870425300148 ) ) ;
#42679 = EDGE_CURVE ( 'NONE', #27297, #39129, #51353, .T. ) ;
#42680 = ADVANCED_FACE ( 'NONE', ( #45637 ), #8831, .T. ) ;
#42681 = EDGE_CURVE ( 'NONE', #28401, #18318, #125, .T. ) ;
#42682 = EDGE_CURVE ( 'NONE', #42318, #46650, #8571, .T. ) ;
#42683 = DIRECTION ( 'NONE',  ( -0.000000000000000000, 0.2393156642875547968, -0.9709418174260527890 ) ) ;
#42684 = FACE_OUTER_BOUND ( 'NONE', #11804, .T. ) ;
#42685 = VERTEX_POINT ( 'NONE', #13559 ) ;
#42686 = ORIENTED_EDGE ( 'NONE', *, *, #32659, .T. ) ;
#42687 = EDGE_CURVE ( 'NONE', #25337, #21157, #21188, .T. ) ;
#42688 = ORIENTED_EDGE ( 'NONE', *, *, #49078, .F. ) ;
#42689 = CIRCLE ( 'NONE', #30905, 125.0000000000000000 ) ;
#42690 = CARTESIAN_POINT ( 'NONE',  ( -9.671950287350391307, -183.6283474603465606, -118.8234112238815499 ) ) ;
#42691 = DIRECTION ( 'NONE',  ( 0.000000000000000000, 0.000000000000000000, 1.000000000000000000 ) ) ;
#42692 = EDGE_CURVE ( 'NONE', #7764, #23663, #24604, .T. ) ;
#42693 = LINE ( 'NONE', #39506, #41292 ) ;
#42694 = CARTESIAN_POINT ( 'NONE',  ( -336.3521761649654422, -123.5000000000000284, 0.000000000000000000 ) ) ;
#42695 = VERTEX_POINT ( 'NONE', #40615 ) ;
#42696 = UNCERTAINTY_MEASURE_WITH_UNIT (LENGTH_MEASURE( 1.000000000000000082E-05 ), #32535, 'distance_accuracy_value', 'NONE');
#42697 = EDGE_CURVE ( 'NONE', #21438, #34375, #4377, .T. ) ;
#42698 = DIRECTION ( 'NONE',  ( 0.000000000000000000, 0.000000000000000000, 1.000000000000000000 ) ) ;
#42699 = CARTESIAN_POINT ( 'NONE',  ( 76.31829002442924548, -183.6283474603465606, 7.113702696402428138 ) ) ;
#42700 = ADVANCED_FACE ( 'NONE', ( #4636 ), #13033, .F. ) ;
#42701 = ORIENTED_EDGE ( 'NONE', *, *, #4078, .T. ) ;
#42702 = ORIENTED_EDGE ( 'NONE', *, *, #47796, .F. ) ;
#42703 = PLANE ( 'NONE',  #5430 ) ;
#42704 = CIRCLE ( 'NONE', #26754, 125.0000000000000000 ) ;
#42705 = DIRECTION ( 'NONE',  ( 0.000000000000000000, 0.9927088740980534176, -0.1205366802553268502 ) ) ;
#42706 = ADVANCED_FACE ( 'NONE', ( #1200 ), #28794, .T. ) ;
#42708 = PRESENTATION_LAYER_ASSIGNMENT (  '', '', ( #13332 ) ) ;
#42707 = FACE_OUTER_BOUND ( 'NONE', #348, .T. ) ;
#42709 = DIRECTION ( 'NONE',  ( 0.000000000000000000, 1.000000000000000000, 0.000000000000000000 ) ) ;
#42710 = VECTOR ( 'NONE', #11252, 1000.000000000000114 ) ;
#42711 = EDGE_CURVE ( 'NONE', #30763, #43156, #36701, .T. ) ;
#42712 = CARTESIAN_POINT ( 'NONE',  ( -336.3521761649654422, -168.7445418633863596, -37.90245108779149064 ) ) ;
#42713 = CARTESIAN_POINT ( 'NONE',  ( 0.000000000000000000, 51.50530197288473744, -13.91328567938375294 ) ) ;
#42714 = ORIENTED_EDGE ( 'NONE', *, *, #25842, .F. ) ;
#42715 = DIRECTION ( 'NONE',  ( -0.000000000000000000, -0.3546048870425267951, 0.9350162426854181641 ) ) ;
#42716 = EDGE_CURVE ( 'NONE', #6875, #29368, #33275, .T. ) ;
#42717 = ORIENTED_EDGE ( 'NONE', *, *, #18153, .F. ) ;
#42718 = CARTESIAN_POINT ( 'NONE',  ( -332.3517673607765914, -181.8730728925770563, 8.732051761644092025 ) ) ;
#42719 = AXIS2_PLACEMENT_3D ( 'NONE', #2533, #46425, #9910 ) ;
#42720 = DIRECTION ( 'NONE',  ( -0.6965510290629882695, 0.000000000000000000, -0.7175072570443395970 ) ) ;
#42721 = VERTEX_POINT ( 'NONE', #16750 ) ;
#42722 = PLANE ( 'NONE',  #3021 ) ;
#42723 = FACE_OUTER_BOUND ( 'NONE', #34214, .T. ) ;
#42724 = DIRECTION ( 'NONE',  ( 0.9982437317643217956, 0.000000000000000000, -0.05924062789370748011 ) ) ;
#42725 = PLANE ( 'NONE',  #45864 ) ;
#42726 = EDGE_CURVE ( 'NONE', #33386, #18911, #13307, .T. ) ;
#42727 = CIRCLE ( 'NONE', #9152, 125.0000000000000000 ) ;
#42728 = EDGE_CURVE ( 'NONE', #49241, #27624, #44842, .T. ) ;
#42729 = DIRECTION ( 'NONE',  ( 0.000000000000000000, 0.2393156642875685636, 0.9709418174260492362 ) ) ;
#42730 = ORIENTED_EDGE ( 'NONE', *, *, #5199, .F. ) ;
#42731 = PLANE ( 'NONE',  #17752 ) ;
#42732 = ORIENTED_EDGE ( 'NONE', *, *, #2741, .T. ) ;
#42733 = ORIENTED_EDGE ( 'NONE', *, *, #38484, .T. ) ;
#42734 = CARTESIAN_POINT ( 'NONE',  ( -26.53529504715431031, -189.7472609257535510, 123.0587999703026725 ) ) ;
#42735 = ORIENTED_EDGE ( 'NONE', *, *, #2145, .T. ) ;
#42736 = CARTESIAN_POINT ( 'NONE',  ( -339.1964088526558498, -71.02573290043838483, 26.97593913775504504 ) ) ;
#42737 = ORIENTED_EDGE ( 'NONE', *, *, #42437, .T. ) ;
#42738 = AXIS2_PLACEMENT_3D ( 'NONE', #24894, #12274, #40639 ) ;
#42739 = LINE ( 'NONE', #27728, #45767 ) ;
#42740 = DIRECTION ( 'NONE',  ( 0.000000000000000000, 1.000000000000000000, 0.000000000000000000 ) ) ;
#42741 = ORIENTED_EDGE ( 'NONE', *, *, #33425, .T. ) ;
#42742 = FACE_OUTER_BOUND ( 'NONE', #41316, .T. ) ;
#42743 = VECTOR ( 'NONE', #4109, 1000.000000000000000 ) ;
#42744 = EDGE_CURVE ( 'NONE', #39966, #44982, #29582, .T. ) ;
#42745 = EDGE_CURVE ( 'NONE', #40405, #13290, #20940, .T. ) ;
#42746 = DIRECTION ( 'NONE',  ( -0.000000000000000000, 1.000000000000000000, -0.000000000000000000 ) ) ;
#42747 = FACE_OUTER_BOUND ( 'NONE', #42934, .T. ) ;
#42748 = VERTEX_POINT ( 'NONE', #37474 ) ;
#42749 = EDGE_LOOP ( 'NONE', ( #3851, #23187, #37809, #41075 ) ) ;
#42750 = ORIENTED_EDGE ( 'NONE', *, *, #1824, .T. ) ;
#42751 = ADVANCED_FACE ( 'NONE', ( #40357 ), #1479, .T. ) ;
#42752 = CARTESIAN_POINT ( 'NONE',  ( -339.1964088526558498, -123.5000000000000284, 0.000000000000000000 ) ) ;
#42753 = LINE ( 'NONE', #6756, #30199 ) ;
#42754 = DIRECTION ( 'NONE',  ( 0.000000000000000000, -0.8854560256532141294, -0.4647231720437604574 ) ) ;
#42755 = DIRECTION ( 'NONE',  ( -0.000000000000000000, 0.9927088740980556381, 0.1205366802553095307 ) ) ;
#42756 = LINE ( 'NONE', #2551, #27210 ) ;
#42757 = ORIENTED_EDGE ( 'NONE', *, *, #14238, .T. ) ;
#42758 = VECTOR ( 'NONE', #22619, 1000.000000000000000 ) ;
#42759 = DIRECTION ( 'NONE',  ( 0.000000000000000000, 0.000000000000000000, 1.000000000000000000 ) ) ;
#42760 = ORIENTED_EDGE ( 'NONE', *, *, #27428, .F. ) ;
#42762 = EDGE_LOOP ( 'NONE', ( #22706, #6631, #39734, #27105 ) ) ;
#42761 = DIRECTION ( 'NONE',  ( 0.000000000000000000, 0.000000000000000000, -1.000000000000000000 ) ) ;
#42763 = VERTEX_POINT ( 'NONE', #26150 ) ;
#42764 = DIRECTION ( 'NONE',  ( -0.9960498426152165630, 0.000000000000000000, -0.08879589532293852283 ) ) ;
#42765 = ADVANCED_FACE ( 'NONE', ( #13824 ), #10135, .T. ) ;
#42766 = LINE ( 'NONE', #41977, #16583 ) ;
#42767 = DIRECTION ( 'NONE',  ( 1.000000000000000000, -0.000000000000000000, -0.000000000000000000 ) ) ;
#42768 = DIRECTION ( 'NONE',  ( 0.6068001458185890984, 0.000000000000000000, 0.7948544414133565938 ) ) ;
#42769 = ORIENTED_EDGE ( 'NONE', *, *, #40345, .T. ) ;
#42770 = DIRECTION ( 'NONE',  ( 0.000000000000000000, 0.8854560256532126861, 0.4647231720437631775 ) ) ;
#42771 = EDGE_LOOP ( 'NONE', ( #37439, #46421, #31398, #21895 ) ) ;
#42772 = ADVANCED_FACE ( 'NONE', ( #14091 ), #1733, .T. ) ;
#42773 = ORIENTED_EDGE ( 'NONE', *, *, #36602, .T. ) ;
#42774 = DIRECTION ( 'NONE',  ( -0.000000000000000000, 1.000000000000000000, -0.000000000000000000 ) ) ;
#42775 = DIRECTION ( 'NONE',  ( -0.000000000000000000, 1.000000000000000000, -0.000000000000000000 ) ) ;
#42776 = CIRCLE ( 'NONE', #27653, 125.0000000000000000 ) ;
#42777 = PLANE ( 'NONE',  #19013 ) ;
#42778 = EDGE_LOOP ( 'NONE', ( #26460, #18324, #47816, #24231 ) ) ;
#42779 = PLANE ( 'NONE',  #22324 ) ;
#42780 = CARTESIAN_POINT ( 'NONE',  ( 57.12946453413545100, -175.3837268820161057, 66.87170886602000053 ) ) ;
#42781 = DIRECTION ( 'NONE',  ( -1.000000000000000000, 0.000000000000000000, 0.000000000000000000 ) ) ;
#42782 = DIRECTION ( 'NONE',  ( 0.000000000000000000, 0.3546048870425463906, 0.9350162426854107256 ) ) ;
#42783 = ORIENTED_EDGE ( 'NONE', *, *, #51349, .F. ) ;
#42784 = DIRECTION ( 'NONE',  ( -0.9027978299657446470, 0.000000000000000000, 0.4300652022765183435 ) ) ;
#42785 = CARTESIAN_POINT ( 'NONE',  ( -330.4913330509368166, -79.00630452878421295, 38.74998146212088557 ) ) ;
#42786 = LINE ( 'NONE', #34880, #23220 ) ;
#42787 = EDGE_LOOP ( 'NONE', ( #20883, #15101, #44750, #18668 ) ) ;
#42788 = DIRECTION ( 'NONE',  ( -0.5338233779648003940, 0.000000000000000000, 0.8455960035018199594 ) ) ;
#42789 = ORIENTED_EDGE ( 'NONE', *, *, #32885, .T. ) ;
#42790 = DIRECTION ( 'NONE',  ( -0.6749830015182196608, 0.000000000000000000, 0.7378332790417189146 ) ) ;
#42791 = VERTEX_POINT ( 'NONE', #22740 ) ;
#42792 = AXIS2_PLACEMENT_3D ( 'NONE', #40594, #13004, #17227 ) ;
#42793 = VECTOR ( 'NONE', #36652, 1000.000000000000000 ) ;
#42794 = DIRECTION ( 'NONE',  ( 0.000000000000000000, 0.000000000000000000, 1.000000000000000000 ) ) ;
#42795 = DIRECTION ( 'NONE',  ( 0.3482016354343866471, 0.000000000000000000, 0.9374196611341253371 ) ) ;
#42796 = CARTESIAN_POINT ( 'NONE',  ( -336.3521761649654422, -164.5945333327934463, -42.41660376256285048 ) ) ;
#42797 = DIRECTION ( 'NONE',  ( -0.8455960035018199594, 0.000000000000000000, -0.5338233779648003940 ) ) ;
#42798 = EDGE_CURVE ( 'NONE', #22690, #41798, #10655, .T. ) ;
#42799 = FACE_OUTER_BOUND ( 'NONE', #2780, .T. ) ;
#42800 = ORIENTED_EDGE ( 'NONE', *, *, #20231, .F. ) ;
#42801 = PLANE ( 'NONE',  #18114 ) ;
#42802 = ORIENTED_EDGE ( 'NONE', *, *, #41373, .T. ) ;
#42803 = DIRECTION ( 'NONE',  ( 0.000000000000000000, 0.000000000000000000, -1.000000000000000000 ) ) ;
#42804 = CIRCLE ( 'NONE', #11739, 125.0000000000000000 ) ;
#42805 = ORIENTED_EDGE ( 'NONE', *, *, #4115, .T. ) ;
#42806 = PLANE ( 'NONE',  #26757 ) ;
#42807 = LINE ( 'NONE', #30460, #41842 ) ;
#42808 = PLANE ( 'NONE',  #48399 ) ;
#42809 = ORIENTED_EDGE ( 'NONE', *, *, #9534, .T. ) ;
#42812 = ORIENTED_EDGE ( 'NONE', *, *, #34256, .F. ) ;
#42811 = DIRECTION ( 'NONE',  ( -0.000000000000000000, 1.000000000000000000, 0.000000000000000000 ) ) ;
#42810 = LINE ( 'NONE', #10758, #48521 ) ;
#42813 = EDGE_CURVE ( 'NONE', #33858, #17577, #25908, .T. ) ;
#42814 = DIRECTION ( 'NONE',  ( -0.000000000000000000, 1.000000000000000000, -0.000000000000000000 ) ) ;
#42815 = ORIENTED_EDGE ( 'NONE', *, *, #9475, .F. ) ;
#42816 = DIRECTION ( 'NONE',  ( -0.000000000000000000, 1.000000000000000000, -0.000000000000000000 ) ) ;
#42817 = ORIENTED_EDGE ( 'NONE', *, *, #38818, .F. ) ;
#42818 = DIRECTION ( 'NONE',  ( -0.000000000000000000, 0.6631226582408039638, 0.7485107481710934207 ) ) ;
#42819 = EDGE_LOOP ( 'NONE', ( #42088, #48267, #36014, #51035 ) ) ;
#42822 = ORIENTED_EDGE ( 'NONE', *, *, #5737, .T. ) ;
#42821 = PLANE ( 'NONE',  #6517 ) ;
#42820 = DIRECTION ( 'NONE',  ( -0.9266896074318370369, 0.000000000000000000, 0.3758275821142292306 ) ) ;
#42823 = ORIENTED_EDGE ( 'NONE', *, *, #12521, .T. ) ;
#42824 = VECTOR ( 'NONE', #28961, 1000.000000000000000 ) ;
#42825 = CARTESIAN_POINT ( 'NONE',  ( -173.4460699164830260, -193.5000000000000000, -2.874563619423202265 ) ) ;
#42826 = EDGE_LOOP ( 'NONE', ( #49047, #42458, #45473, #12940 ) ) ;
#42827 = CARTESIAN_POINT ( 'NONE',  ( -336.3521761649654422, -86.34605966037949543, -45.90766452162698386 ) ) ;
#42828 = CARTESIAN_POINT ( 'NONE',  ( -158.3442440847887269, -189.7472609257535510, -59.62093586438114556 ) ) ;
#42829 = EDGE_LOOP ( 'NONE', ( #8404, #25757, #40418, #15496 ) ) ;
#42830 = EDGE_CURVE ( 'NONE', #50621, #34413, #47149, .T. ) ;
#42831 = CARTESIAN_POINT ( 'NONE',  ( -336.3521761649654422, -158.3591674452439122, -47.62880233550485087 ) ) ;
#42832 = CARTESIAN_POINT ( 'NONE',  ( -9.070200226166599933, -193.5000000000000000, -117.5715283571804122 ) ) ;
#42833 = CARTESIAN_POINT ( 'NONE',  ( -339.1964088526558498, -144.8891964568526305, -54.98865587491811624 ) ) ;
#42834 = DIRECTION ( 'NONE',  ( 0.000000000000000000, 1.000000000000000000, -0.000000000000000000 ) ) ;
#42835 = ORIENTED_EDGE ( 'NONE', *, *, #4942, .T. ) ;
#42836 = EDGE_CURVE ( 'NONE', #50802, #16302, #46662, .T. ) ;
#42837 = DIRECTION ( 'NONE',  ( 0.000000000000000000, 0.000000000000000000, 1.000000000000000000 ) ) ;
#42838 = CARTESIAN_POINT ( 'NONE',  ( -339.1964088526558498, -71.02573290043838483, 26.97593913775504504 ) ) ;
#42839 = DIRECTION ( 'NONE',  ( 0.000000000000000000, 1.000000000000000000, 0.000000000000000000 ) ) ;
#42840 = ORIENTED_EDGE ( 'NONE', *, *, #13185, .T. ) ;
#42841 = AXIS2_PLACEMENT_3D ( 'NONE', #50693, #43577, #27275 ) ;
#42842 = DIRECTION ( 'NONE',  ( 0.7575112421616145841, 0.000000000000000000, 0.6528221181905280446 ) ) ;
#42843 = CARTESIAN_POINT ( 'NONE',  ( -170.7635349987907318, -175.3837268820161057, -25.91377046305876775 ) ) ;
#42844 = CARTESIAN_POINT ( 'NONE',  ( -330.4913330509368166, -123.5000000000000284, 0.000000000000000000 ) ) ;
#42845 = DIRECTION ( 'NONE',  ( 0.000000000000000000, 0.9350162426854158326, 0.3546048870425331234 ) ) ;
#42846 = CARTESIAN_POINT ( 'NONE',  ( 0.000000000000000000, -53.50000000000000000, -16.00000000000000000 ) ) ;
#42847 = ORIENTED_EDGE ( 'NONE', *, *, #41210, .F. ) ;
#42848 = EDGE_CURVE ( 'NONE', #28285, #43244, #37042, .T. ) ;
#42849 = PLANE ( 'NONE',  #212 ) ;
#42850 = CARTESIAN_POINT ( 'NONE',  ( -336.3521761649653854, -88.08538291676191534, 48.43351006119235080 ) ) ;
#42851 = LINE ( 'NONE', #22115, #2682 ) ;
#42852 = DIRECTION ( 'NONE',  ( 0.000000000000000000, -1.000000000000000000, 0.000000000000000000 ) ) ;
#42853 = PLANE ( 'NONE',  #34612 ) ;
#42854 = VECTOR ( 'NONE', #108, 1000.000000000000227 ) ;
#42855 = ORIENTED_EDGE ( 'NONE', *, *, #33659, .F. ) ;
#42856 = EDGE_CURVE ( 'NONE', #14293, #150, #33787, .T. ) ;
#42857 = LINE ( 'NONE', #34972, #10923 ) ;
#42858 = EDGE_CURVE ( 'NONE', #6302, #265, #1818, .T. ) ;
#42859 = VECTOR ( 'NONE', #26586, 1000.000000000000000 ) ;
#42860 = VECTOR ( 'NONE', #44926, 1000.000000000000000 ) ;
#42861 = DIRECTION ( 'NONE',  ( 0.000000000000000000, 1.000000000000000000, 0.000000000000000000 ) ) ;
#42862 = ORIENTED_EDGE ( 'NONE', *, *, #14687, .F. ) ;
#42863 = ORIENTED_EDGE ( 'NONE', *, *, #35668, .T. ) ;
#42864 = EDGE_CURVE ( 'NONE', #20728, #29853, #9374, .T. ) ;
#42865 = EDGE_LOOP ( 'NONE', ( #29278, #22768, #7695, #35230 ) ) ;
#42866 = DIRECTION ( 'NONE',  ( -1.000000000000000000, 0.000000000000000000, 0.000000000000000000 ) ) ;
#42867 = CARTESIAN_POINT ( 'NONE',  ( -48.36085358058748795, -193.5000000000000000, 0.9929810960135245779 ) ) ;
#42868 = DIRECTION ( 'NONE',  ( -0.000000000000000000, 0.9350162426854146114, -0.3546048870425363986 ) ) ;
#42869 = ORIENTED_EDGE ( 'NONE', *, *, #15375, .F. ) ;
#42870 = CARTESIAN_POINT ( 'NONE',  ( -332.3517673607765914, -177.7325358280884586, 23.38292116578760726 ) ) ;
#42871 = CARTESIAN_POINT ( 'NONE',  ( -84.82349129030161805, -189.7472609257535510, -119.5996955107802080 ) ) ;
#42874 = ORIENTED_EDGE ( 'NONE', *, *, #43007, .T. ) ;
#42873 = PLANE ( 'NONE',  #12351 ) ;
#42872 = DIRECTION ( 'NONE',  ( 0.000000000000000000, 1.000000000000000000, 0.000000000000000000 ) ) ;
#42875 = CIRCLE ( 'NONE', #11805, 16.00000000000000711 ) ;
#42876 = ADVANCED_FACE ( 'NONE', ( #50604 ), #14601, .T. ) ;
#42877 = CARTESIAN_POINT ( 'NONE',  ( 69.66827051661184100, -193.5000000000000000, -40.81902153125260213 ) ) ;
#42878 = ORIENTED_EDGE ( 'NONE', *, *, #12627, .F. ) ;
#42879 = DIRECTION ( 'NONE',  ( 0.000000000000000000, -1.000000000000000000, 0.000000000000000000 ) ) ;
#42880 = EDGE_LOOP ( 'NONE', ( #27932, #47551, #36406, #39937 ) ) ;
#42881 = CARTESIAN_POINT ( 'NONE',  ( -365.0160704661291788, -93.50000000000001421, -51.54700538379269403 ) ) ;
#42882 = CARTESIAN_POINT ( 'NONE',  ( -330.4913330509368166, -175.5095439275177398, -27.86139516340860212 ) ) ;
#42883 = DIRECTION ( 'NONE',  ( 0.000000000000000000, -0.1205366802553268363, -0.9927088740980534176 ) ) ;
#42884 = ORIENTED_EDGE ( 'NONE', *, *, #14535, .T. ) ;
#42885 = ORIENTED_EDGE ( 'NONE', *, *, #26943, .T. ) ;
#42886 = FACE_OUTER_BOUND ( 'NONE', #25095, .T. ) ;
#42887 = DIRECTION ( 'NONE',  ( -0.000000000000000000, -0.9350162426854169428, -0.3546048870425300148 ) ) ;
#42888 = ORIENTED_EDGE ( 'NONE', *, *, #44811, .T. ) ;
#42889 = CARTESIAN_POINT ( 'NONE',  ( 54.18765407974404269, -193.5000000000000000, -69.53890913632879744 ) ) ;
#42890 = AXIS2_PLACEMENT_3D ( 'NONE', #33146, #49196, #1869 ) ;
#42891 = LINE ( 'NONE', #42374, #51720 ) ;
#42892 = ORIENTED_EDGE ( 'NONE', *, *, #48821, .F. ) ;
#42893 = FACE_BOUND ( 'NONE', #149, .T. ) ;
#42894 = DIRECTION ( 'NONE',  ( -0.000000000000000000, 1.000000000000000000, -0.000000000000000000 ) ) ;
#42895 = CIRCLE ( 'NONE', #13534, 125.0000000000000000 ) ;
#42896 = ORIENTED_EDGE ( 'NONE', *, *, #4076, .T. ) ;
#42897 = DIRECTION ( 'NONE',  ( -0.000000000000000000, 1.000000000000000000, -0.000000000000000000 ) ) ;
#42898 = VERTEX_POINT ( 'NONE', #46405 ) ;
#42899 = DIRECTION ( 'NONE',  ( -0.9960498426152165630, 0.000000000000000000, -0.08879589532293852283 ) ) ;
#42900 = CARTESIAN_POINT ( 'NONE',  ( -80.17897391495031911, -177.1207230881787780, 120.9136869416132498 ) ) ;
#42901 = EDGE_LOOP ( 'NONE', ( #33049, #36462, #33648, #28065 ) ) ;
#42902 = LINE ( 'NONE', #50298, #17678 ) ;
#42903 = EDGE_CURVE ( 'NONE', #32843, #47910, #34805, .T. ) ;
#42904 = DIRECTION ( 'NONE',  ( 0.000000000000000000, 0.000000000000000000, -1.000000000000000000 ) ) ;
#42905 = CARTESIAN_POINT ( 'NONE',  ( -339.1964088526558498, -75.22798428563991990, -33.92731199008514409 ) ) ;
#42906 = EDGE_CURVE ( 'NONE', #39429, #48052, #22218, .T. ) ;
#42907 = ORIENTED_EDGE ( 'NONE', *, *, #30759, .T. ) ;
#42908 = CARTESIAN_POINT ( 'NONE',  ( 46.01898237923986557, -177.1207230881787780, -81.82363577055902226 ) ) ;
#42909 = AXIS2_PLACEMENT_3D ( 'NONE', #35551, #30326, #47147 ) ;
#42910 = DIRECTION ( 'NONE',  ( 0.000000000000000000, -0.000000000000000000, 1.000000000000000000 ) ) ;
#42911 = DIRECTION ( 'NONE',  ( 0.000000000000000000, 1.003826651431912330E-13, -1.000000000000000000 ) ) ;
#42913 = ORIENTED_EDGE ( 'NONE', *, *, #15129, .F. ) ;
#42912 = CARTESIAN_POINT ( 'NONE',  ( 1.352451982137505171, -193.5000000000000000, 113.5465278748097120 ) ) ;
#42914 = ORIENTED_EDGE ( 'NONE', *, *, #45786, .T. ) ;
#42915 = DIRECTION ( 'NONE',  ( 1.000000000000000000, 0.000000000000000000, 0.000000000000000000 ) ) ;
#42916 = EDGE_CURVE ( 'NONE', #44016, #27425, #50098, .T. ) ;
#42917 = EDGE_CURVE ( 'NONE', #45145, #12900, #34051, .T. ) ;
#42918 = CARTESIAN_POINT ( 'NONE',  ( 75.67769207106684348, -193.5000000000000000, 14.49428645563876650 ) ) ;
#42919 = ORIENTED_EDGE ( 'NONE', *, *, #44644, .T. ) ;
#42920 = ORIENTED_EDGE ( 'NONE', *, *, #2955, .T. ) ;
#42921 = EDGE_CURVE ( 'NONE', #12660, #2495, #25638, .T. ) ;
#42922 = DIRECTION ( 'NONE',  ( -0.000000000000000000, 1.000000000000000000, -0.000000000000000000 ) ) ;
#42923 = ORIENTED_EDGE ( 'NONE', *, *, #51913, .F. ) ;
#42924 = DIRECTION ( 'NONE',  ( 0.7378332790417333475, 0.000000000000000000, -0.6749830015182038956 ) ) ;
#42925 = DIRECTION ( 'NONE',  ( 0.000000000000000000, 0.000000000000000000, 1.000000000000000000 ) ) ;
#42926 = CIRCLE ( 'NONE', #17772, 125.0000000000000000 ) ;
#42927 = EDGE_CURVE ( 'NONE', #40613, #10130, #37911, .T. ) ;
#42928 = DIRECTION ( 'NONE',  ( -0.7765238627180349740, 0.000000000000000000, -0.6300878435817203194 ) ) ;
#42929 = LINE ( 'NONE', #3757, #24128 ) ;
#42930 = AXIS2_PLACEMENT_3D ( 'NONE', #24108, #36960, #949 ) ;
#42931 = ORIENTED_EDGE ( 'NONE', *, *, #2216, .T. ) ;
#42932 = ORIENTED_EDGE ( 'NONE', *, *, #17286, .T. ) ;
#42934 = EDGE_LOOP ( 'NONE', ( #40471, #16893, #360, #1922 ) ) ;
#42933 = CIRCLE ( 'NONE', #48840, 125.0000000000000000 ) ;
#42935 = DIRECTION ( 'NONE',  ( 0.000000000000000000, -0.000000000000000000, 1.000000000000000000 ) ) ;
#42936 = EDGE_CURVE ( 'NONE', #25203, #42991, #10388, .T. ) ;
#42937 = DIRECTION ( 'NONE',  ( 0.6528221181905227155, 0.000000000000000000, -0.7575112421616191360 ) ) ;
#42938 = CARTESIAN_POINT ( 'NONE',  ( -48.47912675150885065, -177.1207230881787780, 6.938893903907228378E-15 ) ) ;
#42939 = CARTESIAN_POINT ( 'NONE',  ( -336.3521761649654422, -70.03480886230919111, 25.08789112700620194 ) ) ;
#42940 = DIRECTION ( 'NONE',  ( -0.000000000000000000, 0.1205366802553337752, 0.9927088740980526405 ) ) ;
#42941 = ORIENTED_EDGE ( 'NONE', *, *, #41009, .T. ) ;
#42942 = DIRECTION ( 'NONE',  ( 1.000000000000000000, -0.000000000000000000, -0.000000000000000000 ) ) ;
#42943 = DIRECTION ( 'NONE',  ( 0.000000000000000000, 0.7485107481711069655, 0.6631226582407885317 ) ) ;
#42944 = VECTOR ( 'NONE', #13199, 1000.000000000000000 ) ;
#42945 = ORIENTED_EDGE ( 'NONE', *, *, #37824, .T. ) ;
#42946 = EDGE_LOOP ( 'NONE', ( #20935, #4231, #33999, #2463 ) ) ;
#42947 = CARTESIAN_POINT ( 'NONE',  ( 17.15229921100054611, -177.1207230881787780, -106.3838142112212921 ) ) ;
#42948 = VECTOR ( 'NONE', #2924, 1000.000000000000114 ) ;
#42949 = LINE ( 'NONE', #6710, #38194 ) ;
#42950 = DIRECTION ( 'NONE',  ( 0.000000000000000000, 0.000000000000000000, 1.000000000000000000 ) ) ;
#42951 = DIRECTION ( 'NONE',  ( 0.000000000000000000, 0.000000000000000000, -1.000000000000000000 ) ) ;
#42952 = PLANE ( 'NONE',  #37960 ) ;
#42953 = DIRECTION ( 'NONE',  ( -0.000000000000000000, -1.000000000000000000, 0.000000000000000000 ) ) ;
#42954 = ORIENTED_EDGE ( 'NONE', *, *, #11344, .T. ) ;
#42955 = LINE ( 'NONE', #6965, #2416 ) ;
#42956 = ADVANCED_FACE ( 'NONE', ( #23270 ), #3019, .T. ) ;
#42957 = VERTEX_POINT ( 'NONE', #23000 ) ;
#42958 = CARTESIAN_POINT ( 'NONE',  ( -149.9407190013152160, -175.3837268820161057, -73.01058346660458653 ) ) ;
#42959 = CARTESIAN_POINT ( 'NONE',  ( -48.47912675150885065, -175.3837268820161057, 6.938893903907228378E-15 ) ) ;
#42960 = ORIENTED_EDGE ( 'NONE', *, *, #5432, .F. ) ;
#42961 = VECTOR ( 'NONE', #36647, 1000.000000000000000 ) ;
#42962 = EDGE_CURVE ( 'NONE', #2344, #47414, #29499, .T. ) ;
#42963 = DIRECTION ( 'NONE',  ( 0.000000000000000000, -1.000000000000000000, 0.000000000000000000 ) ) ;
#42964 = EDGE_CURVE ( 'NONE', #40712, #47727, #51144, .T. ) ;
#42965 = FACE_OUTER_BOUND ( 'NONE', #38146, .T. ) ;
#42966 = DIRECTION ( 'NONE',  ( 0.000000000000000000, 0.000000000000000000, 1.000000000000000000 ) ) ;
#42967 = ADVANCED_FACE ( 'NONE', ( #40044 ), #7743, .T. ) ;
#42968 = VECTOR ( 'NONE', #9310, 1000.000000000000000 ) ;
#42969 = CARTESIAN_POINT ( 'NONE',  ( -339.1964088526558498, -63.99980407363855761, 7.728304129923844634 ) ) ;
#42970 = EDGE_CURVE ( 'NONE', #38087, #1712, #23772, .T. ) ;
#42971 = AXIS2_PLACEMENT_3D ( 'NONE', #2596, #25739, #18629 ) ;
#42972 = CARTESIAN_POINT ( 'NONE',  ( -133.1483155860611021, -183.6283474603465606, -90.59430563621275212 ) ) ;
#42973 = VERTEX_POINT ( 'NONE', #26930 ) ;
#42974 = EDGE_CURVE ( 'NONE', #3147, #3202, #31657, .T. ) ;
#42975 = DIRECTION ( 'NONE',  ( 0.000000000000000000, 0.000000000000000000, -1.000000000000000000 ) ) ;
#42977 = ORIENTED_EDGE ( 'NONE', *, *, #51082, .F. ) ;
#42976 = FACE_OUTER_BOUND ( 'NONE', #5059, .T. ) ;
#42978 = VERTEX_POINT ( 'NONE', #43219 ) ;
#42979 = DIRECTION ( 'NONE',  ( 0.3758275821142292861, 0.000000000000000000, 0.9266896074318371479 ) ) ;
#42980 = EDGE_CURVE ( 'NONE', #2935, #28959, #3499, .T. ) ;
#42981 = ORIENTED_EDGE ( 'NONE', *, *, #32111, .T. ) ;
#42982 = AXIS2_PLACEMENT_3D ( 'NONE', #46303, #25280, #45521 ) ;
#42983 = EDGE_CURVE ( 'NONE', #28863, #44261, #11414, .T. ) ;
#42984 = DIRECTION ( 'NONE',  ( 0.9027978299657416494, 0.000000000000000000, 0.4300652022765245608 ) ) ;
#42985 = AXIS2_PLACEMENT_3D ( 'NONE', #32564, #5504, #24949 ) ;
#42986 = AXIS2_PLACEMENT_3D ( 'NONE', #36608, #24514, #40272 ) ;
#42987 = ORIENTED_EDGE ( 'NONE', *, *, #29214, .T. ) ;
#42988 = EDGE_CURVE ( 'NONE', #15810, #12661, #6888, .T. ) ;
#42989 = DIRECTION ( 'NONE',  ( -0.4031234292879792847, 0.000000000000000000, 0.9151456172430153524 ) ) ;
#42990 = DIRECTION ( 'NONE',  ( 1.000000000000000000, -0.000000000000000000, 1.224646799147353207E-16 ) ) ;
#42991 = VERTEX_POINT ( 'NONE', #3795 ) ;
#42992 = DIRECTION ( 'NONE',  ( 1.000000000000000000, -0.000000000000000000, -0.000000000000000000 ) ) ;
#42993 = EDGE_CURVE ( 'NONE', #41579, #42167, #11683, .T. ) ;
#42994 = LINE ( 'NONE', #39554, #42012 ) ;
#42995 = PLANE ( 'NONE',  #3025 ) ;
#42996 = EDGE_LOOP ( 'NONE', ( #40315, #30430, #45670, #45287 ) ) ;
#42997 = EDGE_LOOP ( 'NONE', ( #26810, #31956, #39040, #18524 ) ) ;
#42998 = EDGE_CURVE ( 'NONE', #10986, #48832, #47186, .T. ) ;
#42999 = EDGE_LOOP ( 'NONE', ( #33092, #49832, #23228, #39672 ) ) ;
#43000 = LINE ( 'NONE', #30639, #21715 ) ;
#43001 = FACE_OUTER_BOUND ( 'NONE', #26713, .T. ) ;
#43002 = FACE_OUTER_BOUND ( 'NONE', #25520, .T. ) ;
#43003 = DIRECTION ( 'NONE',  ( 0.000000000000000000, -0.7485107481710934207, 0.6631226582408039638 ) ) ;
#43004 = CARTESIAN_POINT ( 'NONE',  ( -48.59739992243020623, -193.5000000000000000, -0.9929810960135115883 ) ) ;
#43005 = VECTOR ( 'NONE', #46721, 1000.000000000000114 ) ;
#43006 = VERTEX_POINT ( 'NONE', #46934 ) ;
#43007 = EDGE_CURVE ( 'NONE', #37393, #24991, #47430, .T. ) ;
#43008 = AXIS2_PLACEMENT_3D ( 'NONE', #4733, #13131, #20761 ) ;
#43009 = LINE ( 'NONE', #23038, #42514 ) ;
#43010 = VERTEX_POINT ( 'NONE', #7495 ) ;
#43012 = ORIENTED_EDGE ( 'NONE', *, *, #28548, .T. ) ;
#43011 = DIRECTION ( 'NONE',  ( 0.000000000000000000, -1.000000000000000000, 0.000000000000000000 ) ) ;
#43013 = ORIENTED_EDGE ( 'NONE', *, *, #30832, .F. ) ;
#43014 = DIRECTION ( 'NONE',  ( 1.000000000000000000, -0.000000000000000000, -0.000000000000000000 ) ) ;
#43015 = DIRECTION ( 'NONE',  ( -0.000000000000000000, 0.000000000000000000, -1.000000000000000000 ) ) ;
#43016 = CARTESIAN_POINT ( 'NONE',  ( 23.33927677392131628, -177.1207230881787780, -102.3089288139528747 ) ) ;
#43017 = LINE ( 'NONE', #7026, #26770 ) ;
#43018 = EDGE_LOOP ( 'NONE', ( #31681, #11381, #17274, #16232 ) ) ;
#43019 = DIRECTION ( 'NONE',  ( 0.000000000000000000, -1.000000000000000000, 0.000000000000000000 ) ) ;
#43020 = ORIENTED_EDGE ( 'NONE', *, *, #30379, .F. ) ;
#43021 = CIRCLE ( 'NONE', #43058, 125.0000000000000000 ) ;
#43022 = VECTOR ( 'NONE', #10128, 1000.000000000000000 ) ;
#43023 = EDGE_LOOP ( 'NONE', ( #44296, #24270, #24685, #10057 ) ) ;
#43024 = CARTESIAN_POINT ( 'NONE',  ( 65.79610465833508215, -183.6283474603465606, -50.65739320401927870 ) ) ;
#43025 = CIRCLE ( 'NONE', #20360, 125.0000000000000000 ) ;
#43027 = VECTOR ( 'NONE', #33265, 1000.000000000000000 ) ;
#43026 = DIRECTION ( 'NONE',  ( -0.4566292373937200777, 0.000000000000000000, 0.8896570909947436601 ) ) ;
#43028 = CARTESIAN_POINT ( 'NONE',  ( -339.1964088526558498, -122.9999999999993605, 59.99791663049642665 ) ) ;
#43029 = CARTESIAN_POINT ( 'NONE',  ( -128.7986236165182277, -193.5000000000000000, 94.47107458416954273 ) ) ;
#43030 = EDGE_LOOP ( 'NONE', ( #41739, #26632, #27445, #45886 ) ) ;
#43031 = CARTESIAN_POINT ( 'NONE',  ( 43.86477233319988756, -175.3837268820161057, -84.24728067915975771 ) ) ;
#43032 = FACE_OUTER_BOUND ( 'NONE', #8251, .T. ) ;
#43033 = EDGE_CURVE ( 'NONE', #13545, #47870, #15903, .T. ) ;
#43034 = ADVANCED_FACE ( 'NONE', ( #23516 ), #39529, .F. ) ;
#43035 = DIRECTION ( 'NONE',  ( 0.000000000000000000, 0.000000000000000000, 1.000000000000000000 ) ) ;
#43036 = CARTESIAN_POINT ( 'NONE',  ( -0.3054481938615516423, -177.1207230881787780, 115.3442529744090450 ) ) ;
#43037 = AXIS2_PLACEMENT_3D ( 'NONE', #31213, #3362, #31468 ) ;
#43038 = ORIENTED_EDGE ( 'NONE', *, *, #27828, .T. ) ;
#43039 = DIRECTION ( 'NONE',  ( 0.000000000000000000, -1.000000000000000000, 0.000000000000000000 ) ) ;
#43040 = DIRECTION ( 'NONE',  ( -0.000000000000000000, -1.000000000000000000, -0.000000000000000000 ) ) ;
#43041 = EDGE_CURVE ( 'NONE', #30065, #40321, #35585, .T. ) ;
#43042 = EDGE_CURVE ( 'NONE', #21936, #44616, #2679, .T. ) ;
#43043 = DIRECTION ( 'NONE',  ( 0.2920567706369628924, 0.000000000000000000, 0.9564009842765264224 ) ) ;
#43044 = VERTEX_POINT ( 'NONE', #16154 ) ;
#43045 = DIRECTION ( 'NONE',  ( -0.000000000000000000, 1.000000000000000000, -0.000000000000000000 ) ) ;
#43046 = VECTOR ( 'NONE', #24350, 1000.000000000000000 ) ;
#43047 = PLANE ( 'NONE',  #44592 ) ;
#43048 = ORIENTED_EDGE ( 'NONE', *, *, #1081, .F. ) ;
#43049 = CARTESIAN_POINT ( 'NONE',  ( 76.43863189440992301, -193.5000000000000000, -4.533605064403313456 ) ) ;
#43050 = EDGE_LOOP ( 'NONE', ( #15327, #34291, #13681, #2738 ) ) ;
#43051 = AXIS2_PLACEMENT_3D ( 'NONE', #25867, #5388, #21404 ) ;
#43052 = LINE ( 'NONE', #7060, #2453 ) ;
#43053 = EDGE_CURVE ( 'NONE', #19112, #12481, #10913, .T. ) ;
#43054 = FACE_BOUND ( 'NONE', #16535, .T. ) ;
#43055 = DIRECTION ( 'NONE',  ( 0.000000000000000000, -0.000000000000000000, 1.000000000000000000 ) ) ;
#43057 = VECTOR ( 'NONE', #7375, 1000.000000000000000 ) ;
#43056 = CARTESIAN_POINT ( 'NONE',  ( -108.6269575285487434, -177.1207230881787780, -108.4360005853207269 ) ) ;
#43058 = AXIS2_PLACEMENT_3D ( 'NONE', #13132, #29671, #21280 ) ;
#43059 = VERTEX_POINT ( 'NONE', #4317 ) ;
#43060 = EDGE_CURVE ( 'NONE', #21927, #21227, #37408, .T. ) ;
#43061 = ORIENTED_EDGE ( 'NONE', *, *, #19778, .F. ) ;
#43062 = CARTESIAN_POINT ( 'NONE',  ( -170.0502155641509034, -183.6283474603465606, -29.07697310430886262 ) ) ;
#43063 = CIRCLE ( 'NONE', #4468, 60.00000000000000000 ) ;
#43064 = EDGE_LOOP ( 'NONE', ( #4520, #43710, #2687, #20590 ) ) ;
#43065 = DIRECTION ( 'NONE',  ( 0.000000000000000000, 0.000000000000000000, -1.000000000000000000 ) ) ;
#43066 = VECTOR ( 'NONE', #40133, 1000.000000000000114 ) ;
#43067 = PLANE ( 'NONE',  #44363 ) ;
#43068 = CARTESIAN_POINT ( 'NONE',  ( -142.9772358822569913, -177.1207230881787780, 81.82363577055970438 ) ) ;
#43069 = ORIENTED_EDGE ( 'NONE', *, *, #13139, .F. ) ;
#43072 = ORIENTED_EDGE ( 'NONE', *, *, #50844, .F. ) ;
#43071 = LINE ( 'NONE', #19666, #1252 ) ;
#43070 = DIRECTION ( 'NONE',  ( 0.7765238627180437447, 0.000000000000000000, -0.6300878435817094392 ) ) ;
#43073 = DIRECTION ( 'NONE',  ( 0.000000000000000000, -1.000000000000000000, 0.000000000000000000 ) ) ;
#43074 = ORIENTED_EDGE ( 'NONE', *, *, #45099, .F. ) ;
#43075 = CARTESIAN_POINT ( 'NONE',  ( -48.47912675150885065, -189.7472609257535510, 6.938893903907228378E-15 ) ) ;
#43076 = VECTOR ( 'NONE', #33663, 1000.000000000000000 ) ;
#43077 = ORIENTED_EDGE ( 'NONE', *, *, #2955, .F. ) ;
#43078 = PLANE ( 'NONE',  #9948 ) ;
#43079 = ORIENTED_EDGE ( 'NONE', *, *, #35188, .F. ) ;
#43081 = CARTESIAN_POINT ( 'NONE',  ( -116.2964108826154330, -193.5000000000000000, -105.0038855142073260 ) ) ;
#43080 = PLANE ( 'NONE',  #6503 ) ;
#43082 = VERTEX_POINT ( 'NONE', #28222 ) ;
#43083 = VECTOR ( 'NONE', #33351, 1000.000000000000000 ) ;
#43084 = DIRECTION ( 'NONE',  ( -0.2920567706369833760, 0.000000000000000000, 0.9564009842765202052 ) ) ;
#43085 = EDGE_LOOP ( 'NONE', ( #21399, #17881, #38188, #33218 ) ) ;
#43086 = CARTESIAN_POINT ( 'NONE',  ( -305.0000000000000568, -174.3267994849386184, -31.88473700876087591 ) ) ;
#43087 = FACE_OUTER_BOUND ( 'NONE', #21948, .T. ) ;
#43088 = VERTEX_POINT ( 'NONE', #8769 ) ;
#43089 = PLANE ( 'NONE',  #23833 ) ;
#43090 = DIRECTION ( 'NONE',  ( -1.000000000000000000, 0.000000000000000000, -0.000000000000000000 ) ) ;
#43091 = PLANE ( 'NONE',  #47567 ) ;
#43092 = DIRECTION ( 'NONE',  ( -1.000000000000000000, -0.000000000000000000, 0.000000000000000000 ) ) ;
#43093 = ORIENTED_EDGE ( 'NONE', *, *, #10421, .F. ) ;
#43094 = EDGE_CURVE ( 'NONE', #19724, #13250, #24542, .T. ) ;
#43095 = ADVANCED_FACE ( 'NONE', ( #36369 ), #12705, .F. ) ;
#43096 = AXIS2_PLACEMENT_3D ( 'NONE', #22406, #45807, #38676 ) ;
#43097 = DIRECTION ( 'NONE',  ( -0.000000000000000000, 0.9709418174260553425, 0.2393156642875449158 ) ) ;
#43098 = PLANE ( 'NONE',  #7996 ) ;
#43099 = CARTESIAN_POINT ( 'NONE',  ( 75.10200014432449223, -189.7472609257535510, 10.18383939837613639 ) ) ;
#43100 = ORIENTED_EDGE ( 'NONE', *, *, #51103, .F. ) ;
#43101 = VECTOR ( 'NONE', #44331, 1000.000000000000000 ) ;
#43102 = DIRECTION ( 'NONE',  ( -0.9785564922995017012, 0.000000000000000000, -0.2059786187411094538 ) ) ;
#43103 = DIRECTION ( 'NONE',  ( 0.000000000000000000, 0.000000000000000000, 1.000000000000000000 ) ) ;
#43104 = LINE ( 'NONE', #1684, #15706 ) ;
#43105 = DIRECTION ( 'NONE',  ( 1.000000000000000000, -0.000000000000000000, -0.000000000000000000 ) ) ;
#43106 = DIRECTION ( 'NONE',  ( 0.000000000000000000, 0.000000000000000000, -1.000000000000000000 ) ) ;
#43107 = ORIENTED_EDGE ( 'NONE', *, *, #13446, .F. ) ;
#43108 = FACE_OUTER_BOUND ( 'NONE', #31832, .T. ) ;
#43109 = DIRECTION ( 'NONE',  ( 0.000000000000000000, -1.000000000000000000, 0.000000000000000000 ) ) ;
#43110 = FACE_OUTER_BOUND ( 'NONE', #28474, .T. ) ;
#43111 = EDGE_CURVE ( 'NONE', #13947, #42649, #33632, .T. ) ;
#43112 = CYLINDRICAL_SURFACE ( 'NONE', #27058, 20.00000000000001776 ) ;
#43113 = PLANE ( 'NONE',  #37126 ) ;
#43114 = VECTOR ( 'NONE', #24360, 1000.000000000000000 ) ;
#43115 = ORIENTED_EDGE ( 'NONE', *, *, #9837, .F. ) ;
#43116 = DIRECTION ( 'NONE',  ( 0.000000000000000000, -0.000000000000000000, 1.000000000000000000 ) ) ;
#43117 = AXIS2_PLACEMENT_3D ( 'NONE', #25143, #49838, #1483 ) ;
#43118 = ADVANCED_FACE ( 'NONE', ( #21121 ), #24808, .F. ) ;
#43119 = EDGE_LOOP ( 'NONE', ( #48055, #20312, #17765, #16622 ) ) ;
#43120 = VERTEX_POINT ( 'NONE', #32691 ) ;
#43121 = ORIENTED_EDGE ( 'NONE', *, *, #36139, .F. ) ;
#43122 = LINE ( 'NONE', #34715, #16644 ) ;
#43123 = EDGE_CURVE ( 'NONE', #18433, #43853, #44550, .T. ) ;
#43124 = DIRECTION ( 'NONE',  ( -0.000000000000000000, 1.000000000000000000, -0.000000000000000000 ) ) ;
#43126 = ORIENTED_EDGE ( 'NONE', *, *, #35796, .F. ) ;
#43125 = CIRCLE ( 'NONE', #23847, 125.0000000000000000 ) ;
#43127 = DIRECTION ( 'NONE',  ( 0.000000000000000000, 0.000000000000000000, 1.000000000000000000 ) ) ;
#43128 = DIRECTION ( 'NONE',  ( 0.000000000000000000, 0.000000000000000000, 1.000000000000000000 ) ) ;
#43131 = ORIENTED_EDGE ( 'NONE', *, *, #323, .F. ) ;
#43130 = CARTESIAN_POINT ( 'NONE',  ( 75.60865171534658202, -193.5000000000000000, -15.07392567185468124 ) ) ;
#43129 = LINE ( 'NONE', #15039, #17425 ) ;
#43132 = FACE_OUTER_BOUND ( 'NONE', #7432, .T. ) ;
#43133 = ORIENTED_EDGE ( 'NONE', *, *, #21503, .F. ) ;
#43134 = CARTESIAN_POINT ( 'NONE',  ( -339.1964088526558498, -162.2499814621209850, 44.49369547121574442 ) ) ;
#43135 = VERTEX_POINT ( 'NONE', #40824 ) ;
#43136 = CARTESIAN_POINT ( 'NONE',  ( -332.3517673607765914, -178.0871407151310279, 22.44790492310219676 ) ) ;
#43137 = CARTESIAN_POINT ( 'NONE',  ( -332.3517673607765914, -106.8245764869328980, 56.65561927337994064 ) ) ;
#43139 = PLANE ( 'NONE',  #39915 ) ;
#43138 = DIRECTION ( 'NONE',  ( 0.000000000000000000, 0.000000000000000000, 1.000000000000000000 ) ) ;
#43140 = ORIENTED_EDGE ( 'NONE', *, *, #21738, .F. ) ;
#43141 = ADVANCED_FACE ( 'NONE', ( #40558 ), #5366, .T. ) ;
#43142 = CYLINDRICAL_SURFACE ( 'NONE', #11379, 124.9999999999999858 ) ;
#43143 = ORIENTED_EDGE ( 'NONE', *, *, #43212, .T. ) ;
#43144 = DIRECTION ( 'NONE',  ( 0.000000000000000000, -0.9927088740980526405, 0.1205366802553337890 ) ) ;
#43145 = FACE_OUTER_BOUND ( 'NONE', #11989, .T. ) ;
#43146 = VERTEX_POINT ( 'NONE', #48215 ) ;
#43147 = FACE_OUTER_BOUND ( 'NONE', #9841, .T. ) ;
#43148 = AXIS2_PLACEMENT_3D ( 'NONE', #16662, #19798, #8745 ) ;
#43149 = DIRECTION ( 'NONE',  ( -0.000000000000000000, 1.000000000000000000, -0.000000000000000000 ) ) ;
#43150 = AXIS2_PLACEMENT_3D ( 'NONE', #25455, #45189, #21776 ) ;
#43151 = ORIENTED_EDGE ( 'NONE', *, *, #4059, .F. ) ;
#43152 = ADVANCED_FACE ( 'NONE', ( #642 ), #887, .T. ) ;
#43153 = FACE_BOUND ( 'NONE', #32796, .T. ) ;
#43155 = AXIS2_PLACEMENT_3D ( 'NONE', #37683, #25333, #32942 ) ;
#43154 = CARTESIAN_POINT ( 'NONE',  ( 74.48795740376235130, -183.6283474603465606, -15.97798378892165871 ) ) ;
#43156 = VERTEX_POINT ( 'NONE', #8259 ) ;
#43157 = PLANE ( 'NONE',  #51808 ) ;
#43158 = ORIENTED_EDGE ( 'NONE', *, *, #4818, .T. ) ;
#43159 = EDGE_CURVE ( 'NONE', #16186, #42609, #5111, .T. ) ;
#43160 = LINE ( 'NONE', #3231, #30687 ) ;
#43161 = CARTESIAN_POINT ( 'NONE',  ( -336.3521761649654422, -73.44864141332200802, 31.34948880313848107 ) ) ;
#43162 = VERTEX_POINT ( 'NONE', #32431 ) ;
#43163 = DIRECTION ( 'NONE',  ( -0.2059786187411094538, 0.000000000000000000, 0.9785564922995017012 ) ) ;
#43164 = LINE ( 'NONE', #31861, #44056 ) ;
#43165 = CARTESIAN_POINT ( 'NONE',  ( -28.74596282265200387, -183.6283474603465606, 123.4325817657431372 ) ) ;
#43166 = AXIS2_PLACEMENT_3D ( 'NONE', #34588, #30646, #18061 ) ;
#43167 = CARTESIAN_POINT ( 'NONE',  ( -116.2964108826154188, -177.1207230881787780, -105.0038855142073402 ) ) ;
#43168 = CARTESIAN_POINT ( 'NONE',  ( -305.0000000000000568, -150.9396941197150852, 53.35787839313398706 ) ) ;
#43169 = DIRECTION ( 'NONE',  ( -0.000000000000000000, 1.000000000000000000, -0.000000000000000000 ) ) ;
#43170 = EDGE_CURVE ( 'NONE', #4741, #41311, #33206, .T. ) ;
#43171 = DIRECTION ( 'NONE',  ( 1.043714542225393223E-14, 0.6631226582407863113, -0.7485107481711089639 ) ) ;
#43173 = ORIENTED_EDGE ( 'NONE', *, *, #32401, .T. ) ;
#43172 = CARTESIAN_POINT ( 'NONE',  ( 41.40822382563629134, -183.6283474603465606, 85.41934182508082074 ) ) ;
#43174 = ORIENTED_EDGE ( 'NONE', *, *, #49685, .F. ) ;
#43175 = LINE ( 'NONE', #26375, #23247 ) ;
#43176 = DIRECTION ( 'NONE',  ( 0.000000000000000000, 0.000000000000000000, 1.000000000000000000 ) ) ;
#43177 = EDGE_LOOP ( 'NONE', ( #37072, #5262, #4363, #18401 ) ) ;
#43178 = ORIENTED_EDGE ( 'NONE', *, *, #51375, .T. ) ;
#43179 = CARTESIAN_POINT ( 'NONE',  ( 75.60865171534658202, -177.1207230881787780, -15.07392567185468124 ) ) ;
#43180 = ORIENTED_EDGE ( 'NONE', *, *, #17373, .F. ) ;
#43181 = CARTESIAN_POINT ( 'NONE',  ( -105.2524431885210845, -175.3837268820161057, 110.2396968984195382 ) ) ;
#43182 = DIRECTION ( 'NONE',  ( 1.000000000000000000, 0.000000000000000000, 0.000000000000000000 ) ) ;
#43183 = AXIS2_PLACEMENT_3D ( 'NONE', #5025, #25245, #32856 ) ;
#43184 = AXIS2_PLACEMENT_3D ( 'NONE', #21260, #49387, #4983 ) ;
#43185 = DIRECTION ( 'NONE',  ( 0.9027978299657387629, 0.000000000000000000, 0.4300652022765304450 ) ) ;
#43186 = FACE_OUTER_BOUND ( 'NONE', #21881, .T. ) ;
#43187 = ORIENTED_EDGE ( 'NONE', *, *, #30137, .T. ) ;
#43188 = VERTEX_POINT ( 'NONE', #45060 ) ;
#43189 = AXIS2_PLACEMENT_3D ( 'NONE', #45577, #9314, #40829 ) ;
#43190 = ORIENTED_EDGE ( 'NONE', *, *, #50449, .F. ) ;
#43191 = CARTESIAN_POINT ( 'NONE',  ( -48.47912675150885065, -175.3837268820161057, 6.938893903907228378E-15 ) ) ;
#43192 = DIRECTION ( 'NONE',  ( 0.5586467658036476935, 0.000000000000000000, 0.8294056854502049880 ) ) ;
#43193 = CARTESIAN_POINT ( 'NONE',  ( -332.3517673607765914, -76.88706545914891421, 37.77875505479673279 ) ) ;
#43194 = AXIS2_PLACEMENT_3D ( 'NONE', #10759, #42811, #10490 ) ;
#43195 = DIRECTION ( 'NONE',  ( -0.000000000000000000, 1.000000000000000000, -0.000000000000000000 ) ) ;
#43196 = PLANE ( 'NONE',  #35661 ) ;
#43197 = VERTEX_POINT ( 'NONE', #9050 ) ;
#43198 = EDGE_CURVE ( 'NONE', #37735, #20132, #8510, .T. ) ;
#43199 = PRODUCT_DEFINITION_CONTEXT ( 'detailed design', #10557, 'design' ) ;
#43200 = DIRECTION ( 'NONE',  ( 0.000000000000000000, 0.000000000000000000, 1.000000000000000000 ) ) ;
#43201 = CARTESIAN_POINT ( 'NONE',  ( -4.176930889631405464, -189.7472609257535510, 116.8859077982279615 ) ) ;
#43202 = ORIENTED_EDGE ( 'NONE', *, *, #30844, .F. ) ;
#43203 = VERTEX_POINT ( 'NONE', #41096 ) ;
#43204 = DIRECTION ( 'NONE',  ( 0.000000000000000000, -2.914335439641035919E-13, -1.000000000000000000 ) ) ;
#43205 = DIRECTION ( 'NONE',  ( 0.000000000000000000, 0.000000000000000000, 1.000000000000000000 ) ) ;
#43206 = CARTESIAN_POINT ( 'NONE',  ( -339.1964088526558498, -156.6043281241909426, 48.84008046109164525 ) ) ;
#43207 = EDGE_LOOP ( 'NONE', ( #39660, #40805, #24654, #22727 ) ) ;
#43208 = LINE ( 'NONE', #23761, #8086 ) ;
#43209 = DIRECTION ( 'NONE',  ( -1.000000000000000000, 8.589602288500749505E-15, -5.928974370889027093E-15 ) ) ;
#43210 = CARTESIAN_POINT ( 'NONE',  ( -48.41988612361514299, -177.1207230881787780, -0.9982437317643144681 ) ) ;
#43211 = ORIENTED_EDGE ( 'NONE', *, *, #7616, .F. ) ;
#43212 = EDGE_CURVE ( 'NONE', #47366, #8754, #37145, .T. ) ;
#43213 = CARTESIAN_POINT ( 'NONE',  ( -332.3517673607765914, -87.28260048324004572, 47.83617848703421771 ) ) ;
#43214 = EDGE_CURVE ( 'NONE', #50151, #9197, #29269, .T. ) ;
#43215 = ORIENTED_EDGE ( 'NONE', *, *, #5529, .F. ) ;
#43216 = DIRECTION ( 'NONE',  ( 0.000000000000000000, 1.000000000000000000, -0.000000000000000000 ) ) ;
#43217 = EDGE_CURVE ( 'NONE', #650, #50927, #44670, .T. ) ;
#43218 = VECTOR ( 'NONE', #49888, 1000.000000000000000 ) ;
#43219 = CARTESIAN_POINT ( 'NONE',  ( 45.36094686508022988, -177.1207230881787780, -82.57748230379236531 ) ) ;
#43220 = ORIENTED_EDGE ( 'NONE', *, *, #12168, .T. ) ;
#43221 = CIRCLE ( 'NONE', #23086, 124.9999999999999858 ) ;
#43222 = VECTOR ( 'NONE', #50294, 1000.000000000000000 ) ;
#43223 = DIRECTION ( 'NONE',  ( 0.000000000000000000, 0.000000000000000000, 1.000000000000000000 ) ) ;
#43224 = CARTESIAN_POINT ( 'NONE',  ( -48.47912675150885065, -175.3837268820161057, 6.938893903907228378E-15 ) ) ;
#43225 = CARTESIAN_POINT ( 'NONE',  ( 64.29733702426837283, -175.3837268820161057, 53.91167979418564471 ) ) ;
#43226 = DIRECTION ( 'NONE',  ( -0.000000000000000000, 1.000000000000000000, -0.000000000000000000 ) ) ;
#43227 = CIRCLE ( 'NONE', #30612, 4.999999999999997335 ) ;
#43228 = PLANE ( 'NONE',  #42071 ) ;
#43229 = ORIENTED_EDGE ( 'NONE', *, *, #23287, .T. ) ;
#43230 = AXIS2_PLACEMENT_3D ( 'NONE', #20385, #4117, #24335 ) ;
#43231 = DIRECTION ( 'NONE',  ( 1.000000000000000000, 0.000000000000000000, 0.000000000000000000 ) ) ;
#43233 = ORIENTED_EDGE ( 'NONE', *, *, #26186, .F. ) ;
#43232 = DIRECTION ( 'NONE',  ( -0.000000000000000000, 0.000000000000000000, -1.000000000000000000 ) ) ;
#43234 = AXIS2_PLACEMENT_3D ( 'NONE', #31612, #47665, #7459 ) ;
#43235 = EDGE_LOOP ( 'NONE', ( #10401, #44090, #21572, #34366 ) ) ;
#43236 = DIRECTION ( 'NONE',  ( 0.000000000000000000, -0.8660254037844378194, -0.5000000000000012212 ) ) ;
#43237 = VECTOR ( 'NONE', #27, 1000.000000000000000 ) ;
#43238 = ORIENTED_EDGE ( 'NONE', *, *, #11476, .T. ) ;
#43239 = AXIS2_PLACEMENT_3D ( 'NONE', #3126, #39114, #3379 ) ;
#43240 = CARTESIAN_POINT ( 'NONE',  ( -260.0000000000000000, -153.5000000000000284, 60.00000000000002132 ) ) ;
#43241 = ORIENTED_EDGE ( 'NONE', *, *, #2546, .T. ) ;
#43242 = LINE ( 'NONE', #19850, #51143 ) ;
#43243 = CARTESIAN_POINT ( 'NONE',  ( -142.2007120195389405, -177.1207230881787780, 81.19354792697799894 ) ) ;
#43244 = VERTEX_POINT ( 'NONE', #40301 ) ;
#43245 = CARTESIAN_POINT ( 'NONE',  ( -280.0000000000000000, -63.50000000000000000, 60.00000000000000711 ) ) ;
#43246 = CARTESIAN_POINT ( 'NONE',  ( -59.28786813212838069, -193.5000000000000000, 124.5318076226587323 ) ) ;
#43247 = DIRECTION ( 'NONE',  ( 0.000000000000000000, -0.000000000000000000, 1.000000000000000000 ) ) ;
#43248 = ORIENTED_EDGE ( 'NONE', *, *, #12627, .T. ) ;
#43249 = VERTEX_POINT ( 'NONE', #6406 ) ;
#43250 = ORIENTED_EDGE ( 'NONE', *, *, #50348, .T. ) ;
#43251 = DIRECTION ( 'NONE',  ( 1.000000000000000000, -0.000000000000000000, -0.000000000000000000 ) ) ;
#43252 = FACE_OUTER_BOUND ( 'NONE', #6708, .T. ) ;
#43253 = AXIS2_PLACEMENT_3D ( 'NONE', #3226, #51317, #35782 ) ;
#43254 = VECTOR ( 'NONE', #15889, 1000.000000000000000 ) ;
#43255 = CARTESIAN_POINT ( 'NONE',  ( -332.3517673607765914, -97.52665284734005979, -53.00046796564681983 ) ) ;
#43256 = CARTESIAN_POINT ( 'NONE',  ( -48.77118352214583297, -177.1207230881787780, 0.9564009842765270886 ) ) ;
#43257 = ORIENTED_EDGE ( 'NONE', *, *, #1563, .F. ) ;
#43258 = CIRCLE ( 'NONE', #44127, 60.00000000000000000 ) ;
#43259 = EDGE_CURVE ( 'NONE', #15531, #30167, #24504, .T. ) ;
#43260 = EDGE_CURVE ( 'NONE', #41322, #27872, #37679, .T. ) ;
#43261 = EDGE_CURVE ( 'NONE', #32390, #37883, #25851, .T. ) ;
#43262 = EDGE_CURVE ( 'NONE', #40095, #23489, #49590, .T. ) ;
#43263 = LINE ( 'NONE', #23554, #17368 ) ;
#43264 = VERTEX_POINT ( 'NONE', #22430 ) ;
#43266 = EDGE_LOOP ( 'NONE', ( #48641, #50064, #36850, #17991 ) ) ;
#43265 = CARTESIAN_POINT ( 'NONE',  ( -105.7090724259148118, -175.3837268820161057, 111.1293539894142839 ) ) ;
#43267 = EDGE_LOOP ( 'NONE', ( #42122, #7733, #7218, #8158 ) ) ;
#43268 = EDGE_CURVE ( 'NONE', #42496, #36635, #30049, .T. ) ;
#43269 = LINE ( 'NONE', #39059, #13217 ) ;
#43270 = AXIS2_PLACEMENT_3D ( 'NONE', #38287, #6513, #7279 ) ;
#43271 = EDGE_CURVE ( 'NONE', #34582, #4879, #42653, .T. ) ;
#43272 = LINE ( 'NONE', #39061, #1453 ) ;
#43273 = VECTOR ( 'NONE', #5433, 1000.000000000000000 ) ;
#43274 = LINE ( 'NONE', #7286, #47319 ) ;
#43275 = DIRECTION ( 'NONE',  ( -0.7765238627180393038, 0.000000000000000000, -0.6300878435817147682 ) ) ;
#43276 = ORIENTED_EDGE ( 'NONE', *, *, #31324, .F. ) ;
#43277 = EDGE_CURVE ( 'NONE', #7756, #51755, #17709, .T. ) ;
#43278 = CARTESIAN_POINT ( 'NONE',  ( 0.000000000000000000, -53.50000000000000000, 0.000000000000000000 ) ) ;
#43279 = AXIS2_PLACEMENT_3D ( 'NONE', #9160, #36751, #40408 ) ;
#43280 = ORIENTED_EDGE ( 'NONE', *, *, #12505, .F. ) ;
#43281 = EDGE_CURVE ( 'NONE', #5750, #14193, #10334, .T. ) ;
#43282 = AXIS2_PLACEMENT_3D ( 'NONE', #29623, #45672, #9662 ) ;
#43283 = EDGE_CURVE ( 'NONE', #32626, #30858, #6664, .T. ) ;
#43284 = EDGE_LOOP ( 'NONE', ( #1056, #45394, #20052, #11208 ) ) ;
#43285 = DIRECTION ( 'NONE',  ( 1.000000000000000000, 0.000000000000000000, -0.000000000000000000 ) ) ;
#43286 = CARTESIAN_POINT ( 'NONE',  ( -340.0000000000000568, -123.5000000000000142, 60.00000000000000000 ) ) ;
#43287 = EDGE_CURVE ( 'NONE', #29932, #13886, #24399, .T. ) ;
#43288 = CARTESIAN_POINT ( 'NONE',  ( -336.3521761649654422, -78.25545813661345562, 37.90245108779119931 ) ) ;
#43289 = DIRECTION ( 'NONE',  ( -0.000000000000000000, 0.000000000000000000, -1.000000000000000000 ) ) ;
#43290 = LINE ( 'NONE', #44064, #2936 ) ;
#43291 = ADVANCED_FACE ( 'NONE', ( #33983 ), #10081, .F. ) ;
#43292 = FACE_OUTER_BOUND ( 'NONE', #39802, .T. ) ;
#43293 = DIRECTION ( 'NONE',  ( -0.000000000000000000, 1.000000000000000000, -0.000000000000000000 ) ) ;
#43294 = ORIENTED_EDGE ( 'NONE', *, *, #24366, .T. ) ;
#43295 = DIRECTION ( 'NONE',  ( -0.000000000000000000, 1.000000000000000000, -0.000000000000000000 ) ) ;
#43296 = CARTESIAN_POINT ( 'NONE',  ( -109.9568094315246185, -183.6283474603465606, -108.8370090194290754 ) ) ;
#43297 = FACE_BOUND ( 'NONE', #46020, .T. ) ;
#43298 = ORIENTED_EDGE ( 'NONE', *, *, #23854, .T. ) ;
#43299 = VECTOR ( 'NONE', #21265, 1000.000000000000114 ) ;
#43300 = CARTESIAN_POINT ( 'NONE',  ( -336.3521761649654422, -133.2247606357419443, -58.25253621232173629 ) ) ;
#43301 = VECTOR ( 'NONE', #15500, 1000.000000000000000 ) ;
#43302 = CIRCLE ( 'NONE', #1364, 125.0000000000000000 ) ;
#43303 = LINE ( 'NONE', #22821, #48808 ) ;
#43304 = ORIENTED_EDGE ( 'NONE', *, *, #6311, .T. ) ;
#43305 = DIRECTION ( 'NONE',  ( -0.000000000000000000, 0.2393156642875448881, -0.9709418174260553425 ) ) ;
#43306 = ORIENTED_EDGE ( 'NONE', *, *, #11834, .F. ) ;
#43307 = ADVANCED_FACE ( 'NONE', ( #1679 ), #18482, .T. ) ;
#43308 = DIRECTION ( 'NONE',  ( 0.000000000000000000, 1.000000000000000000, 0.000000000000000000 ) ) ;
#43309 = FACE_BOUND ( 'NONE', #44554, .T. ) ;
#43310 = VECTOR ( 'NONE', #20925, 1000.000000000000000 ) ;
#43312 = VERTEX_POINT ( 'NONE', #26097 ) ;
#43311 = LINE ( 'NONE', #39365, #27068 ) ;
#43313 = VECTOR ( 'NONE', #6410, 1000.000000000000114 ) ;
#43314 = AXIS2_PLACEMENT_3D ( 'NONE', #42825, #49948, #33651 ) ;
#43315 = DIRECTION ( 'NONE',  ( 1.000000000000000000, -4.051632851310597467E-17, 7.719741424018539620E-17 ) ) ;
#43316 = VERTEX_POINT ( 'NONE', #13764 ) ;
#43317 = ORIENTED_EDGE ( 'NONE', *, *, #6639, .F. ) ;
#43318 = AXIS2_PLACEMENT_3D ( 'NONE', #10117, #26134, #42164 ) ;
#43319 = EDGE_CURVE ( 'NONE', #25483, #23608, #14028, .T. ) ;
#43320 = DIRECTION ( 'NONE',  ( 0.000000000000000000, 1.000000000000000000, 0.000000000000000000 ) ) ;
#43321 = VERTEX_POINT ( 'NONE', #42387 ) ;
#43322 = DIRECTION ( 'NONE',  ( 0.3202698538628416247, 0.000000000000000000, -0.9473263538541900619 ) ) ;
#43323 = EDGE_CURVE ( 'NONE', #4472, #26301, #22165, .T. ) ;
#43324 = ADVANCED_FACE ( 'NONE', ( #29775 ), #49524, .T. ) ;
#43325 = EDGE_CURVE ( 'NONE', #46128, #2222, #30301, .T. ) ;
#43326 = ADVANCED_FACE ( 'NONE', ( #33732 ), #9822, .T. ) ;
#43327 = ADVANCED_FACE ( 'NONE', ( #51571 ), #10854, .F. ) ;
#43328 = LINE ( 'NONE', #43833, #4108 ) ;
#43329 = DIRECTION ( 'NONE',  ( 0.000000000000000000, 0.000000000000000000, -1.000000000000000000 ) ) ;
#43330 = EDGE_LOOP ( 'NONE', ( #36934, #26084, #11715, #17540 ) ) ;
#43333 = VERTEX_POINT ( 'NONE', #14808 ) ;
#43332 = CARTESIAN_POINT ( 'NONE',  ( -48.47912675150885065, -175.3837268820161057, 6.938893903907228378E-15 ) ) ;
#43331 = CARTESIAN_POINT ( 'NONE',  ( -305.0000000000000568, -175.8491356171901145, 29.31839013542587935 ) ) ;
#43334 = AXIS2_PLACEMENT_3D ( 'NONE', #51712, #44070, #39081 ) ;
#43335 = VECTOR ( 'NONE', #37792, 1000.000000000000000 ) ;
#43336 = EDGE_CURVE ( 'NONE', #6145, #51787, #19504, .T. ) ;
#43337 = EDGE_CURVE ( 'NONE', #31562, #22071, #29539, .T. ) ;
#43338 = CARTESIAN_POINT ( 'NONE',  ( -77.67449977936063021, -193.5000000000000000, -121.5427093402339267 ) ) ;
#43339 = EDGE_LOOP ( 'NONE', ( #16006, #11249, #9459, #1676 ) ) ;
#43340 = FACE_OUTER_BOUND ( 'NONE', #23491, .T. ) ;
#43341 = ORIENTED_EDGE ( 'NONE', *, *, #51415, .T. ) ;
#43342 = AXIS2_PLACEMENT_3D ( 'NONE', #36833, #29450, #10023 ) ;
#43343 = CARTESIAN_POINT ( 'NONE',  ( 76.37123734610607073, -193.5000000000000000, 6.114457023561876703 ) ) ;
#43344 = ORIENTED_EDGE ( 'NONE', *, *, #15048, .T. ) ;
#43345 = EDGE_CURVE ( 'NONE', #34863, #12900, #36249, .T. ) ;
#43347 = LINE ( 'NONE', #39636, #30847 ) ;
#43346 = DIRECTION ( 'NONE',  ( -0.000000000000000000, 1.000000000000000000, -0.000000000000000000 ) ) ;
#43348 = EDGE_LOOP ( 'NONE', ( #5884, #32668, #38129, #16242 ) ) ;
#43349 = ADVANCED_FACE ( 'NONE', ( #39471 ), #47894, .T. ) ;
#43350 = CARTESIAN_POINT ( 'NONE',  ( -49.47517659412407198, -177.1207230881787780, 0.08879589532293177823 ) ) ;
#43351 = ORIENTED_EDGE ( 'NONE', *, *, #32478, .F. ) ;
#43352 = DIRECTION ( 'NONE',  ( -0.000000000000000000, 0.8229838658936613482, 0.5680647467311485954 ) ) ;
#43353 = VECTOR ( 'NONE', #50536, 1000.000000000000000 ) ;
#43354 = DIRECTION ( 'NONE',  ( 0.000000000000000000, -0.9350162426854121689, 0.3546048870425426713 ) ) ;
#43355 = EDGE_CURVE ( 'NONE', #25869, #44162, #15314, .T. ) ;
#43356 = VERTEX_POINT ( 'NONE', #42900 ) ;
#43357 = AXIS2_PLACEMENT_3D ( 'NONE', #21318, #37857, #29198 ) ;
#43358 = CARTESIAN_POINT ( 'NONE',  ( -332.3517673607765914, -135.0638248728647852, 57.91551518289418254 ) ) ;
#43359 = DIRECTION ( 'NONE',  ( 1.000000000000000000, 0.000000000000000000, -0.000000000000000000 ) ) ;
#43360 = PLANE ( 'NONE',  #29957 ) ;
#43361 = VECTOR ( 'NONE', #8506, 1000.000000000000114 ) ;
#43362 = CARTESIAN_POINT ( 'NONE',  ( 76.37123734610607073, -177.1207230881787780, 6.114457023561876703 ) ) ;
#43363 = ADVANCED_FACE ( 'NONE', ( #7166 ), #3729, .F. ) ;
#43364 = VERTEX_POINT ( 'NONE', #11098 ) ;
#43365 = DIRECTION ( 'NONE',  ( 0.000000000000000000, 0.000000000000000000, 1.000000000000000000 ) ) ;
#43366 = VECTOR ( 'NONE', #6692, 1000.000000000000000 ) ;
#43367 = PLANE ( 'NONE',  #24618 ) ;
#43368 = DIRECTION ( 'NONE',  ( -0.000000000000000000, 0.000000000000000000, 1.000000000000000000 ) ) ;
#43369 = EDGE_CURVE ( 'NONE', #40095, #37488, #26867, .T. ) ;
#43370 = CIRCLE ( 'NONE', #22393, 125.0000000000000000 ) ;
#43371 = DIRECTION ( 'NONE',  ( 0.000000000000000000, -1.000000000000000000, -0.000000000000000000 ) ) ;
#43372 = EDGE_LOOP ( 'NONE', ( #29657, #28646, #10268, #12816 ) ) ;
#43373 = CARTESIAN_POINT ( 'NONE',  ( -98.71382891444399377, -175.3837268820161057, -114.4616734920523555 ) ) ;
#43374 = DIRECTION ( 'NONE',  ( 0.000000000000000000, 0.000000000000000000, -1.000000000000000000 ) ) ;
#43375 = CARTESIAN_POINT ( 'NONE',  ( -305.0000000000000568, -63.99980407363861445, -7.728304129924412180 ) ) ;
#43377 = VERTEX_POINT ( 'NONE', #39715 ) ;
#43376 = CYLINDRICAL_SURFACE ( 'NONE', #11515, 124.9999999999999858 ) ;
#43378 = ORIENTED_EDGE ( 'NONE', *, *, #19525, .T. ) ;
#43379 = ORIENTED_EDGE ( 'NONE', *, *, #25165, .F. ) ;
#43380 = EDGE_CURVE ( 'NONE', #37325, #27840, #17806, .T. ) ;
#43381 = AXIS2_PLACEMENT_3D ( 'NONE', #49531, #45579, #9564 ) ;
#43382 = CARTESIAN_POINT ( 'NONE',  ( -63.31390705753092618, -175.3837268820161057, 123.1094209424469312 ) ) ;
#43383 = CIRCLE ( 'NONE', #6444, 125.0000000000000000 ) ;
#43384 = CARTESIAN_POINT ( 'NONE',  ( -332.3517673607765914, -123.5000000000000284, 0.000000000000000000 ) ) ;
#43385 = DIRECTION ( 'NONE',  ( 0.000000000000000000, 0.000000000000000000, -1.000000000000000000 ) ) ;
#43386 = VECTOR ( 'NONE', #39567, 1000.000000000000114 ) ;
#43387 = VERTEX_POINT ( 'NONE', #15845 ) ;
#43388 = CARTESIAN_POINT ( 'NONE',  ( 1.989912926925674563, 50.94255943192818137, -21.04850772462241082 ) ) ;
#43389 = ORIENTED_EDGE ( 'NONE', *, *, #39058, .T. ) ;
#43390 = AXIS2_PLACEMENT_3D ( 'NONE', #16188, #28261, #4104 ) ;
#43391 = EDGE_LOOP ( 'NONE', ( #7385, #18079, #13344, #10015 ) ) ;
#43392 = AXIS2_PLACEMENT_3D ( 'NONE', #44124, #24417, #11797 ) ;
#43393 = ORIENTED_EDGE ( 'NONE', *, *, #34387, .F. ) ;
#43394 = CARTESIAN_POINT ( 'NONE',  ( -151.4272465800706016, -177.1207230881787780, 70.89911581792887318 ) ) ;
#43395 = AXIS2_PLACEMENT_3D ( 'NONE', #4237, #1528, #3979 ) ;
#43396 = VECTOR ( 'NONE', #40498, 1000.000000000000227 ) ;
#43397 = ADVANCED_FACE ( 'NONE', ( #3473 ), #22941, .T. ) ;
#43398 = EDGE_CURVE ( 'NONE', #17017, #43316, #31329, .T. ) ;
#43400 = VECTOR ( 'NONE', #27678, 1000.000000000000000 ) ;
#43399 = CARTESIAN_POINT ( 'NONE',  ( -339.1964088526558498, -138.1050951016792681, -57.16590939599323917 ) ) ;
#43401 = ORIENTED_EDGE ( 'NONE', *, *, #7675, .F. ) ;
#43402 = VECTOR ( 'NONE', #26790, 1000.000000000000000 ) ;
#43403 = LINE ( 'NONE', #6367, #45311 ) ;
#43404 = DIRECTION ( 'NONE',  ( 1.043714542225393381E-14, -0.2393156642875582940, -0.9709418174260519008 ) ) ;
#43407 = ORIENTED_EDGE ( 'NONE', *, *, #10125, .F. ) ;
#43406 = DIRECTION ( 'NONE',  ( 1.000000000000000000, -0.000000000000000000, 0.000000000000000000 ) ) ;
#43405 = CARTESIAN_POINT ( 'NONE',  ( -147.2362428880188077, -177.1207230881787780, -74.98773087994455011 ) ) ;
#43408 = DIRECTION ( 'NONE',  ( -0.000000000000000000, 1.000000000000000000, 0.000000000000000000 ) ) ;
#43409 = ORIENTED_EDGE ( 'NONE', *, *, #39488, .F. ) ;
#43410 = CYLINDRICAL_SURFACE ( 'NONE', #2901, 125.0000000000000000 ) ;
#43411 = ORIENTED_EDGE ( 'NONE', *, *, #24243, .T. ) ;
#43412 = DIRECTION ( 'NONE',  ( 0.000000000000000000, -1.000000000000000000, 0.000000000000000000 ) ) ;
#43413 = PLANE ( 'NONE',  #16241 ) ;
#43415 = LINE ( 'NONE', #51553, #45838 ) ;
#43414 = FACE_OUTER_BOUND ( 'NONE', #43064, .T. ) ;
#43416 = ORIENTED_EDGE ( 'NONE', *, *, #33444, .T. ) ;
#43417 = CARTESIAN_POINT ( 'NONE',  ( -339.1964088526558498, -96.52406086224361559, 52.47426709956096147 ) ) ;
#43418 = AXIS2_PLACEMENT_3D ( 'NONE', #17114, #33120, #36537 ) ;
#43419 = ORIENTED_EDGE ( 'NONE', *, *, #48573, .T. ) ;
#43420 = LINE ( 'NONE', #18726, #2973 ) ;
#43421 = AXIS2_PLACEMENT_3D ( 'NONE', #5575, #14234, #30253 ) ;
#43422 = ORIENTED_EDGE ( 'NONE', *, *, #45609, .T. ) ;
#43423 = EDGE_CURVE ( 'NONE', #4180, #2804, #35790, .T. ) ;
#43424 = CARTESIAN_POINT ( 'NONE',  ( -50.89116676070551648, -183.6283474603465606, 124.9767260852757147 ) ) ;
#43425 = VECTOR ( 'NONE', #18115, 999.9999999999998863 ) ;
#43426 = DIRECTION ( 'NONE',  ( -0.000000000000000000, 1.000000000000000000, -0.000000000000000000 ) ) ;
#43427 = ORIENTED_EDGE ( 'NONE', *, *, #42998, .T. ) ;
#43428 = CARTESIAN_POINT ( 'NONE',  ( -170.9948556092908234, -193.5000000000000000, 19.12855698118475090 ) ) ;
#43429 = CARTESIAN_POINT ( 'NONE',  ( -336.3521761649654422, -139.2044816956407089, -56.89493493766761389 ) ) ;
#43430 = EDGE_CURVE ( 'NONE', #18675, #32483, #36173, .T. ) ;
#43431 = ORIENTED_EDGE ( 'NONE', *, *, #3608, .T. ) ;
#43432 = DIRECTION ( 'NONE',  ( -0.000000000000000000, -1.000000000000000000, -0.000000000000000000 ) ) ;
#43433 = ORIENTED_EDGE ( 'NONE', *, *, #41059, .F. ) ;
#43434 = VECTOR ( 'NONE', #19534, 1000.000000000000227 ) ;
#43435 = CARTESIAN_POINT ( 'NONE',  ( -88.78924379339709105, -183.6283474603465606, -118.3219948448692662 ) ) ;
#43436 = AXIS2_PLACEMENT_3D ( 'NONE', #50001, #30275, #2153 ) ;
#43437 = CARTESIAN_POINT ( 'NONE',  ( -339.1964088526558498, -83.33976666099020747, -44.57752413667995484 ) ) ;
#43438 = VECTOR ( 'NONE', #24593, 1000.000000000000000 ) ;
#43439 = CARTESIAN_POINT ( 'NONE',  ( 45.28027613463186185, 28.00000000000000355, -47.36004163347733709 ) ) ;
#43440 = DIRECTION ( 'NONE',  ( -0.000000000000000000, 1.000000000000000000, -0.000000000000000000 ) ) ;
#43441 = DIRECTION ( 'NONE',  ( -0.000000000000000000, 1.000000000000000000, -0.000000000000000000 ) ) ;
#43442 = MECHANICAL_DESIGN_GEOMETRIC_PRESENTATION_REPRESENTATION (  '', ( #42484 ), #1376 ) ;
#43444 = VECTOR ( 'NONE', #32276, 1000.000000000000000 ) ;
#43443 = DIRECTION ( 'NONE',  ( 0.000000000000000000, 0.000000000000000000, 1.000000000000000000 ) ) ;
#43445 = PLANE ( 'NONE',  #18636 ) ;
#43446 = LINE ( 'NONE', #11880, #46583 ) ;
#43448 = VERTEX_POINT ( 'NONE', #43161 ) ;
#43447 = CARTESIAN_POINT ( 'NONE',  ( -136.5246168469702468, -193.5000000000000000, 87.31661597576146505 ) ) ;
#43449 = ORIENTED_EDGE ( 'NONE', *, *, #51654, .T. ) ;
#43450 = CARTESIAN_POINT ( 'NONE',  ( 67.87295084395105960, -193.5000000000000000, 42.87565520599286373 ) ) ;
#43451 = DIRECTION ( 'NONE',  ( 0.000000000000000000, -0.000000000000000000, 1.000000000000000000 ) ) ;
#43452 = EDGE_LOOP ( 'NONE', ( #10994, #31908, #32012, #44265 ) ) ;
#43453 = CIRCLE ( 'NONE', #24139, 9.999999999999994671 ) ;
#43454 = AXIS2_PLACEMENT_3D ( 'NONE', #6314, #18407, #14465 ) ;
#43455 = ORIENTED_EDGE ( 'NONE', *, *, #32558, .F. ) ;
#43456 = DIRECTION ( 'NONE',  ( -0.3202698538628350744, 0.000000000000000000, -0.9473263538541923934 ) ) ;
#43457 = VERTEX_POINT ( 'NONE', #47644 ) ;
#43458 = CARTESIAN_POINT ( 'NONE',  ( -166.2107720749848738, -193.5000000000000000, -38.92640747825594616 ) ) ;
#43459 = CARTESIAN_POINT ( 'NONE',  ( -71.22983192549011733, -189.7472609257535510, -121.8950816227732759 ) ) ;
#43460 = AXIS2_PLACEMENT_3D ( 'NONE', #48698, #15867, #32130 ) ;
#43461 = EDGE_CURVE ( 'NONE', #17455, #17248, #23962, .T. ) ;
#43462 = CARTESIAN_POINT ( 'NONE',  ( -49.13194886969936448, -193.5000000000000000, -0.7575112421616214675 ) ) ;
#43463 = CARTESIAN_POINT ( 'NONE',  ( -336.3521761649654422, -67.75522407825191351, 19.39547174791671935 ) ) ;
#43464 = ORIENTED_EDGE ( 'NONE', *, *, #7411, .F. ) ;
#43465 = VERTEX_POINT ( 'NONE', #11628 ) ;
#43466 = VERTEX_POINT ( 'NONE', #43437 ) ;
#43467 = DIRECTION ( 'NONE',  ( 0.000000000000000000, 0.000000000000000000, 1.000000000000000000 ) ) ;
#43468 = CARTESIAN_POINT ( 'NONE',  ( -332.3517673607765914, -156.2279223070262049, 50.28800156563452362 ) ) ;
#43469 = AXIS2_PLACEMENT_3D ( 'NONE', #32967, #49015, #24569 ) ;
#43470 = DIRECTION ( 'NONE',  ( -0.000000000000000000, 1.000000000000000000, -0.000000000000000000 ) ) ;
#43471 = DIRECTION ( 'NONE',  ( 1.000000000000000000, -0.000000000000000000, 0.000000000000000000 ) ) ;
#43472 = DIRECTION ( 'NONE',  ( 0.9785564922995046988, 0.000000000000000000, -0.2059786187410953262 ) ) ;
#43473 = ORIENTED_EDGE ( 'NONE', *, *, #30054, .F. ) ;
#43474 = CARTESIAN_POINT ( 'NONE',  ( -330.4913330509368166, -123.5000000000000284, 0.000000000000000000 ) ) ;
#43475 = FACE_OUTER_BOUND ( 'NONE', #43030, .T. ) ;
#43476 = AXIS2_PLACEMENT_3D ( 'NONE', #49446, #20789, #8432 ) ;
#43477 = ORIENTED_EDGE ( 'NONE', *, *, #641, .F. ) ;
#43478 = VERTEX_POINT ( 'NONE', #23207 ) ;
#43479 = EDGE_LOOP ( 'NONE', ( #50185, #14833, #31703, #10078 ) ) ;
#43480 = DIRECTION ( 'NONE',  ( -0.000000000000000000, 1.000000000000000000, -0.000000000000000000 ) ) ;
#43481 = DIRECTION ( 'NONE',  ( 0.000000000000000000, -0.9350162426854158326, -0.3546048870425331789 ) ) ;
#43482 = ORIENTED_EDGE ( 'NONE', *, *, #8264, .F. ) ;
#43483 = EDGE_CURVE ( 'NONE', #33612, #15472, #7682, .T. ) ;
#43484 = DIRECTION ( 'NONE',  ( 0.000000000000000000, 0.000000000000000000, -1.000000000000000000 ) ) ;
#43485 = CARTESIAN_POINT ( 'NONE',  ( -330.4913330509368166, -103.0458197858332312, -55.34326076196081345 ) ) ;
#43486 = CARTESIAN_POINT ( 'NONE',  ( -70.75782287548091176, -175.3837268820161057, 122.9986166548864759 ) ) ;
#43487 = ORIENTED_EDGE ( 'NONE', *, *, #2896, .F. ) ;
#43488 = DIRECTION ( 'NONE',  ( 0.9960498426152177842, 0.000000000000000000, -0.08879589532292482545 ) ) ;
#43489 = ORIENTED_EDGE ( 'NONE', *, *, #1518, .T. ) ;
#43490 = DIRECTION ( 'NONE',  ( 0.000000000000000000, 0.000000000000000000, 1.000000000000000000 ) ) ;
#43491 = CIRCLE ( 'NONE', #19993, 125.0000000000000000 ) ;
#43492 = VECTOR ( 'NONE', #6876, 1000.000000000000000 ) ;
#43493 = DIRECTION ( 'NONE',  ( -0.000000000000000000, 1.000000000000000000, -0.000000000000000000 ) ) ;
#43494 = EDGE_LOOP ( 'NONE', ( #23510, #13977, #39753, #35102 ) ) ;
#43495 = VECTOR ( 'NONE', #6626, 1000.000000000000000 ) ;
#43496 = DIRECTION ( 'NONE',  ( 0.000000000000000000, 0.000000000000000000, 1.000000000000000000 ) ) ;
#43497 = DIRECTION ( 'NONE',  ( 0.000000000000000000, 0.000000000000000000, 1.000000000000000000 ) ) ;
#43498 = LINE ( 'NONE', #19572, #8927 ) ;
#43499 = DIRECTION ( 'NONE',  ( 0.8294056854502049880, 0.000000000000000000, -0.5586467658036476935 ) ) ;
#43500 = FACE_OUTER_BOUND ( 'NONE', #45634, .T. ) ;
#43501 = VERTEX_POINT ( 'NONE', #36569 ) ;
#43502 = VERTEX_POINT ( 'NONE', #4006 ) ;
#43503 = AXIS2_PLACEMENT_3D ( 'NONE', #13404, #2076, #1309 ) ;
#43504 = CARTESIAN_POINT ( 'NONE',  ( -336.3521761649654422, -80.42027357919624819, -40.34602258462219027 ) ) ;
#43506 = VERTEX_POINT ( 'NONE', #4522 ) ;
#43505 = PLANE ( 'NONE',  #14529 ) ;
#43507 = EDGE_CURVE ( 'NONE', #210, #38978, #12123, .T. ) ;
#43508 = ORIENTED_EDGE ( 'NONE', *, *, #20495, .F. ) ;
#43509 = FACE_OUTER_BOUND ( 'NONE', #37980, .T. ) ;
#43510 = VECTOR ( 'NONE', #43849, 1000.000000000000114 ) ;
#43511 = ADVANCED_FACE ( 'NONE', ( #9252 ), #8202, .T. ) ;
#43512 = DIRECTION ( 'NONE',  ( 0.000000000000000000, 0.000000000000000000, 1.000000000000000000 ) ) ;
#43513 = ORIENTED_EDGE ( 'NONE', *, *, #21819, .T. ) ;
#43514 = DIRECTION ( 'NONE',  ( -0.000000000000000000, 1.000000000000000000, -0.000000000000000000 ) ) ;
#43515 = FACE_OUTER_BOUND ( 'NONE', #49328, .T. ) ;
#43516 = EDGE_LOOP ( 'NONE', ( #37274, #38161 ) ) ;
#43517 = CARTESIAN_POINT ( 'NONE',  ( -339.1964088526558498, -171.7720157143604069, -33.92731199008472487 ) ) ;
#43518 = ADVANCED_FACE ( 'NONE', ( #16095 ), #13190, .T. ) ;
#43519 = DIRECTION ( 'NONE',  ( -0.000000000000000000, 1.000000000000000000, -0.000000000000000000 ) ) ;
#43520 = DIRECTION ( 'NONE',  ( -0.000000000000000000, 1.000000000000000000, -0.000000000000000000 ) ) ;
#43521 = ORIENTED_EDGE ( 'NONE', *, *, #39806, .T. ) ;
#43522 = EDGE_LOOP ( 'NONE', ( #44196, #48916, #22032, #24137 ) ) ;
#43523 = EDGE_CURVE ( 'NONE', #42284, #19235, #44997, .T. ) ;
#43524 = ORIENTED_EDGE ( 'NONE', *, *, #4766, .F. ) ;
#43525 = PLANE ( 'NONE',  #49252 ) ;
#43526 = CARTESIAN_POINT ( 'NONE',  ( 46.00000000000000711, 20.00000000000000000, -46.00000000000000000 ) ) ;
#43527 = VECTOR ( 'NONE', #32421, 1000.000000000000000 ) ;
#43528 = ADVANCED_FACE ( 'NONE', ( #28155 ), #25023, .T. ) ;
#43529 = AXIS2_PLACEMENT_3D ( 'NONE', #26778, #26009, #42033 ) ;
#43530 = CARTESIAN_POINT ( 'NONE',  ( 34.93559171950835918, -183.6283474603465606, -93.09664195018496002 ) ) ;
#43531 = DIRECTION ( 'NONE',  ( 0.000000000000000000, 0.000000000000000000, 1.000000000000000000 ) ) ;
#43532 = PLANE ( 'NONE',  #49068 ) ;
#43533 = ORIENTED_EDGE ( 'NONE', *, *, #18247, .T. ) ;
#43534 = CARTESIAN_POINT ( 'NONE',  ( -9.671950287350391307, -177.1207230881787780, -118.8234112238815499 ) ) ;
#43535 = ORIENTED_EDGE ( 'NONE', *, *, #47796, .T. ) ;
#43537 = VERTEX_POINT ( 'NONE', #20537 ) ;
#43536 = DIRECTION ( 'NONE',  ( -0.000000000000000000, 1.000000000000000000, -0.000000000000000000 ) ) ;
#43538 = VECTOR ( 'NONE', #3627, 1000.000000000000000 ) ;
#43539 = ORIENTED_EDGE ( 'NONE', *, *, #15773, .T. ) ;
#43540 = DIRECTION ( 'NONE',  ( 0.000000000000000000, 1.000000000000000000, 0.000000000000000000 ) ) ;
#43541 = ADVANCED_FACE ( 'NONE', ( #16874 ), #4257, .T. ) ;
#43542 = DIRECTION ( 'NONE',  ( 0.000000000000000000, 0.9350162426854132791, -0.3546048870425396182 ) ) ;
#43543 = LINE ( 'NONE', #7023, #31350 ) ;
#43544 = FACE_OUTER_BOUND ( 'NONE', #30342, .T. ) ;
#43545 = EDGE_LOOP ( 'NONE', ( #20937, #41109, #16162, #48166 ) ) ;
#43546 = CARTESIAN_POINT ( 'NONE',  ( -101.9736325116273576, -177.1207230881787780, 112.9749434763330811 ) ) ;
#43547 = VERTEX_POINT ( 'NONE', #36309 ) ;
#43548 = VECTOR ( 'NONE', #29050, 1000.000000000000114 ) ;
#43549 = ORIENTED_EDGE ( 'NONE', *, *, #26926, .F. ) ;
#43550 = LINE ( 'NONE', #40355, #17880 ) ;
#43551 = DIRECTION ( 'NONE',  ( -0.6068001458186002006, 0.000000000000000000, 0.7948544414133481562 ) ) ;
#43552 = DIRECTION ( 'NONE',  ( -0.9266896074318370369, 0.000000000000000000, 0.3758275821142292306 ) ) ;
#43553 = DIRECTION ( 'NONE',  ( 0.000000000000000000, -0.4739294676984007193, 0.8805628084623552398 ) ) ;
#43554 = DIRECTION ( 'NONE',  ( -1.000000000000000000, 0.000000000000000000, -4.884776371667510679E-16 ) ) ;
#43555 = DIRECTION ( 'NONE',  ( 0.4031234292879600778, 0.000000000000000000, 0.9151456172430237901 ) ) ;
#43556 = DIRECTION ( 'NONE',  ( -0.000000000000000000, 1.000000000000000000, 0.000000000000000000 ) ) ;
#43557 = ORIENTED_EDGE ( 'NONE', *, *, #36202, .F. ) ;
#43558 = CARTESIAN_POINT ( 'NONE',  ( -131.8938452225253855, -183.6283474603465606, 93.09664195018558530 ) ) ;
#43559 = CARTESIAN_POINT ( 'NONE',  ( -332.3517673607765914, -69.26746417191145611, -23.38292116578723068 ) ) ;
#43560 = FACE_BOUND ( 'NONE', #19789, .T. ) ;
#43561 = ORIENTED_EDGE ( 'NONE', *, *, #12788, .T. ) ;
#43562 = AXIS2_PLACEMENT_3D ( 'NONE', #37034, #13129, #29150 ) ;
#43563 = LINE ( 'NONE', #27262, #25596 ) ;
#43564 = VECTOR ( 'NONE', #16191, 1000.000000000000000 ) ;
#43565 = CARTESIAN_POINT ( 'NONE',  ( -48.65601702663141737, -183.6283474603465606, -0.9842305779475923888 ) ) ;
#43566 = EDGE_CURVE ( 'NONE', #10561, #4246, #12648, .T. ) ;
#43567 = VERTEX_POINT ( 'NONE', #45267 ) ;
#43568 = EDGE_CURVE ( 'NONE', #31066, #34017, #33671, .T. ) ;
#43569 = CARTESIAN_POINT ( 'NONE',  ( -30.31202594373734627, -193.5000000000000000, -123.6727797384705809 ) ) ;
#43570 = ORIENTED_EDGE ( 'NONE', *, *, #2036, .T. ) ;
#43571 = VECTOR ( 'NONE', #14116, 1000.000000000000000 ) ;
#43572 = DIRECTION ( 'NONE',  ( -1.000000000000000000, -0.000000000000000000, -0.000000000000000000 ) ) ;
#43573 = FACE_BOUND ( 'NONE', #46657, .T. ) ;
#43575 = EDGE_LOOP ( 'NONE', ( #2919, #40811, #10760, #43304 ) ) ;
#43574 = FACE_OUTER_BOUND ( 'NONE', #35831, .T. ) ;
#43576 = EDGE_CURVE ( 'NONE', #24186, #6302, #8452, .T. ) ;
#43577 = DIRECTION ( 'NONE',  ( -0.000000000000000000, -1.000000000000000000, 0.000000000000000000 ) ) ;
#43578 = ORIENTED_EDGE ( 'NONE', *, *, #12757, .T. ) ;
#43579 = ADVANCED_FACE ( 'NONE', ( #16348 ), #12393, .T. ) ;
#43580 = AXIS2_PLACEMENT_3D ( 'NONE', #35849, #17126, #45253 ) ;
#43581 = ORIENTED_EDGE ( 'NONE', *, *, #27607, .T. ) ;
#43582 = CARTESIAN_POINT ( 'NONE',  ( -339.1964088526558498, -162.2499814621209850, 44.49369547121574442 ) ) ;
#43583 = EDGE_CURVE ( 'NONE', #34438, #48449, #23573, .T. ) ;
#43584 = ORIENTED_EDGE ( 'NONE', *, *, #14684, .T. ) ;
#43585 = PLANE ( 'NONE',  #48611 ) ;
#43586 = EDGE_CURVE ( 'NONE', #993, #20913, #37086, .T. ) ;
#43587 = DIRECTION ( 'NONE',  ( -0.000000000000000000, 0.8854560256532093554, -0.4647231720437695057 ) ) ;
#43588 = DIRECTION ( 'NONE',  ( 0.000000000000000000, 0.000000000000000000, 1.000000000000000000 ) ) ;
#43589 = EDGE_LOOP ( 'NONE', ( #40860, #920, #25094, #1718 ) ) ;
#43591 = ORIENTED_EDGE ( 'NONE', *, *, #44471, .F. ) ;
#43590 = CARTESIAN_POINT ( 'NONE',  ( -332.3517673607765914, -168.7445418633863596, -37.90245108779149064 ) ) ;
#43592 = ORIENTED_EDGE ( 'NONE', *, *, #43111, .F. ) ;
#43593 = AXIS2_PLACEMENT_3D ( 'NONE', #29345, #38259, #41949 ) ;
#43594 = CARTESIAN_POINT ( 'NONE',  ( -78.00521078983979351, -193.5000000000000000, 121.4627941443857111 ) ) ;
#43595 = EDGE_LOOP ( 'NONE', ( #10750, #17627, #9215, #45574 ) ) ;
#43596 = DIRECTION ( 'NONE',  ( 0.000000000000000000, 1.000000000000000000, 0.000000000000000000 ) ) ;
#43597 = CIRCLE ( 'NONE', #27535, 125.0000000000000000 ) ;
#43598 = VERTEX_POINT ( 'NONE', #5051 ) ;
#43599 = PLANE ( 'NONE',  #35962 ) ;
#43600 = ORIENTED_EDGE ( 'NONE', *, *, #38879, .T. ) ;
#43602 = DIRECTION ( 'NONE',  ( 0.000000000000000000, 1.000000000000000000, 0.000000000000000000 ) ) ;
#43601 = FACE_OUTER_BOUND ( 'NONE', #18415, .T. ) ;
#43603 = ORIENTED_EDGE ( 'NONE', *, *, #8551, .F. ) ;
#43604 = CARTESIAN_POINT ( 'NONE',  ( 72.71365293123227502, -183.6283474603465606, -30.61552143554913030 ) ) ;
#43605 = ORIENTED_EDGE ( 'NONE', *, *, #45769, .T. ) ;
#43606 = PLANE ( 'NONE',  #3537 ) ;
#43607 = PLANE ( 'NONE',  #26522 ) ;
#43608 = CARTESIAN_POINT ( 'NONE',  ( -305.0000000000000568, -181.0704707379907745, 16.90091414705587525 ) ) ;
#43609 = DIRECTION ( 'NONE',  ( -0.000000000000000000, -0.5680647467311485954, 0.8229838658936613482 ) ) ;
#43610 = FACE_OUTER_BOUND ( 'NONE', #16413, .T. ) ;
#43611 = DIRECTION ( 'NONE',  ( 0.000000000000000000, 0.9927088740980551940, 0.1205366802553130001 ) ) ;
#43612 = ORIENTED_EDGE ( 'NONE', *, *, #3577, .T. ) ;
#43613 = CARTESIAN_POINT ( 'NONE',  ( 0.000000000000000000, 0.000000000000000000, 0.000000000000000000 ) ) ;
#43614 = LINE ( 'NONE', #12326, #44810 ) ;
#43615 = PLANE ( 'NONE',  #29031 ) ;
#43616 = CIRCLE ( 'NONE', #15944, 125.0000000000000000 ) ;
#43617 = ADVANCED_FACE ( 'NONE', ( #44725 ), #24749, .T. ) ;
#43618 = DIRECTION ( 'NONE',  ( -0.000000000000000000, 1.000000000000000000, -0.000000000000000000 ) ) ;
#43619 = VERTEX_POINT ( 'NONE', #48933 ) ;
#43620 = CARTESIAN_POINT ( 'NONE',  ( -339.1964088526558498, -182.0095552316575152, 7.608018572113563138 ) ) ;
#43621 = DIRECTION ( 'NONE',  ( 0.000000000000000000, 0.000000000000000000, -1.000000000000000000 ) ) ;
#43622 = ADVANCED_FACE ( 'NONE', ( #21065 ), #17135, .T. ) ;
#43623 = CARTESIAN_POINT ( 'NONE',  ( -169.1033029113419559, -189.7472609257535510, 32.78426643622744052 ) ) ;
#43625 = ORIENTED_EDGE ( 'NONE', *, *, #14285, .F. ) ;
#43624 = DIRECTION ( 'NONE',  ( 0.000000000000000000, 1.000000000000000000, -0.000000000000000000 ) ) ;
#43626 = ADVANCED_FACE ( 'NONE', ( #10031 ), #49469, .F. ) ;
#43627 = EDGE_CURVE ( 'NONE', #6745, #19363, #6339, .T. ) ;
#43628 = ORIENTED_EDGE ( 'NONE', *, *, #4271, .T. ) ;
#43629 = ORIENTED_EDGE ( 'NONE', *, *, #26294, .F. ) ;
#43630 = ADVANCED_FACE ( 'NONE', ( #17912 ), #29460, .F. ) ;
#43631 = FACE_BOUND ( 'NONE', #26387, .T. ) ;
#43632 = EDGE_CURVE ( 'NONE', #4146, #5935, #30250, .T. ) ;
#43633 = CARTESIAN_POINT ( 'NONE',  ( -48.47912675150885065, -177.1207230881787780, 6.938893903907228378E-15 ) ) ;
#43634 = DIRECTION ( 'NONE',  ( 0.000000000000000000, 0.000000000000000000, 1.000000000000000000 ) ) ;
#43635 = CARTESIAN_POINT ( 'NONE',  ( -330.4913330509368166, -162.9117225908391333, -45.24064679492040142 ) ) ;
#43636 = EDGE_LOOP ( 'NONE', ( #1253, #9340, #14467, #42237 ) ) ;
#43637 = ADVANCED_FACE ( 'NONE', ( #13703 ), #45512, .T. ) ;
#43638 = CARTESIAN_POINT ( 'NONE',  ( 1.446991361456883896, 50.76983389525828727, -21.20535062037070517 ) ) ;
#43639 = EDGE_CURVE ( 'NONE', #49683, #40790, #1777, .T. ) ;
#43640 = EDGE_LOOP ( 'NONE', ( #6707, #13636, #12271, #34478 ) ) ;
#43641 = ORIENTED_EDGE ( 'NONE', *, *, #10256, .T. ) ;
#43642 = EDGE_CURVE ( 'NONE', #21275, #31707, #38118, .T. ) ;
#43643 = VERTEX_POINT ( 'NONE', #46295 ) ;
#43644 = LINE ( 'NONE', #36268, #12457 ) ;
#43645 = EDGE_CURVE ( 'NONE', #18653, #46318, #41543, .T. ) ;
#43646 = CARTESIAN_POINT ( 'NONE',  ( -49.38192458147459973, -177.1207230881787780, 0.4300652022765185656 ) ) ;
#43647 = ORIENTED_EDGE ( 'NONE', *, *, #4058, .F. ) ;
#43648 = EDGE_CURVE ( 'NONE', #48702, #15921, #10276, .T. ) ;
#43649 = AXIS2_PLACEMENT_3D ( 'NONE', #26129, #46131, #10112 ) ;
#43650 = AXIS2_PLACEMENT_3D ( 'NONE', #8276, #36125, #44011 ) ;
#43651 = DIRECTION ( 'NONE',  ( 0.000000000000000000, 1.000000000000000000, 0.000000000000000000 ) ) ;
#43652 = DIRECTION ( 'NONE',  ( -0.000000000000000000, 0.9927088740980538617, -0.1205366802553232974 ) ) ;
#43655 = EDGE_LOOP ( 'NONE', ( #4274, #22120, #17056, #14021 ) ) ;
#43654 = CARTESIAN_POINT ( 'NONE',  ( -15.48416040178639008, -183.6283474603465606, 119.5301634136914970 ) ) ;
#43653 = DIRECTION ( 'NONE',  ( 0.8757349421956310831, 0.000000000000000000, 0.4827922027307550712 ) ) ;
#43656 = DIRECTION ( 'NONE',  ( -0.9646355819083576311, 0.000000000000000000, -0.2635871660690715101 ) ) ;
#43657 = ORIENTED_EDGE ( 'NONE', *, *, #38806, .T. ) ;
#43658 = CARTESIAN_POINT ( 'NONE',  ( -339.1964088526558498, -79.00630452878414189, 38.74998146212082162 ) ) ;
#43659 = ORIENTED_EDGE ( 'NONE', *, *, #41486, .F. ) ;
#43660 = CARTESIAN_POINT ( 'NONE',  ( -170.0000000000000284, -93.50000000000002842, 51.54700538379266561 ) ) ;
#43661 = DIRECTION ( 'NONE',  ( 0.000000000000000000, 1.000000000000000000, -0.000000000000000000 ) ) ;
#43663 = CARTESIAN_POINT ( 'NONE',  ( 19.33815737959698566, -193.5000000000000000, 105.0038855142078233 ) ) ;
#43662 = DIRECTION ( 'NONE',  ( 0.000000000000000000, -1.000000000000000000, -0.000000000000000000 ) ) ;
#43664 = ADVANCED_FACE ( 'NONE', ( #49969 ), #38389, .F. ) ;
#43665 = ORIENTED_EDGE ( 'NONE', *, *, #27844, .T. ) ;
#43666 = DIRECTION ( 'NONE',  ( 0.000000000000000000, 0.000000000000000000, -1.000000000000000000 ) ) ;
#43667 = PLANE ( 'NONE',  #14434 ) ;
#43669 = AXIS2_PLACEMENT_3D ( 'NONE', #45660, #38268, #9645 ) ;
#43668 = PLANE ( 'NONE',  #29228 ) ;
#43670 = ORIENTED_EDGE ( 'NONE', *, *, #7511, .T. ) ;
#43671 = LINE ( 'NONE', #27374, #34158 ) ;
#43672 = PLANE ( 'NONE',  #8913 ) ;
#43673 = CARTESIAN_POINT ( 'NONE',  ( -146.0653709326077490, -189.7472609257535510, -78.11481899503411341 ) ) ;
#43674 = ORIENTED_EDGE ( 'NONE', *, *, #14930, .T. ) ;
#43675 = LINE ( 'NONE', #15565, #13330 ) ;
#43676 = FACE_OUTER_BOUND ( 'NONE', #25100, .T. ) ;
#43677 = LINE ( 'NONE', #8393, #46348 ) ;
#43678 = VERTEX_POINT ( 'NONE', #14489 ) ;
#43679 = LINE ( 'NONE', #22937, #45103 ) ;
#43680 = ORIENTED_EDGE ( 'NONE', *, *, #4927, .F. ) ;
#43681 = LINE ( 'NONE', #31072, #23133 ) ;
#43682 = CARTESIAN_POINT ( 'NONE',  ( -180.0000000000000568, -115.7896721143442278, -60.00000000000000711 ) ) ;
#43683 = ADVANCED_FACE ( 'NONE', ( #25272 ), #45766, .T. ) ;
#43684 = PLANE ( 'NONE',  #38622 ) ;
#43685 = DIRECTION ( 'NONE',  ( 0.000000000000000000, 0.000000000000000000, 1.000000000000000000 ) ) ;
#43686 = DIRECTION ( 'NONE',  ( -0.000000000000000000, 1.000000000000000000, -0.000000000000000000 ) ) ;
#43687 = ADVANCED_FACE ( 'NONE', ( #41286 ), #5573, .T. ) ;
#43688 = VECTOR ( 'NONE', #2927, 1000.000000000000114 ) ;
#43689 = ADVANCED_FACE ( 'NONE', ( #6084 ), #46044, .F. ) ;
#43690 = AXIS2_PLACEMENT_3D ( 'NONE', #6912, #22944, #35027 ) ;
#43691 = DIRECTION ( 'NONE',  ( -0.000000000000000000, 1.000000000000000000, -0.000000000000000000 ) ) ;
#43692 = EDGE_CURVE ( 'NONE', #24091, #19650, #21858, .T. ) ;
#43693 = DIRECTION ( 'NONE',  ( 0.7378332790417189146, 0.000000000000000000, 0.6749830015182196608 ) ) ;
#43694 = CARTESIAN_POINT ( 'NONE',  ( -146.0653709326077490, -175.3837268820161057, -78.11481899503409920 ) ) ;
#43696 = EDGE_LOOP ( 'NONE', ( #22621, #15528, #50393, #34157, #48625, #26233, #43115, #15925 ) ) ;
#43695 = CARTESIAN_POINT ( 'NONE',  ( -123.4791267515088435, -173.5000000000000284, 80.00000000000000000 ) ) ;
#43697 = ORIENTED_EDGE ( 'NONE', *, *, #33741, .T. ) ;
#43698 = FACE_OUTER_BOUND ( 'NONE', #20578, .T. ) ;
#43699 = CARTESIAN_POINT ( 'NONE',  ( -48.47912675150885065, -183.6283474603465606, 6.938893903907228378E-15 ) ) ;
#43700 = VERTEX_POINT ( 'NONE', #17410 ) ;
#43701 = VERTEX_POINT ( 'NONE', #9763 ) ;
#43702 = AXIS2_PLACEMENT_3D ( 'NONE', #9851, #2220, #50323 ) ;
#43703 = LINE ( 'NONE', #7703, #44987 ) ;
#43704 = EDGE_CURVE ( 'NONE', #14725, #18880, #25791, .T. ) ;
#43705 = ORIENTED_EDGE ( 'NONE', *, *, #41321, .T. ) ;
#43706 = CARTESIAN_POINT ( 'NONE',  ( 10.22625775207004928, -193.5000000000000000, -109.2239789693433352 ) ) ;
#43707 = CARTESIAN_POINT ( 'NONE',  ( -339.1964088526558498, -143.9541802141672235, -55.34326076196065003 ) ) ;
#43708 = FACE_OUTER_BOUND ( 'NONE', #31208, .T. ) ;
#43709 = DIRECTION ( 'NONE',  ( -0.000000000000000000, 1.000000000000000000, -0.000000000000000000 ) ) ;
#43710 = ORIENTED_EDGE ( 'NONE', *, *, #36002, .T. ) ;
#43711 = EDGE_LOOP ( 'NONE', ( #5167, #7458, #45989, #2447 ) ) ;
#43712 = EDGE_CURVE ( 'NONE', #43188, #40339, #32506, .T. ) ;
#43713 = ORIENTED_EDGE ( 'NONE', *, *, #40235, .F. ) ;
#43714 = CARTESIAN_POINT ( 'NONE',  ( 44.30815888362531041, -175.3837268820161057, 83.75869879877568280 ) ) ;
#43715 = DIRECTION ( 'NONE',  ( -0.9646355819083614058, 0.000000000000000000, 0.2635871660690581320 ) ) ;
#43716 = CARTESIAN_POINT ( 'NONE',  ( -305.0000000000000568, -80.37812621821328207, -41.71934804796994456 ) ) ;
#43717 = FACE_OUTER_BOUND ( 'NONE', #45431, .T. ) ;
#43718 = FACE_OUTER_BOUND ( 'NONE', #50893, .T. ) ;
#43719 = ORIENTED_EDGE ( 'NONE', *, *, #10125, .T. ) ;
#43720 = DIRECTION ( 'NONE',  ( 0.000000000000000000, 0.000000000000000000, 1.000000000000000000 ) ) ;
#43721 = AXIS2_PLACEMENT_3D ( 'NONE', #30758, #27325, #43103 ) ;
#43722 = CARTESIAN_POINT ( 'NONE',  ( -90.87721961371603641, -175.3837268820161057, 116.5264228893328777 ) ) ;
#43723 = LINE ( 'NONE', #29250, #18197 ) ;
#43724 = VECTOR ( 'NONE', #33672, 1000.000000000000114 ) ;
#43725 = VERTEX_POINT ( 'NONE', #3165 ) ;
#43726 = ORIENTED_EDGE ( 'NONE', *, *, #51006, .F. ) ;
#43727 = ORIENTED_EDGE ( 'NONE', *, *, #25687, .F. ) ;
#43728 = DIRECTION ( 'NONE',  ( 0.000000000000000000, 1.000000000000000000, -0.000000000000000000 ) ) ;
#43729 = LINE ( 'NONE', #15624, #37567 ) ;
#43730 = ORIENTED_EDGE ( 'NONE', *, *, #19617, .F. ) ;
#43731 = LINE ( 'NONE', #15369, #14820 ) ;
#43732 = CARTESIAN_POINT ( 'NONE',  ( -336.3521761649654422, -100.1170788342122080, 54.23253582808833073 ) ) ;
#43733 = CARTESIAN_POINT ( 'NONE',  ( -330.4913330509368166, -66.09477493971917283, -13.63415328425296202 ) ) ;
#43734 = ORIENTED_EDGE ( 'NONE', *, *, #13065, .F. ) ;
#43735 = CARTESIAN_POINT ( 'NONE',  ( -74.51199343215203896, -193.5000000000000000, -122.2591094863194598 ) ) ;
#43736 = VERTEX_POINT ( 'NONE', #18934 ) ;
#43737 = DIRECTION ( 'NONE',  ( 1.000000000000000000, 0.000000000000000000, 0.000000000000000000 ) ) ;
#43738 = FACE_BOUND ( 'NONE', #36911, .T. ) ;
#43739 = CARTESIAN_POINT ( 'NONE',  ( -109.9568094315246327, -193.5000000000000000, -108.8370090194290611 ) ) ;
#43740 = ORIENTED_EDGE ( 'NONE', *, *, #3694, .T. ) ;
#43741 = CARTESIAN_POINT ( 'NONE',  ( -48.53836737940257251, -193.5000000000000000, 0.9982437317643279018 ) ) ;
#43742 = CARTESIAN_POINT ( 'NONE',  ( -162.9896759831413249, -193.5000000000000000, -50.12318939043961308 ) ) ;
#43743 = CARTESIAN_POINT ( 'NONE',  ( 60.58466639580034041, -193.5000000000000000, -61.07445476073405644 ) ) ;
#43744 = EDGE_CURVE ( 'NONE', #19552, #10747, #26942, .T. ) ;
#43745 = DIRECTION ( 'NONE',  ( 1.000000000000000000, -0.000000000000000000, -0.000000000000000000 ) ) ;
#43746 = VERTEX_POINT ( 'NONE', #15513 ) ;
#43747 = DIRECTION ( 'NONE',  ( 0.000000000000000000, 0.000000000000000000, -1.000000000000000000 ) ) ;
#43748 = VERTEX_POINT ( 'NONE', #4387 ) ;
#43749 = ORIENTED_EDGE ( 'NONE', *, *, #22922, .F. ) ;
#43750 = CARTESIAN_POINT ( 'NONE',  ( -56.05401443572774411, -193.5000000000000000, 124.7702732086912931 ) ) ;
#43752 = ORIENTED_EDGE ( 'NONE', *, *, #50761, .T. ) ;
#43751 = CARTESIAN_POINT ( 'NONE',  ( -49.30901192927175458, -193.5000000000000000, -124.9972451320097093 ) ) ;
#43753 = VECTOR ( 'NONE', #19577, 1000.000000000000000 ) ;
#43754 = VERTEX_POINT ( 'NONE', #20411 ) ;
#43755 = LINE ( 'NONE', #7757, #30501 ) ;
#43756 = VECTOR ( 'NONE', #18027, 1000.000000000000000 ) ;
#43757 = VECTOR ( 'NONE', #10602, 1000.000000000000114 ) ;
#43758 = DIRECTION ( 'NONE',  ( -0.000000000000000000, -0.6631226582407989678, -0.7485107481710977506 ) ) ;
#43759 = EDGE_LOOP ( 'NONE', ( #16512, #34581, #18695, #45841 ) ) ;
#43760 = FACE_BOUND ( 'NONE', #11638, .T. ) ;
#43761 = DIRECTION ( 'NONE',  ( 0.000000000000000000, -1.000000000000000000, 0.000000000000000000 ) ) ;
#43762 = EDGE_CURVE ( 'NONE', #15743, #7849, #27593, .T. ) ;
#43763 = ORIENTED_EDGE ( 'NONE', *, *, #49547, .F. ) ;
#43764 = CARTESIAN_POINT ( 'NONE',  ( 69.72248760683812918, -177.1207230881787780, -37.47770156625421833 ) ) ;
#43765 = LINE ( 'NONE', #12219, #38390 ) ;
#43766 = DIRECTION ( 'NONE',  ( 0.000000000000000000, -0.000000000000000000, 1.000000000000000000 ) ) ;
#43767 = DIRECTION ( 'NONE',  ( 0.000000000000000000, 0.000000000000000000, 1.000000000000000000 ) ) ;
#43768 = ORIENTED_EDGE ( 'NONE', *, *, #2080, .F. ) ;
#43769 = AXIS2_PLACEMENT_3D ( 'NONE', #19076, #31402, #31670 ) ;
#43770 = ORIENTED_EDGE ( 'NONE', *, *, #13771, .T. ) ;
#43771 = ORIENTED_EDGE ( 'NONE', *, *, #23469, .T. ) ;
#43772 = DIRECTION ( 'NONE',  ( 0.9646355819083576311, 0.000000000000000000, 0.2635871660690715101 ) ) ;
#43773 = DIRECTION ( 'NONE',  ( 0.000000000000000000, 0.000000000000000000, 1.000000000000000000 ) ) ;
#43774 = CIRCLE ( 'NONE', #51373, 125.0000000000000000 ) ;
#43775 = DIRECTION ( 'NONE',  ( 1.000000000000000000, 0.000000000000000000, 0.000000000000000000 ) ) ;
#43776 = FACE_OUTER_BOUND ( 'NONE', #31918, .T. ) ;
#43777 = LINE ( 'NONE', #15940, #30589 ) ;
#43778 = ORIENTED_EDGE ( 'NONE', *, *, #51534, .F. ) ;
#43779 = ADVANCED_FACE ( 'NONE', ( #31526 ), #16045, .T. ) ;
#43780 = CARTESIAN_POINT ( 'NONE',  ( -330.4913330509368166, -182.0095552316575152, 7.608018572113473432 ) ) ;
#43781 = ORIENTED_EDGE ( 'NONE', *, *, #33535, .T. ) ;
#43783 = ORIENTED_EDGE ( 'NONE', *, *, #42936, .F. ) ;
#43782 = CARTESIAN_POINT ( 'NONE',  ( -127.6327502296859535, -193.5000000000000000, -95.45105364470084908 ) ) ;
#43784 = EDGE_LOOP ( 'NONE', ( #30599, #16085, #163, #50312 ) ) ;
#43785 = EDGE_CURVE ( 'NONE', #11713, #49096, #7108, .T. ) ;
#43786 = LINE ( 'NONE', #154, #49316 ) ;
#43787 = CARTESIAN_POINT ( 'NONE',  ( -332.3517673607765914, -180.3949349376675855, 15.70448169564087770 ) ) ;
#43788 = VECTOR ( 'NONE', #12898, 1000.000000000000227 ) ;
#43789 = FACE_OUTER_BOUND ( 'NONE', #9041, .T. ) ;
#43790 = DIRECTION ( 'NONE',  ( 0.05924062789370006937, 0.000000000000000000, 0.9982437317643222396 ) ) ;
#43791 = ORIENTED_EDGE ( 'NONE', *, *, #34198, .T. ) ;
#43792 = CARTESIAN_POINT ( 'NONE',  ( -48.47912675150885065, -175.3837268820161057, 6.938893903907228378E-15 ) ) ;
#43793 = AXIS2_PLACEMENT_3D ( 'NONE', #49775, #46351, #26358 ) ;
#43794 = ORIENTED_EDGE ( 'NONE', *, *, #25634, .T. ) ;
#43795 = VECTOR ( 'NONE', #46049, 1000.000000000000114 ) ;
#43796 = EDGE_CURVE ( 'NONE', #2344, #14293, #35215, .T. ) ;
#43797 = EDGE_LOOP ( 'NONE', ( #9471, #43276, #24391, #10108 ) ) ;
#43798 = LINE ( 'NONE', #7799, #20381 ) ;
#43799 = DIRECTION ( 'NONE',  ( 1.000000000000000000, -8.465038975556420946E-17, -2.086444717177458678E-17 ) ) ;
#43800 = PLANE ( 'NONE',  #40695 ) ;
#43801 = DIRECTION ( 'NONE',  ( 0.000000000000000000, 0.000000000000000000, -1.000000000000000000 ) ) ;
#43802 = LINE ( 'NONE', #38825, #13658 ) ;
#43803 = EDGE_CURVE ( 'NONE', #17270, #50197, #14355, .T. ) ;
#43804 = EDGE_LOOP ( 'NONE', ( #1760, #20134, #50765, #11442 ) ) ;
#43805 = CARTESIAN_POINT ( 'NONE',  ( -332.3517673607765914, -85.72124494520284088, -46.61293454085073051 ) ) ;
#43806 = CARTESIAN_POINT ( 'NONE',  ( 75.04604393171729271, -189.7472609257535510, -10.84123789944573168 ) ) ;
#43807 = VECTOR ( 'NONE', #48685, 1000.000000000000000 ) ;
#43808 = FACE_BOUND ( 'NONE', #32200, .T. ) ;
#43809 = ORIENTED_EDGE ( 'NONE', *, *, #42798, .T. ) ;
#43810 = AXIS2_PLACEMENT_3D ( 'NONE', #14245, #9777, #22376 ) ;
#43811 = ADVANCED_FACE ( 'NONE', ( #16484 ), #51267, .T. ) ;
#43812 = CIRCLE ( 'NONE', #1878, 60.00000000000000000 ) ;
#43813 = DIRECTION ( 'NONE',  ( -0.000000000000000000, 1.000000000000000000, 0.000000000000000000 ) ) ;
#43814 = CARTESIAN_POINT ( 'NONE',  ( 75.02564229359539638, -189.7472609257535510, -19.27620354518635182 ) ) ;
#43815 = EDGE_LOOP ( 'NONE', ( #37633, #10615, #5332, #11374, #31003, #44721, #3002, #26180, #44154, #11785, #1838, #39300, #1700, #48317, #28572, #47235, #40542, #19909 ) ) ;
#43816 = DIRECTION ( 'NONE',  ( 0.8757349421956412971, 0.000000000000000000, -0.4827922027307366970 ) ) ;
#43817 = ORIENTED_EDGE ( 'NONE', *, *, #43642, .F. ) ;
#43818 = CARTESIAN_POINT ( 'NONE',  ( -134.9506378406916554, -189.7472609257535510, 90.26448786734091811 ) ) ;
#43819 = FACE_BOUND ( 'NONE', #45333, .T. ) ;
#43821 = ORIENTED_EDGE ( 'NONE', *, *, #48754, .T. ) ;
#43820 = DIRECTION ( 'NONE',  ( -0.8455960035018234011, 0.000000000000000000, -0.5338233779647948429 ) ) ;
#43822 = EDGE_CURVE ( 'NONE', #45007, #19578, #47061, .T. ) ;
#43823 = VECTOR ( 'NONE', #10192, 1000.000000000000000 ) ;
#43824 = CARTESIAN_POINT ( 'NONE',  ( -305.0000000000000568, -63.50208336950359467, 0.4999999999999573119 ) ) ;
#43825 = EDGE_LOOP ( 'NONE', ( #16122, #6911, #17320, #50159 ) ) ;
#43826 = EDGE_LOOP ( 'NONE', ( #35804, #32631, #15224, #37970 ) ) ;
#43827 = CARTESIAN_POINT ( 'NONE',  ( -180.0000000000000568, -115.7896721143442278, 60.00000000000000711 ) ) ;
#43828 = ORIENTED_EDGE ( 'NONE', *, *, #40112, .T. ) ;
#43829 = DIRECTION ( 'NONE',  ( 0.000000000000000000, -1.000000000000000000, -0.000000000000000000 ) ) ;
#43830 = CARTESIAN_POINT ( 'NONE',  ( -48.02249751411514467, -193.5000000000000000, 0.8896570909947569827 ) ) ;
#43831 = CIRCLE ( 'NONE', #19495, 125.0000000000000000 ) ;
#43832 = VECTOR ( 'NONE', #21112, 1000.000000000000000 ) ;
#43833 = CARTESIAN_POINT ( 'NONE',  ( -336.3521761649654422, -88.64083255475578937, 47.62880233550460218 ) ) ;
#43834 = CARTESIAN_POINT ( 'NONE',  ( -157.8637630444124795, -175.3837268820161057, -60.49794494914009135 ) ) ;
#43835 = ORIENTED_EDGE ( 'NONE', *, *, #37705, .T. ) ;
#43838 = ORIENTED_EDGE ( 'NONE', *, *, #20080, .T. ) ;
#43837 = CARTESIAN_POINT ( 'NONE',  ( -106.4764934152196645, -213.5000000000000000, 110.7307791902283043 ) ) ;
#43836 = LINE ( 'NONE', #27291, #9908 ) ;
#43839 = CIRCLE ( 'NONE', #51408, 124.9999999999999858 ) ;
#43840 = VECTOR ( 'NONE', #50752, 1000.000000000000000 ) ;
#43841 = EDGE_LOOP ( 'NONE', ( #44716, #18223, #19556, #34242 ) ) ;
#43842 = DIRECTION ( 'NONE',  ( -0.9785564922995017012, 0.000000000000000000, -0.2059786187411094538 ) ) ;
#43843 = ORIENTED_EDGE ( 'NONE', *, *, #10879, .T. ) ;
#43844 = CARTESIAN_POINT ( 'NONE',  ( -336.3521761649654422, -170.5607375887735770, 35.68215131113770155 ) ) ;
#43845 = VERTEX_POINT ( 'NONE', #51515 ) ;
#43846 = EDGE_CURVE ( 'NONE', #34815, #31384, #39409, .T. ) ;
#43847 = EDGE_CURVE ( 'NONE', #24293, #21281, #41199, .T. ) ;
#43848 = CLOSED_SHELL ( 'NONE', ( #14761, #40148, #4407, #3264, #18551, #4535, #43307, #17841, #5383, #46806, #26903, #6095, #23828, #39996, #36059, #5738, #34898, #907, #1709, #10231, #16047, #3773, #29156, #33314, #10919, #33123, #18435, #9635, #40590, #16668, #740, #4807, #23347, #19197, #40918, #38982, #20063, #18163, #34953, #20885, #38120, #21868, #38033, #13969, #33674, #49422, #25642, #11997, #30904, #29884, #29215, #3000, #17071, #40722, #49748, #30695, #21152, #16707, #37805, #9009, #27306, #39697, #20902, #8508, #41613, #49405, #18928, #21806, #33840, #16437, #5736, #49450, #49156, #34029, #18882, #3120, #43939, #49262, #20377, #33405, #29565, #46970, #41115, #44965, #29753, #12544, #34973, #7425, #539, #11361, #47730, #28731, #18948, #28744, #42320, #31132, #50077, #34077, #28199, #8269, #6150, #34024, #2823, #42506, #41827, #18265, #9812, #13113, #39923, #41974, #51369, #27542, #39051, #36737, #23683, #47906, #48370, #22385, #8608, #20151, #9652, #26825, #19317, #6089, #11159, #51018, #17190, #10292, #7991, #35117, #8592, #42265, #6747, #48438, #4416, #34343, #22134, #36193, #46394, #13662, #39280, #2406, #43909, #47645, #27258, #44060, #27713, #36191, #39194, #49746, #2537, #43868, #25485, #10814, #6915, #5461, #14036, #9192, #2004, #18890, #20671, #29748, #50758, #48925, #28432, #3416, #46610, #48514, #15035, #51969, #31448, #12452, #10920, #26360, #49841, #43363, #30812, #49409, #23930, #44314, #13072, #9290, #20181, #25538, #48736, #41236, #8338, #7034, #22699, #12792, #31410, #49408, #46314, #4344, #26844, #2473, #32875, #10233, #19081, #38902, #16646, #931, #35650, #36632, #34099, #47085, #23061, #44279, #144, #40792, #4404, #19602, #8966, #15765, #1979, #13157, #19442, #44290, #24052, #7834, #9466, #31127, #184, #15010, #14033, #22386, #2413, #28540, #49089, #14049, #33623, #36323, #21798, #24696, #41901, #26607, #27637, #36573, #30747, #47560, #2164, #13779, #37406, #19762, #32176, #41617, #45677, #43626, #36601, #21575, #15860, #35975, #9286, #24713, #33807, #46891, #3311, #31800, #2811, #44527, #25072, #36081, #43931, #27546, #36221, #50303, #8134, #15799, #48636, #29999, #6898, #47022, #5762, #24373, #41738, #3007, #9703, #2885, #32162, #37724, #11466, #4029, #21682, #14339, #18816, #21748, #1607, #6097, #6576, #3465, #1283, #1859, #28343, #45919, #38116, #18615, #9947, #50467, #15443, #23037, #12357, #47704, #6903, #44703, #34693, #29473, #11301, #36873, #18892, #14137, #135, #37584, #24711, #34620, #46551, #2518, #5918, #23258, #50343, #6380, #3474, #45370, #41915, #27026, #3964, #16999, #29676, #2286, #32793, #7941, #10309, #29668, #40356, #538, #50047, #2859, #20532, #3826, #18829, #18622, #42375, #51423, #40300, #13754, #16029, #1868, #27886, #2168, #35733, #27887, #28492, #39656, #25073, #11522, #38743, #49346, #13398, #1750, #33029, #41868, #12061, #21446, #24946, #51800, #41717, #14381, #49416, #41090, #1948, #33063, #24535, #38479, #42180, #28480, #38646, #30990, #46704, #38423, #7909, #49123, #15014, #14819, #16539, #12890, #47146, #38850, #37342, #34482, #52028, #17947, #198, #22736, #5390, #21226, #11869, #13805, #50182, #31763, #21458, #23633, #15534, #19849, #35477, #50585, #47265, #46195, #13796, #13493, #40696, #5457, #9783, #26041, #50498, #26824, #15326, #30456, #40201, #47488, #17043, #38509, #34215, #36824, #43689, #42876, #35537, #21206, #37101, #29949, #49306, #24297, #41135, #23035, #51705, #46217, #46737, #3662, #982, #24640, #32670, #48798, #34625, #51062, #1327, #32734, #24131, #44581, #26379, #45554, #46255, #18336, #51686, #12292, #13345, #3865, #39477, #48075, #20854, #9602, #32407, #47382, #15714, #8222, #46151, #17250, #37587, #33896, #17597, #28196, #25716, #19526, #5071, #43095, #25233, #16174, #17142, #16511, #34465, #23422, #26772, #44764, #50787, #21542, #13749, #33989, #20607, #25300, #48734, #5222, #41408, #24369, #1091, #8365, #12504, #36947, #30224, #16007, #6391, #51736, #30818, #29004, #27784, #34206, #45079, #38842, #45772, #7229, #4993, #33086, #33718, #50003, #20247, #44645, #45402, #35848, #47745, #3388, #20440, #42700, #27862, #44288, #47133, #1856, #16604, #1259, #36555, #51308, #14592, #21142, #46187, #43664, #50416, #37873, #1531, #38221, #1202, #13744, #51964, #21272, #36444, #31852, #18776, #17019, #12477, #28419 ) ) ;
#43849 = DIRECTION ( 'NONE',  ( -0.000000000000000000, 0.7485107481710999711, -0.6631226582407964143 ) ) ;
#43850 = VERTEX_POINT ( 'NONE', #10526 ) ;
#43852 = DIRECTION ( 'NONE',  ( -0.5085311186492154079, 0.000000000000000000, -0.8610436117673585521 ) ) ;
#43851 = DIRECTION ( 'NONE',  ( -0.000000000000000000, 1.000000000000000000, -0.000000000000000000 ) ) ;
#43853 = VERTEX_POINT ( 'NONE', #42843 ) ;
#43854 = CARTESIAN_POINT ( 'NONE',  ( -121.8391548840036620, -183.6283474603465606, -99.97252634603250954 ) ) ;
#43855 = ORIENTED_EDGE ( 'NONE', *, *, #32956, .F. ) ;
#43856 = FACE_OUTER_BOUND ( 'NONE', #3583, .T. ) ;
#43857 = DIRECTION ( 'NONE',  ( -0.000000000000000000, 1.000000000000000000, 0.000000000000000000 ) ) ;
#43858 = DIRECTION ( 'NONE',  ( -0.000000000000000000, 1.000000000000000000, -0.000000000000000000 ) ) ;
#43859 = PLANE ( 'NONE',  #36723 ) ;
#43860 = PLANE ( 'NONE',  #20733 ) ;
#43861 = CIRCLE ( 'NONE', #1058, 20.00000000000001776 ) ;
#43862 = DIRECTION ( 'NONE',  ( 0.000000000000000000, 0.000000000000000000, -1.000000000000000000 ) ) ;
#43863 = VERTEX_POINT ( 'NONE', #6849 ) ;
#43864 = DIRECTION ( 'NONE',  ( 0.7110288200941177195, 4.405623073809627828E-17, 0.7031628666216435120 ) ) ;
#43865 = ADVANCED_FACE ( 'NONE', ( #34950 ), #47583, .T. ) ;
#43866 = CARTESIAN_POINT ( 'NONE',  ( 43.63512310656542326, -193.5000000000000000, 84.49831343337136502 ) ) ;
#43867 = CARTESIAN_POINT ( 'NONE',  ( 18.00181100848376303, -193.5000000000000000, -105.8550183720733742 ) ) ;
#43868 = ADVANCED_FACE ( 'NONE', ( #42592 ), #38641, .F. ) ;
#43869 = AXIS2_PLACEMENT_3D ( 'NONE', #18945, #46554, #10539 ) ;
#43870 = CARTESIAN_POINT ( 'NONE',  ( -339.1964088526558498, -90.39567187580801999, 48.84008046109089918 ) ) ;
#43871 = ORIENTED_EDGE ( 'NONE', *, *, #23986, .T. ) ;
#43872 = EDGE_CURVE ( 'NONE', #21582, #38978, #2607, .T. ) ;
#43873 = CARTESIAN_POINT ( 'NONE',  ( -336.3521761649654422, -181.7525362123217292, 9.724760635742144999 ) ) ;
#43874 = EDGE_CURVE ( 'NONE', #14462, #31403, #24613, .T. ) ;
#43875 = LINE ( 'NONE', #45206, #50455 ) ;
#43876 = DIRECTION ( 'NONE',  ( 1.000000000000000000, -0.000000000000000000, 0.000000000000000000 ) ) ;
#43877 = ORIENTED_EDGE ( 'NONE', *, *, #45845, .F. ) ;
#43878 = ORIENTED_EDGE ( 'NONE', *, *, #23126, .T. ) ;
#43879 = AXIS2_PLACEMENT_3D ( 'NONE', #35211, #27322, #3160 ) ;
#43880 = EDGE_LOOP ( 'NONE', ( #591, #16990, #10191, #45778 ) ) ;
#43881 = VECTOR ( 'NONE', #51998, 1000.000000000000000 ) ;
#43882 = VECTOR ( 'NONE', #1288, 1000.000000000000000 ) ;
#43883 = CARTESIAN_POINT ( 'NONE',  ( -148.6149069237406195, -177.1207230881787780, -74.81861753132353954 ) ) ;
#43884 = CIRCLE ( 'NONE', #41370, 4.999999999999997335 ) ;
#43885 = DIRECTION ( 'NONE',  ( 0.5085311186492154079, 0.000000000000000000, 0.8610436117673585521 ) ) ;
#43886 = LINE ( 'NONE', #3955, #2757 ) ;
#43887 = CARTESIAN_POINT ( 'NONE',  ( -161.2555905272864436, -175.3837268820161057, -53.91167979418489864 ) ) ;
#43888 = ORIENTED_EDGE ( 'NONE', *, *, #19626, .F. ) ;
#43889 = AXIS2_PLACEMENT_3D ( 'NONE', #36385, #27469, #12475 ) ;
#43890 = CARTESIAN_POINT ( 'NONE',  ( 3.877854670627010947, 56.07043499712327872, -17.37938424498008771 ) ) ;
#43891 = ORIENTED_EDGE ( 'NONE', *, *, #8331, .F. ) ;
#43892 = ORIENTED_EDGE ( 'NONE', *, *, #31110, .F. ) ;
#43893 = ORIENTED_EDGE ( 'NONE', *, *, #12827, .T. ) ;
#43894 = DIRECTION ( 'NONE',  ( -0.000000000000000000, 1.000000000000000000, -0.000000000000000000 ) ) ;
#43895 = VECTOR ( 'NONE', #23515, 1000.000000000000000 ) ;
#43896 = ORIENTED_EDGE ( 'NONE', *, *, #29045, .F. ) ;
#43897 = AXIS2_PLACEMENT_3D ( 'NONE', #8466, #32648, #28687 ) ;
#43898 = LINE ( 'NONE', #23925, #23463 ) ;
#43899 = CARTESIAN_POINT ( 'NONE',  ( -339.1964088526558498, -123.5000000000000284, 0.000000000000000000 ) ) ;
#43902 = ORIENTED_EDGE ( 'NONE', *, *, #16338, .T. ) ;
#43901 = DIRECTION ( 'NONE',  ( -0.000000000000000000, -0.000000000000000000, -1.000000000000000000 ) ) ;
#43900 = CARTESIAN_POINT ( 'NONE',  ( -89.73513343757494454, -193.5000000000000000, -117.9955164924467397 ) ) ;
#43903 = DIRECTION ( 'NONE',  ( 1.000000000000000000, -0.000000000000000000, -0.000000000000000000 ) ) ;
#43904 = ORIENTED_EDGE ( 'NONE', *, *, #4162, .F. ) ;
#43905 = CARTESIAN_POINT ( 'NONE',  ( -339.1964088526558498, -79.66942718702553350, -39.49849221029258928 ) ) ;
#43906 = ORIENTED_EDGE ( 'NONE', *, *, #17181, .T. ) ;
#43907 = EDGE_CURVE ( 'NONE', #18747, #43197, #714, .T. ) ;
#43908 = EDGE_CURVE ( 'NONE', #16384, #38633, #4648, .T. ) ;
#43909 = ADVANCED_FACE ( 'NONE', ( #49326 ), #25403, .F. ) ;
#43910 = CARTESIAN_POINT ( 'NONE',  ( 32.34187644556187280, -175.3837268820161057, 94.04236105995857997 ) ) ;
#43911 = DIRECTION ( 'NONE',  ( 0.000000000000000000, -0.8854560256532079121, 0.4647231720437725033 ) ) ;
#43913 = CARTESIAN_POINT ( 'NONE',  ( -77.77032474405881146, -193.5000000000000000, 120.4907712303052989 ) ) ;
#43912 = CARTESIAN_POINT ( 'NONE',  ( -50.89116676070551648, -193.5000000000000000, 124.9767260852757147 ) ) ;
#43914 = VECTOR ( 'NONE', #23184, 999.9999999999998863 ) ;
#43915 = ORIENTED_EDGE ( 'NONE', *, *, #24633, .T. ) ;
#43916 = EDGE_CURVE ( 'NONE', #34663, #28107, #37907, .T. ) ;
#43917 = LINE ( 'NONE', #7427, #19786 ) ;
#43918 = AXIS2_PLACEMENT_3D ( 'NONE', #22013, #42498, #6521 ) ;
#43919 = PLANE ( 'NONE',  #36244 ) ;
#43920 = ORIENTED_EDGE ( 'NONE', *, *, #31193, .T. ) ;
#43921 = ADVANCED_FACE ( 'NONE', ( #21723 ), #20675, .T. ) ;
#43922 =( NAMED_UNIT ( * ) PLANE_ANGLE_UNIT ( ) SI_UNIT ( $, .RADIAN. ) );
#43923 = DIRECTION ( 'NONE',  ( -0.000000000000000000, 1.000000000000000000, -0.000000000000000000 ) ) ;
#43924 = EDGE_CURVE ( 'NONE', #12141, #36143, #48809, .T. ) ;
#43925 = FACE_OUTER_BOUND ( 'NONE', #5299, .T. ) ;
#43926 = ORIENTED_EDGE ( 'NONE', *, *, #33069, .F. ) ;
#43927 = DIRECTION ( 'NONE',  ( 0.000000000000000000, -1.000000000000000000, -0.000000000000000000 ) ) ;
#43928 = VECTOR ( 'NONE', #37749, 1000.000000000000114 ) ;
#43929 = EDGE_CURVE ( 'NONE', #41184, #23109, #40392, .T. ) ;
#43930 = FACE_OUTER_BOUND ( 'NONE', #12148, .T. ) ;
#43931 = ADVANCED_FACE ( 'NONE', ( #45385 ), #29066, .F. ) ;
#43932 = ORIENTED_EDGE ( 'NONE', *, *, #35692, .T. ) ;
#43933 = LINE ( 'NONE', #11093, #3100 ) ;
#43934 = ORIENTED_EDGE ( 'NONE', *, *, #46194, .F. ) ;
#43935 = EDGE_CURVE ( 'NONE', #43203, #9007, #36967, .T. ) ;
#43936 = CARTESIAN_POINT ( 'NONE',  ( -136.1415351158078693, -189.7472609257535510, -89.10837311819173578 ) ) ;
#43937 = CARTESIAN_POINT ( 'NONE',  ( -59.28786813212838069, -177.1207230881787780, 124.5318076226587323 ) ) ;
#43938 = VECTOR ( 'NONE', #32503, 1000.000000000000114 ) ;
#43939 = ADVANCED_FACE ( 'NONE', ( #44593 ), #45644, .F. ) ;
#43940 = DIRECTION ( 'NONE',  ( -1.000000000000000000, 0.000000000000000000, 0.000000000000000000 ) ) ;
#43941 = LINE ( 'NONE', #20282, #39016 ) ;
#43942 = CARTESIAN_POINT ( 'NONE',  ( -336.3521761649654422, -106.8245764869328980, 56.65561927337994064 ) ) ;
#43943 = AXIS2_PLACEMENT_3D ( 'NONE', #1642, #5063, #49726 ) ;
#43944 = DIRECTION ( 'NONE',  ( -0.05924062789371441901, 0.000000000000000000, 0.9982437317643214625 ) ) ;
#43945 = FACE_OUTER_BOUND ( 'NONE', #49618, .T. ) ;
#43946 = CARTESIAN_POINT ( 'NONE',  ( 43.33156026654913262, 30.00000000000000355, -51.04247435516399634 ) ) ;
#43948 = ORIENTED_EDGE ( 'NONE', *, *, #12163, .T. ) ;
#43947 = PLANE ( 'NONE',  #8539 ) ;
#43949 = ORIENTED_EDGE ( 'NONE', *, *, #14775, .T. ) ;
#43950 = PLANE ( 'NONE',  #29116 ) ;
#43951 = AXIS2_PLACEMENT_3D ( 'NONE', #46830, #36203, #44375 ) ;
#43952 = EDGE_CURVE ( 'NONE', #809, #23381, #5174, .T. ) ;
#43953 = DIRECTION ( 'NONE',  ( 0.000000000000000000, 0.000000000000000000, 1.000000000000000000 ) ) ;
#43954 = ORIENTED_EDGE ( 'NONE', *, *, #48812, .T. ) ;
#43955 = EDGE_LOOP ( 'NONE', ( #26575, #28696, #4835, #2703 ) ) ;
#43956 = ORIENTED_EDGE ( 'NONE', *, *, #23303, .F. ) ;
#43957 = DIRECTION ( 'NONE',  ( -8.718379230999707126E-17, 0.2393156642875516604, -0.9709418174260535661 ) ) ;
#43958 = PLANE ( 'NONE',  #51872 ) ;
#43959 = CARTESIAN_POINT ( 'NONE',  ( 0.000000000000000000, -109.3803758070334737, 57.28556722813694080 ) ) ;
#43960 = LINE ( 'NONE', #27413, #13206 ) ;
#43961 = VERTEX_POINT ( 'NONE', #40899 ) ;
#43962 = ORIENTED_EDGE ( 'NONE', *, *, #15882, .F. ) ;
#43963 = ORIENTED_EDGE ( 'NONE', *, *, #46090, .F. ) ;
#43964 = EDGE_CURVE ( 'NONE', #775, #26963, #10182, .T. ) ;
#43965 = CARTESIAN_POINT ( 'NONE',  ( -336.3521761649654422, -65.58448481710581746, 11.56382487286456140 ) ) ;
#43966 = CARTESIAN_POINT ( 'NONE',  ( -332.3517673607765914, -182.2665742509934148, -5.491276508484069119 ) ) ;
#43967 = CARTESIAN_POINT ( 'NONE',  ( -330.4913330509368166, -178.8432607619609200, -20.45418021416661247 ) ) ;
#43968 = DIRECTION ( 'NONE',  ( -0.000000000000000000, 1.000000000000000000, -0.000000000000000000 ) ) ;
#43969 = CARTESIAN_POINT ( 'NONE',  ( -339.1964088526558498, -172.3400804610915600, -33.10432812419107051 ) ) ;
#43970 = AXIS2_PLACEMENT_3D ( 'NONE', #12260, #28546, #7807 ) ;
#43971 = EDGE_LOOP ( 'NONE', ( #25270, #22094, #17153, #25986 ) ) ;
#43972 = FACE_OUTER_BOUND ( 'NONE', #21127, .T. ) ;
#43973 = CIRCLE ( 'NONE', #41459, 125.0000000000000000 ) ;
#43974 = EDGE_CURVE ( 'NONE', #49096, #36522, #45132, .T. ) ;
#43975 = EDGE_CURVE ( 'NONE', #9933, #17165, #41163, .T. ) ;
#43976 = EDGE_CURVE ( 'NONE', #20460, #21321, #17265, .T. ) ;
#43977 = LINE ( 'NONE', #16391, #3934 ) ;
#43978 = CARTESIAN_POINT ( 'NONE',  ( 23.54917025746143011, -183.6283474603465606, -100.9358816284410665 ) ) ;
#43979 = CARTESIAN_POINT ( 'NONE',  ( -336.3521761649654422, -176.9651911376907094, -25.08789112700655721 ) ) ;
#43980 = AXIS2_PLACEMENT_3D ( 'NONE', #49581, #41157, #17260 ) ;
#43981 = EDGE_CURVE ( 'NONE', #27241, #49313, #5441, .T. ) ;
#43982 = ORIENTED_EDGE ( 'NONE', *, *, #17309, .F. ) ;
#43983 = VERTEX_POINT ( 'NONE', #25651 ) ;
#43984 = VERTEX_POINT ( 'NONE', #1486 ) ;
#43985 = CARTESIAN_POINT ( 'NONE',  ( -339.1964088526558498, -151.3613951634092700, -52.00954392751739164 ) ) ;
#43986 = CARTESIAN_POINT ( 'NONE',  ( -170.9669310976187830, -193.5000000000000000, -24.93467037017130394 ) ) ;
#43987 = ORIENTED_EDGE ( 'NONE', *, *, #30844, .T. ) ;
#43988 = DIRECTION ( 'NONE',  ( -1.000000000000000000, -0.000000000000000000, 0.000000000000000000 ) ) ;
#43989 = DIRECTION ( 'NONE',  ( -1.000000000000000000, 0.000000000000000000, -0.000000000000000000 ) ) ;
#43990 = PLANE ( 'NONE',  #23447 ) ;
#43991 = ORIENTED_EDGE ( 'NONE', *, *, #13010, .T. ) ;
#43992 = FACE_OUTER_BOUND ( 'NONE', #11603, .T. ) ;
#43993 = AXIS2_PLACEMENT_3D ( 'NONE', #30084, #6702, #1969 ) ;
#43994 = ORIENTED_EDGE ( 'NONE', *, *, #28772, .F. ) ;
#43995 = CARTESIAN_POINT ( 'NONE',  ( -48.13092511607445800, -177.1207230881787780, 0.9374196611341301111 ) ) ;
#43996 = ORIENTED_EDGE ( 'NONE', *, *, #46971, .F. ) ;
#43997 = DIRECTION ( 'NONE',  ( 0.000000000000000000, 0.000000000000000000, 1.000000000000000000 ) ) ;
#43998 = EDGE_CURVE ( 'NONE', #12404, #46929, #29591, .T. ) ;
#43999 = DIRECTION ( 'NONE',  ( -0.000000000000000000, 1.000000000000000000, -0.000000000000000000 ) ) ;
#44000 = ORIENTED_EDGE ( 'NONE', *, *, #46933, .T. ) ;
#44001 = EDGE_CURVE ( 'NONE', #39339, #38101, #33795, .T. ) ;
#44002 = CARTESIAN_POINT ( 'NONE',  ( -8.461066480258370603, -193.5000000000000000, 117.3655938605930231 ) ) ;
#44003 = CARTESIAN_POINT ( 'NONE',  ( -41.90263914168912152, -189.7472609257535510, -124.8268793598473536 ) ) ;
#44004 = CARTESIAN_POINT ( 'NONE',  ( -339.1964088526558498, -162.9117225908391333, -45.24064679492040142 ) ) ;
#44005 = CARTESIAN_POINT ( 'NONE',  ( -47.70260288879080690, -193.5000000000000000, -0.6300878435817026668 ) ) ;
#44006 = EDGE_CURVE ( 'NONE', #2225, #48882, #3027, .T. ) ;
#44007 = EDGE_LOOP ( 'NONE', ( #36100, #42427, #36383, #22540 ) ) ;
#44008 = CARTESIAN_POINT ( 'NONE',  ( -336.3521761649654422, -69.26746417191145611, -23.38292116578723068 ) ) ;
#44009 = ORIENTED_EDGE ( 'NONE', *, *, #12355, .T. ) ;
#44010 = ORIENTED_EDGE ( 'NONE', *, *, #26326, .F. ) ;
#44011 = DIRECTION ( 'NONE',  ( 0.000000000000000000, -0.1205366802553095168, 0.9927088740980556381 ) ) ;
#44013 = ORIENTED_EDGE ( 'NONE', *, *, #13788, .T. ) ;
#44012 = DIRECTION ( 'NONE',  ( 0.000000000000000000, 1.000000000000000000, 0.000000000000000000 ) ) ;
#44014 = VECTOR ( 'NONE', #26017, 1000.000000000000114 ) ;
#44015 = B_SPLINE_CURVE_WITH_KNOTS ( 'NONE', 3,
 ( #908, #18181, #34208, #3684, #43638, #43388, #16050, #11, #31816, #27079, #47075, #19713, #39175, #11824, #27853, #35743, #39671, #47854, #32058, #19983, #7885, #2916, #43890, #23914, #3428, #19456, #35480, #7395, #35229, #31285, #39931, #3959, #23418, #7637 ),
 .UNSPECIFIED., .F., .F.,
 ( 4, 2, 2, 2, 2, 2, 2, 2, 2, 2, 2, 2, 2, 2, 2, 2, 4 ),
 ( 0.004374701946809896047, 0.005252622471382774154, 0.006130542995955652261, 0.007008463520528530367, 0.007886384045101408474, 0.008764304569674287448, 0.009642225094247164688, 0.01052014561882004193, 0.01139806614339292090, 0.01227598666796579988, 0.01315390719253867712, 0.01403182771711155435, 0.01490974824168443333, 0.01578766876625731230, 0.01666558929083018781, 0.01754350981540306678, 0.01842143033997594576 ),
 .UNSPECIFIED. ) ;
#44016 = VERTEX_POINT ( 'NONE', #10921 ) ;
#44017 = LINE ( 'NONE', #36656, #38275 ) ;
#44018 = AXIS2_PLACEMENT_3D ( 'NONE', #50608, #10658, #26690 ) ;
#44019 = ADVANCED_FACE ( 'NONE', ( #1994 ), #26694, .T. ) ;
#44020 = CARTESIAN_POINT ( 'NONE',  ( -336.3521761649654422, -81.08339623743702873, -41.09453333279329712 ) ) ;
#44021 = ORIENTED_EDGE ( 'NONE', *, *, #7857, .F. ) ;
#44022 = CARTESIAN_POINT ( 'NONE',  ( -336.3521761649654422, -159.1821513111375452, -47.06073758877369073 ) ) ;
#44023 = DIRECTION ( 'NONE',  ( 0.000000000000000000, 0.000000000000000000, 1.000000000000000000 ) ) ;
#44024 = VERTEX_POINT ( 'NONE', #34060 ) ;
#44025 = DIRECTION ( 'NONE',  ( 0.000000000000000000, 0.000000000000000000, 1.000000000000000000 ) ) ;
#44026 = CARTESIAN_POINT ( 'NONE',  ( -332.3517673607765914, -153.2494431741581025, -51.01861988938816950 ) ) ;
#44028 = AXIS2_PLACEMENT_3D ( 'NONE', #46840, #50006, #14261 ) ;
#44027 = DIRECTION ( 'NONE',  ( 1.000000000000000000, -0.000000000000000000, 0.000000000000000000 ) ) ;
#44029 = PLANE ( 'NONE',  #14871 ) ;
#44030 = ORIENTED_EDGE ( 'NONE', *, *, #13019, .T. ) ;
#44031 = ORIENTED_EDGE ( 'NONE', *, *, #44885, .F. ) ;
#44032 = ORIENTED_EDGE ( 'NONE', *, *, #39909, .F. ) ;
#44033 = PLANE ( 'NONE',  #43390 ) ;
#44034 = LINE ( 'NONE', #11717, #48662 ) ;
#44035 = CARTESIAN_POINT ( 'NONE',  ( 22.03849146056077757, -193.5000000000000000, 103.2098131075567409 ) ) ;
#44036 = FACE_BOUND ( 'NONE', #49121, .T. ) ;
#44037 = DIRECTION ( 'NONE',  ( 0.000000000000000000, -0.3546048870425426158, -0.9350162426854120579 ) ) ;
#44038 = ORIENTED_EDGE ( 'NONE', *, *, #32339, .T. ) ;
#44039 = EDGE_CURVE ( 'NONE', #32740, #34582, #6980, .T. ) ;
#44040 = EDGE_CURVE ( 'NONE', #27293, #2653, #34814, .T. ) ;
#44041 = CARTESIAN_POINT ( 'NONE',  ( 68.93474881819258826, -193.5000000000000000, 39.87457906003773900 ) ) ;
#44042 = EDGE_LOOP ( 'NONE', ( #31809, #3127, #24213, #31677 ) ) ;
#44044 = ORIENTED_EDGE ( 'NONE', *, *, #20547, .T. ) ;
#44043 = DIRECTION ( 'NONE',  ( -0.000000000000000000, 1.000000000000000000, -0.000000000000000000 ) ) ;
#44045 = ORIENTED_EDGE ( 'NONE', *, *, #20646, .F. ) ;
#44046 = CIRCLE ( 'NONE', #50776, 125.0000000000000000 ) ;
#44047 = CARTESIAN_POINT ( 'NONE',  ( -165.7578939544008847, -183.6283474603465606, -43.25148278810625868 ) ) ;
#44048 = CARTESIAN_POINT ( 'NONE',  ( 68.21542617880035664, -183.6283474603465606, 41.93543928473692262 ) ) ;
#44049 = VECTOR ( 'NONE', #27950, 1000.000000000000000 ) ;
#44050 = AXIS2_PLACEMENT_3D ( 'NONE', #10721, #38823, #29910 ) ;
#44051 = CARTESIAN_POINT ( 'NONE',  ( -339.1964088526558498, -151.3613951634084742, 52.00954392751779665 ) ) ;
#44052 = LINE ( 'NONE', #5164, #43548 ) ;
#44053 = ORIENTED_EDGE ( 'NONE', *, *, #36918, .T. ) ;
#44054 = CARTESIAN_POINT ( 'NONE',  ( -49.35486169370448550, -183.6283474603465606, -0.4827922027307481878 ) ) ;
#44055 = ORIENTED_EDGE ( 'NONE', *, *, #47731, .T. ) ;
#44056 = VECTOR ( 'NONE', #19506, 1000.000000000000000 ) ;
#44057 = ORIENTED_EDGE ( 'NONE', *, *, #17952, .T. ) ;
#44058 = CARTESIAN_POINT ( 'NONE',  ( -180.0000000000000568, -155.0173647354142759, 14.76740078976490622 ) ) ;
#44060 = ADVANCED_FACE ( 'NONE', ( #18037 ), #13834, .F. ) ;
#44059 = VECTOR ( 'NONE', #29690, 1000.000000000000000 ) ;
#44061 = FACE_OUTER_BOUND ( 'NONE', #9847, .T. ) ;
#44062 = PLANE ( 'NONE',  #18997 ) ;
#44063 = AXIS2_PLACEMENT_3D ( 'NONE', #665, #31932, #4599 ) ;
#44064 = CARTESIAN_POINT ( 'NONE',  ( -123.6678354051270077, -175.3837268820161057, 99.85818990449067201 ) ) ;
#44065 = CYLINDRICAL_SURFACE ( 'NONE', #19639, 125.0000000000000000 ) ;
#44066 = CARTESIAN_POINT ( 'NONE',  ( -40.24578378811990831, -193.5000000000000000, 124.7285535218268251 ) ) ;
#44067 = VERTEX_POINT ( 'NONE', #2267 ) ;
#44068 = AXIS2_PLACEMENT_3D ( 'NONE', #22141, #46074, #17695 ) ;
#44069 = FACE_OUTER_BOUND ( 'NONE', #16921, .T. ) ;
#44070 = DIRECTION ( 'NONE',  ( 0.000000000000000000, -1.000000000000000000, -0.000000000000000000 ) ) ;
#44071 = EDGE_CURVE ( 'NONE', #19790, #18653, #30894, .T. ) ;
#44072 = AXIS2_PLACEMENT_3D ( 'NONE', #12026, #462, #28056 ) ;
#44073 = FACE_BOUND ( 'NONE', #27138, .T. ) ;
#44074 = VERTEX_POINT ( 'NONE', #42972 ) ;
#44075 = DIRECTION ( 'NONE',  ( -0.000000000000000000, 0.2393156642875448881, -0.9709418174260553425 ) ) ;
#44076 = DIRECTION ( 'NONE',  ( 0.000000000000000000, 0.000000000000000000, 1.000000000000000000 ) ) ;
#44077 = ORIENTED_EDGE ( 'NONE', *, *, #47159, .F. ) ;
#44078 = CARTESIAN_POINT ( 'NONE',  ( 75.46126020185813843, -175.3837268820161057, 3.844569333773209419 ) ) ;
#44079 = ORIENTED_EDGE ( 'NONE', *, *, #20009, .F. ) ;
#44080 = DIRECTION ( 'NONE',  ( 0.000000000000000000, 1.000000000000000000, 0.000000000000000000 ) ) ;
#44081 = VECTOR ( 'NONE', #2895, 1000.000000000000000 ) ;
#44082 = FACE_BOUND ( 'NONE', #35483, .T. ) ;
#44083 = DIRECTION ( 'NONE',  ( 0.5338233779647948429, 0.000000000000000000, -0.8455960035018234011 ) ) ;
#44084 = CIRCLE ( 'NONE', #39046, 125.0000000000000000 ) ;
#44085 = AXIS2_PLACEMENT_3D ( 'NONE', #8451, #40761, #20814 ) ;
#44086 = DIRECTION ( 'NONE',  ( -0.7765238627180349740, 0.000000000000000000, -0.6300878435817203194 ) ) ;
#44087 = ORIENTED_EDGE ( 'NONE', *, *, #22939, .T. ) ;
#44088 = CIRCLE ( 'NONE', #13029, 60.00000000000000000 ) ;
#44089 = EDGE_CURVE ( 'NONE', #29776, #21157, #41939, .T. ) ;
#44090 = ORIENTED_EDGE ( 'NONE', *, *, #27479, .T. ) ;
#44091 = FACE_OUTER_BOUND ( 'NONE', #29611, .T. ) ;
#44092 = ORIENTED_EDGE ( 'NONE', *, *, #19549, .T. ) ;
#44093 = AXIS2_PLACEMENT_3D ( 'NONE', #39823, #47994, #16732 ) ;
#44094 = DIRECTION ( 'NONE',  ( 0.000000000000000000, -1.000000000000000000, 0.000000000000000000 ) ) ;
#44095 = VECTOR ( 'NONE', #23229, 1000.000000000000227 ) ;
#44096 = CARTESIAN_POINT ( 'NONE',  ( -330.4913330509368166, -115.8919814278863356, 58.50955523165747252 ) ) ;
#44097 = EDGE_CURVE ( 'NONE', #38627, #22578, #31186, .T. ) ;
#44098 = VECTOR ( 'NONE', #19670, 1000.000000000000000 ) ;
#44099 = VECTOR ( 'NONE', #28197, 1000.000000000000000 ) ;
#44100 = CARTESIAN_POINT ( 'NONE',  ( -339.1964088526558498, -95.63860483659122735, -52.00954392751761191 ) ) ;
#44101 = CARTESIAN_POINT ( 'NONE',  ( -49.42645310536304493, -175.3837268820161057, 0.3202698538628349079 ) ) ;
#44102 = VERTEX_POINT ( 'NONE', #21972 ) ;
#44105 = ORIENTED_EDGE ( 'NONE', *, *, #47879, .F. ) ;
#44104 = FACE_OUTER_BOUND ( 'NONE', #6377, .T. ) ;
#44103 = PLANE ( 'NONE',  #11582 ) ;
#44106 = EDGE_CURVE ( 'NONE', #39370, #46453, #14102, .T. ) ;
#44107 = VERTEX_POINT ( 'NONE', #30119 ) ;
#44108 = DIRECTION ( 'NONE',  ( 0.000000000000000000, 0.000000000000000000, 1.000000000000000000 ) ) ;
#44109 = VERTEX_POINT ( 'NONE', #6728 ) ;
#44110 = DIRECTION ( 'NONE',  ( 0.6068001458185834363, 0.000000000000000000, 0.7948544414133608127 ) ) ;
#44111 = EDGE_LOOP ( 'NONE', ( #451, #15023, #40604, #29451 ) ) ;
#44112 = CARTESIAN_POINT ( 'NONE',  ( 21.21056010634071853, -175.3837268820161057, 103.7706487676302061 ) ) ;
#44113 = ORIENTED_EDGE ( 'NONE', *, *, #49783, .T. ) ;
#44115 = CARTESIAN_POINT ( 'NONE',  ( -336.3521761649654422, -70.03480886230919111, 25.08789112700620194 ) ) ;
#44114 = CARTESIAN_POINT ( 'NONE',  ( -330.4913330509368166, -178.8432607619609200, -20.45418021416661247 ) ) ;
#44116 = ORIENTED_EDGE ( 'NONE', *, *, #30459, .T. ) ;
#44117 = EDGE_LOOP ( 'NONE', ( #4220, #2540, #39274, #20041 ) ) ;
#44118 = DIRECTION ( 'NONE',  ( 0.8124868780056863082, 0.000000000000000000, -0.5829794791144649047 ) ) ;
#44119 = VECTOR ( 'NONE', #41219, 1000.000000000000000 ) ;
#44120 = CARTESIAN_POINT ( 'NONE',  ( -58.29063029684667185, -193.5000000000000000, 124.6143426664034877 ) ) ;
#44121 = ADVANCED_FACE ( 'NONE', ( #46163 ), #14882, .T. ) ;
#44122 = DIRECTION ( 'NONE',  ( -1.000000000000000000, 0.000000000000000000, 0.000000000000000000 ) ) ;
#44123 = DIRECTION ( 'NONE',  ( 0.000000000000000000, 0.000000000000000000, -1.000000000000000000 ) ) ;
#44124 = CARTESIAN_POINT ( 'NONE',  ( -48.47912675150885065, -177.1207230881787780, 6.938893903907228378E-15 ) ) ;
#44125 = CIRCLE ( 'NONE', #10550, 125.0000000000000000 ) ;
#44126 = DIRECTION ( 'NONE',  ( 0.000000000000000000, 1.000000000000000000, 0.000000000000000000 ) ) ;
#44127 = AXIS2_PLACEMENT_3D ( 'NONE', #4004, #8713, #52 ) ;
#44128 = EDGE_CURVE ( 'NONE', #38011, #12927, #35381, .T. ) ;
#44129 = EDGE_LOOP ( 'NONE', ( #28594, #41180 ) ) ;
#44130 =( LENGTH_UNIT ( ) NAMED_UNIT ( * ) SI_UNIT ( .MILLI., .METRE. ) );
#44131 = CARTESIAN_POINT ( 'NONE',  ( -339.1964088526558498, -95.63860483659122735, -52.00954392751761191 ) ) ;
#44132 = DIRECTION ( 'NONE',  ( 0.000000000000000000, 0.000000000000000000, 1.000000000000000000 ) ) ;
#44133 = CARTESIAN_POINT ( 'NONE',  ( 49.10711742958949344, -193.5000000000000000, 78.11481899503480975 ) ) ;
#44134 = ORIENTED_EDGE ( 'NONE', *, *, #4403, .F. ) ;
#44135 = DIRECTION ( 'NONE',  ( 0.000000000000000000, -1.000000000000000000, 0.000000000000000000 ) ) ;
#44136 = AXIS2_PLACEMENT_3D ( 'NONE', #49448, #45490, #18144 ) ;
#44137 = VECTOR ( 'NONE', #110, 1000.000000000000000 ) ;
#44138 = DIRECTION ( 'NONE',  ( -1.000000000000000000, 0.000000000000000000, -0.000000000000000000 ) ) ;
#44139 = FACE_OUTER_BOUND ( 'NONE', #43348, .T. ) ;
#44140 = ORIENTED_EDGE ( 'NONE', *, *, #37813, .F. ) ;
#44141 = VERTEX_POINT ( 'NONE', #14351 ) ;
#44142 = AXIS2_PLACEMENT_3D ( 'NONE', #4507, #13427, #37331 ) ;
#44143 = ORIENTED_EDGE ( 'NONE', *, *, #3739, .T. ) ;
#44144 = AXIS2_PLACEMENT_3D ( 'NONE', #7747, #42724, #23777 ) ;
#44145 = FACE_OUTER_BOUND ( 'NONE', #31074, .T. ) ;
#44146 = CARTESIAN_POINT ( 'NONE',  ( -336.3521761649654422, -65.12692710742291524, -8.732051761643681687 ) ) ;
#44147 = DIRECTION ( 'NONE',  ( 0.000000000000000000, -1.000000000000000000, 0.000000000000000000 ) ) ;
#44148 = VERTEX_POINT ( 'NONE', #10142 ) ;
#44149 = EDGE_CURVE ( 'NONE', #24862, #19780, #14607, .T. ) ;
#44150 = DIRECTION ( 'NONE',  ( -0.000000000000000000, 0.8854560256532093554, -0.4647231720437695057 ) ) ;
#44151 = ORIENTED_EDGE ( 'NONE', *, *, #35318, .T. ) ;
#44152 = EDGE_CURVE ( 'NONE', #14246, #10133, #36204, .T. ) ;
#44153 = ORIENTED_EDGE ( 'NONE', *, *, #24481, .T. ) ;
#44154 = ORIENTED_EDGE ( 'NONE', *, *, #31335, .T. ) ;
#44155 = CIRCLE ( 'NONE', #30717, 60.00000000000000000 ) ;
#44156 = AXIS2_PLACEMENT_3D ( 'NONE', #19213, #18943, #11298 ) ;
#44157 = VERTEX_POINT ( 'NONE', #22227 ) ;
#44158 = CARTESIAN_POINT ( 'NONE',  ( 63.10841233855954613, -189.7472609257535510, -54.07611884703302962 ) ) ;
#44159 = CIRCLE ( 'NONE', #1363, 125.0000000000000000 ) ;
#44160 = VECTOR ( 'NONE', #39214, 1000.000000000000000 ) ;
#44161 = ADVANCED_FACE ( 'NONE', ( #38251 ), #18301, .T. ) ;
#44162 = VERTEX_POINT ( 'NONE', #47713 ) ;
#44163 = EDGE_CURVE ( 'NONE', #6145, #4347, #7503, .T. ) ;
#44164 = EDGE_CURVE ( 'NONE', #4631, #43537, #22792, .T. ) ;
#44165 = CARTESIAN_POINT ( 'NONE',  ( 70.19984492582109681, -193.5000000000000000, 39.24667733211968823 ) ) ;
#44166 = PLANE ( 'NONE',  #34458 ) ;
#44169 = EDGE_LOOP ( 'NONE', ( #25772, #15116, #12491, #43670 ) ) ;
#44168 = FACE_OUTER_BOUND ( 'NONE', #40307, .T. ) ;
#44167 = DIRECTION ( 'NONE',  ( 0.000000000000000000, 0.000000000000000000, 1.000000000000000000 ) ) ;
#44170 = AXIS2_PLACEMENT_3D ( 'NONE', #37974, #10378, #50595 ) ;
#44171 = EDGE_CURVE ( 'NONE', #50347, #51592, #35592, .T. ) ;
#44172 = AXIS2_PLACEMENT_3D ( 'NONE', #37165, #25346, #905 ) ;
#44173 = VECTOR ( 'NONE', #49130, 1000.000000000000000 ) ;
#44174 = PLANE ( 'NONE',  #2953 ) ;
#44176 = ORIENTED_EDGE ( 'NONE', *, *, #42993, .F. ) ;
#44175 = AXIS2_PLACEMENT_3D ( 'NONE', #21118, #359, #5363 ) ;
#44177 = DIRECTION ( 'NONE',  ( 0.000000000000000000, 0.9350162426854146114, -0.3546048870425363986 ) ) ;
#44178 = ORIENTED_EDGE ( 'NONE', *, *, #13204, .F. ) ;
#44179 = DIRECTION ( 'NONE',  ( -0.000000000000000000, 1.000000000000000000, 0.000000000000000000 ) ) ;
#44180 = CIRCLE ( 'NONE', #33270, 4.999999999999997335 ) ;
#44181 = PLANE ( 'NONE',  #6198 ) ;
#44183 = CYLINDRICAL_SURFACE ( 'NONE', #29878, 125.0000000000000000 ) ;
#44182 = DIRECTION ( 'NONE',  ( -1.000000000000000000, 2.497772389992620524E-15, 1.013386094502321458E-14 ) ) ;
#44184 = ORIENTED_EDGE ( 'NONE', *, *, #44006, .T. ) ;
#44185 = AXIS2_PLACEMENT_3D ( 'NONE', #22918, #27101, #43138 ) ;
#44186 = CARTESIAN_POINT ( 'NONE',  ( -172.3334410065085933, -183.6283474603465606, -6.025661128238047226 ) ) ;
#44187 = CARTESIAN_POINT ( 'NONE',  ( 5.015379008610418410, -193.5000000000000000, -112.9749434763326690 ) ) ;
#44188 = VERTEX_POINT ( 'NONE', #4080 ) ;
#44189 = VECTOR ( 'NONE', #35695, 999.9999999999998863 ) ;
#44190 = LINE ( 'NONE', #24468, #24950 ) ;
#44191 = DIRECTION ( 'NONE',  ( 0.000000000000000000, 0.000000000000000000, 1.000000000000000000 ) ) ;
#44192 = DIRECTION ( 'NONE',  ( 0.000000000000000000, 1.000000000000000000, 0.000000000000000000 ) ) ;
#44193 = VERTEX_POINT ( 'NONE', #47958 ) ;
#44194 = DIRECTION ( 'NONE',  ( 0.9151456172430210145, 0.000000000000000000, -0.4031234292879665171 ) ) ;
#44195 = LINE ( 'NONE', #3998, #47468 ) ;
#44196 = ORIENTED_EDGE ( 'NONE', *, *, #6562, .T. ) ;
#44197 = CARTESIAN_POINT ( 'NONE',  ( -336.3521761649653854, -139.4384828369889249, -57.84431488793872944 ) ) ;
#44198 = EDGE_LOOP ( 'NONE', ( #652, #45061, #26555, #50839 ) ) ;
#44199 = VECTOR ( 'NONE', #36119, 1000.000000000000000 ) ;
#44200 = VECTOR ( 'NONE', #36312, 1000.000000000000000 ) ;
#44201 = LINE ( 'NONE', #36053, #21432 ) ;
#44202 = CARTESIAN_POINT ( 'NONE',  ( 69.88207517204678254, -193.5000000000000000, 40.19484891390058579 ) ) ;
#44203 = AXIS2_PLACEMENT_3D ( 'NONE', #32871, #28926, #9495 ) ;
#44204 = DIRECTION ( 'NONE',  ( -1.000000000000000000, -0.000000000000000000, 0.000000000000000000 ) ) ;
#44205 = FACE_OUTER_BOUND ( 'NONE', #22495, .T. ) ;
#44206 = DIRECTION ( 'NONE',  ( 0.000000000000000000, 0.9709418174260502354, -0.2393156642875652051 ) ) ;
#44207 = CARTESIAN_POINT ( 'NONE',  ( -336.3521761649654422, -181.4155151828941825, -11.56382487286496463 ) ) ;
#44208 = AXIS2_PLACEMENT_3D ( 'NONE', #46593, #10576, #5356 ) ;
#44209 = VECTOR ( 'NONE', #23390, 1000.000000000000000 ) ;
#44210 = PLANE ( 'NONE',  #8528 ) ;
#44211 = CARTESIAN_POINT ( 'NONE',  ( -339.1964088526558498, -74.65991953890826949, 33.10432812419072945 ) ) ;
#44213 = ORIENTED_EDGE ( 'NONE', *, *, #3170, .T. ) ;
#44212 = CARTESIAN_POINT ( 'NONE',  ( -336.3521761649654422, -161.4024510877913485, 45.24454186338643780 ) ) ;
#44214 = CIRCLE ( 'NONE', #34982, 125.0000000000000000 ) ;
#44215 = AXIS2_PLACEMENT_3D ( 'NONE', #6905, #19499, #38947 ) ;
#44216 = ORIENTED_EDGE ( 'NONE', *, *, #38802, .F. ) ;
#44217 = EDGE_CURVE ( 'NONE', #23438, #18322, #8271, .T. ) ;
#44218 = EDGE_CURVE ( 'NONE', #11822, #28559, #23276, .T. ) ;
#44219 = DIRECTION ( 'NONE',  ( -0.000000000000000000, 0.000000000000000000, 1.000000000000000000 ) ) ;
#44220 = CIRCLE ( 'NONE', #34135, 60.00000000000000000 ) ;
#44221 = VECTOR ( 'NONE', #21834, 1000.000000000000000 ) ;
#44222 = DIRECTION ( 'NONE',  ( -0.000000000000000000, 1.000000000000000000, -0.000000000000000000 ) ) ;
#44223 = VERTEX_POINT ( 'NONE', #35866 ) ;
#44224 = ORIENTED_EDGE ( 'NONE', *, *, #26037, .F. ) ;
#44225 = EDGE_LOOP ( 'NONE', ( #24832, #11535, #4608, #15191 ) ) ;
#44226 = DIRECTION ( 'NONE',  ( -0.000000000000000000, -0.4647231720437604574, 0.8854560256532141294 ) ) ;
#44227 = EDGE_CURVE ( 'NONE', #47448, #10566, #11167, .T. ) ;
#44228 = EDGE_CURVE ( 'NONE', #40758, #38078, #3298, .T. ) ;
#44229 = CARTESIAN_POINT ( 'NONE',  ( 42.45000882818163035, -175.3837268820161057, -84.30834960112932208 ) ) ;
#44230 = DIRECTION ( 'NONE',  ( 0.000000000000000000, -1.000000000000000000, -0.000000000000000000 ) ) ;
#44231 = ORIENTED_EDGE ( 'NONE', *, *, #46158, .T. ) ;
#44232 = VERTEX_POINT ( 'NONE', #15650 ) ;
#44233 = ADVANCED_FACE ( 'NONE', ( #19833 ), #11691, .F. ) ;
#44234 = ORIENTED_EDGE ( 'NONE', *, *, #9964, .F. ) ;
#44235 = DIRECTION ( 'NONE',  ( 0.6965510290629982615, 0.000000000000000000, -0.7175072570443298270 ) ) ;
#44236 = CARTESIAN_POINT ( 'NONE',  ( -96.30460367372252506, -183.6283474603465606, -114.4068333132746176 ) ) ;
#44237 = VECTOR ( 'NONE', #2560, 1000.000000000000000 ) ;
#44238 = CARTESIAN_POINT ( 'NONE',  ( 38.46761263173351608, -175.3837268820161057, 89.80681772907068705 ) ) ;
#44239 = CIRCLE ( 'NONE', #43421, 125.0000000000000000 ) ;
#44240 = ADVANCED_FACE ( 'NONE', ( #35343 ), #43228, .T. ) ;
#44241 = DIRECTION ( 'NONE',  ( 1.000000000000000000, -0.000000000000000000, -0.000000000000000000 ) ) ;
#44242 = LINE ( 'NONE', #35562, #33975 ) ;
#44243 = ORIENTED_EDGE ( 'NONE', *, *, #32952, .T. ) ;
#44244 = CARTESIAN_POINT ( 'NONE',  ( 33.25242634436024503, -175.3837268820161057, -94.57776286494160445 ) ) ;
#44245 = CIRCLE ( 'NONE', #21601, 125.0000000000000000 ) ;
#44246 = EDGE_CURVE ( 'NONE', #49764, #33603, #42926, .T. ) ;
#44247 = CARTESIAN_POINT ( 'NONE',  ( -339.1964088526558498, -84.75001853787875916, -44.49369547121548862 ) ) ;
#44248 = DIRECTION ( 'NONE',  ( -0.000000000000000000, -1.000000000000000000, 3.491481338843133355E-15 ) ) ;
#44249 = DIRECTION ( 'NONE',  ( -0.8455960035018272869, 0.000000000000000000, 0.5338233779647886257 ) ) ;
#44250 = VERTEX_POINT ( 'NONE', #116 ) ;
#44251 = ORIENTED_EDGE ( 'NONE', *, *, #32344, .F. ) ;
#44252 = AXIS2_PLACEMENT_3D ( 'NONE', #36338, #31363, #32393 ) ;
#44253 = ORIENTED_EDGE ( 'NONE', *, *, #8160, .F. ) ;
#44254 = CARTESIAN_POINT ( 'NONE',  ( -27.36201831380532923, -189.7472609257535510, -122.1886788576022411 ) ) ;
#44255 = LINE ( 'NONE', #36357, #32527 ) ;
#44256 = VECTOR ( 'NONE', #7963, 1000.000000000000000 ) ;
#44257 = ORIENTED_EDGE ( 'NONE', *, *, #11832, .T. ) ;
#44258 = DIRECTION ( 'NONE',  ( 0.000000000000000000, 0.7485107481710953081, -0.6631226582408016323 ) ) ;
#44259 = VECTOR ( 'NONE', #46979, 1000.000000000000114 ) ;
#44260 = CARTESIAN_POINT ( 'NONE',  ( 76.21810084846656252, -183.6283474603465606, -8.694908215727984668 ) ) ;
#44261 = VERTEX_POINT ( 'NONE', #51397 ) ;
#44262 = FACE_OUTER_BOUND ( 'NONE', #33299, .T. ) ;
#44263 = CIRCLE ( 'NONE', #26630, 125.0000000000000000 ) ;
#44264 = AXIS2_PLACEMENT_3D ( 'NONE', #42353, #30274, #46574 ) ;
#44265 = ORIENTED_EDGE ( 'NONE', *, *, #8027, .T. ) ;
#44266 = DIRECTION ( 'NONE',  ( -0.7765238627180349740, 0.000000000000000000, -0.6300878435817203194 ) ) ;
#44267 = ORIENTED_EDGE ( 'NONE', *, *, #51887, .T. ) ;
#44268 = DIRECTION ( 'NONE',  ( 0.2635871660690715101, 0.000000000000000000, -0.9646355819083576311 ) ) ;
#44269 = FACE_BOUND ( 'NONE', #4945, .T. ) ;
#44270 = DIRECTION ( 'NONE',  ( -0.9785564922995032555, 0.000000000000000000, -0.2059786187411021818 ) ) ;
#44271 = ORIENTED_EDGE ( 'NONE', *, *, #40446, .T. ) ;
#44272 = FACE_OUTER_BOUND ( 'NONE', #17318, .T. ) ;
#44273 = CARTESIAN_POINT ( 'NONE',  ( -115.4536696835168357, -183.6283474603465606, -105.5434062319793611 ) ) ;
#44274 = DIRECTION ( 'NONE',  ( 0.000000000000000000, -1.000000000000000000, 0.000000000000000000 ) ) ;
#44275 = FACE_OUTER_BOUND ( 'NONE', #7701, .T. ) ;
#44276 = ORIENTED_EDGE ( 'NONE', *, *, #19334, .F. ) ;
#44277 = DIRECTION ( 'NONE',  ( 0.000000000000000000, 1.000000000000000000, 0.000000000000000000 ) ) ;
#44278 = EDGE_LOOP ( 'NONE', ( #28948, #2272, #5477, #23825 ) ) ;
#44279 = ADVANCED_FACE ( 'NONE', ( #15387 ), #24041, .F. ) ;
#44280 = ORIENTED_EDGE ( 'NONE', *, *, #39759, .T. ) ;
#44281 = AXIS2_PLACEMENT_3D ( 'NONE', #25129, #41400, #41143 ) ;
#44282 = AXIS2_PLACEMENT_3D ( 'NONE', #22016, #1263, #25961 ) ;
#44283 = CARTESIAN_POINT ( 'NONE',  ( 141.7825277784304205, -193.5000000000000000, 10.00000000000000178 ) ) ;
#44285 = ORIENTED_EDGE ( 'NONE', *, *, #17612, .F. ) ;
#44284 = FACE_OUTER_BOUND ( 'NONE', #47337, .T. ) ;
#44286 = AXIS2_PLACEMENT_3D ( 'NONE', #17741, #34008, #45088 ) ;
#44287 = EDGE_CURVE ( 'NONE', #7639, #12625, #31919, .T. ) ;
#44288 = ADVANCED_FACE ( 'NONE', ( #11939 ), #47441, .F. ) ;
#44289 = EDGE_LOOP ( 'NONE', ( #4575, #8014, #31303, #36502 ) ) ;
#44290 = ADVANCED_FACE ( 'NONE', ( #43500 ), #31144, .F. ) ;
#44291 = CARTESIAN_POINT ( 'NONE',  ( -47.49008656418669005, -183.6283474603465606, 0.1476465640024920423 ) ) ;
#44292 = EDGE_CURVE ( 'NONE', #29433, #18178, #39535, .T. ) ;
#44293 = EDGE_CURVE ( 'NONE', #29270, #27177, #16941, .T. ) ;
#44294 = DIRECTION ( 'NONE',  ( 0.000000000000000000, 1.000000000000000000, 0.000000000000000000 ) ) ;
#44295 = CIRCLE ( 'NONE', #27515, 60.00000000000000000 ) ;
#44296 = ORIENTED_EDGE ( 'NONE', *, *, #42312, .T. ) ;
#44297 = DIRECTION ( 'NONE',  ( -1.000000000000000000, 0.000000000000000000, 0.000000000000000000 ) ) ;
#44298 = EDGE_CURVE ( 'NONE', #40001, #24499, #29530, .T. ) ;
#44299 = CARTESIAN_POINT ( 'NONE',  ( -48.71401279728982558, -189.7472609257535510, -0.9720229140804069745 ) ) ;
#44300 = ORIENTED_EDGE ( 'NONE', *, *, #22816, .T. ) ;
#44301 = DIRECTION ( 'NONE',  ( -1.000000000000000000, 0.000000000000000000, 0.000000000000000000 ) ) ;
#44302 = FACE_OUTER_BOUND ( 'NONE', #21146, .T. ) ;
#44303 = CIRCLE ( 'NONE', #12394, 125.0000000000000000 ) ;
#44304 = ADVANCED_FACE ( 'NONE', ( #24552 ), #1424, .T. ) ;
#44305 = DIRECTION ( 'NONE',  ( 1.000000000000000000, 0.000000000000000000, 0.000000000000000000 ) ) ;
#44306 = DIRECTION ( 'NONE',  ( 0.9929810960135178055, 0.000000000000000000, -0.1182731709213592358 ) ) ;
#44307 = ORIENTED_EDGE ( 'NONE', *, *, #243, .F. ) ;
#44308 = ORIENTED_EDGE ( 'NONE', *, *, #12778, .T. ) ;
#44309 = ADVANCED_FACE ( 'NONE', ( #5377 ), #32949, .T. ) ;
#44310 = EDGE_LOOP ( 'NONE', ( #31320, #30989, #29324, #2441 ) ) ;
#44311 = CIRCLE ( 'NONE', #20821, 125.0000000000000000 ) ;
#44312 = CARTESIAN_POINT ( 'NONE',  ( -48.47912675150885065, -177.1207230881787780, 6.938893903907228378E-15 ) ) ;
#44313 = CARTESIAN_POINT ( 'NONE',  ( -332.3517673607765914, -181.0704707379907745, 16.90091414705587525 ) ) ;
#44314 = ADVANCED_FACE ( 'NONE', ( #48493 ), #8777, .F. ) ;
#44315 = CARTESIAN_POINT ( 'NONE',  ( -111.8989814360438686, -189.7472609257535510, -107.7168604805787169 ) ) ;
#44316 = FACE_BOUND ( 'NONE', #26865, .T. ) ;
#44317 = CARTESIAN_POINT ( 'NONE',  ( -305.0000000000000568, -126.1322888500942554, -59.94223098458773080 ) ) ;
#44318 = ORIENTED_EDGE ( 'NONE', *, *, #27781, .T. ) ;
#44319 = EDGE_CURVE ( 'NONE', #12735, #4174, #32443, .T. ) ;
#44320 = EDGE_CURVE ( 'NONE', #41179, #16323, #49000, .T. ) ;
#44321 = ORIENTED_EDGE ( 'NONE', *, *, #17300, .T. ) ;
#44323 = ORIENTED_EDGE ( 'NONE', *, *, #38489, .T. ) ;
#44322 = LINE ( 'NONE', #40602, #44935 ) ;
#44324 = LINE ( 'NONE', #31181, #37204 ) ;
#44325 = VECTOR ( 'NONE', #50282, 1000.000000000000114 ) ;
#44326 = EDGE_LOOP ( 'NONE', ( #39972, #12490, #49540, #35270 ) ) ;
#44327 = CIRCLE ( 'NONE', #15816, 125.0000000000000000 ) ;
#44328 = LINE ( 'NONE', #8316, #41722 ) ;
#44329 = CARTESIAN_POINT ( 'NONE',  ( -47.48307690889363641, -189.7472609257535510, -0.08879589532292464504 ) ) ;
#44330 = VECTOR ( 'NONE', #32900, 1000.000000000000000 ) ;
#44331 = DIRECTION ( 'NONE',  ( -1.000000000000000000, -8.589602288500833124E-15, -5.928974370888904820E-15 ) ) ;
#44332 = DIRECTION ( 'NONE',  ( -0.1182731709213730997, 0.000000000000000000, 0.9929810960135161402 ) ) ;
#44333 = ORIENTED_EDGE ( 'NONE', *, *, #4867, .F. ) ;
#44334 = CARTESIAN_POINT ( 'NONE',  ( -336.3521761649654422, -128.9912765084839066, 58.76657425099337928 ) ) ;
#44335 = VERTEX_POINT ( 'NONE', #21392 ) ;
#44336 = EDGE_CURVE ( 'NONE', #32514, #47785, #33494, .T. ) ;
#44337 = EDGE_CURVE ( 'NONE', #12908, #49461, #22001, .T. ) ;
#44338 = ORIENTED_EDGE ( 'NONE', *, *, #15986, .T. ) ;
#44339 = DIRECTION ( 'NONE',  ( -0.000000000000000000, 1.000000000000000000, -0.000000000000000000 ) ) ;
#44340 = AXIS2_PLACEMENT_3D ( 'NONE', #19292, #4030, #20048 ) ;
#44341 = CARTESIAN_POINT ( 'NONE',  ( -50.89116676070555911, -183.6283474603465606, 124.9767260852757147 ) ) ;
#44342 = DIRECTION ( 'NONE',  ( 0.000000000000000000, -0.000000000000000000, 1.000000000000000000 ) ) ;
#44343 = CARTESIAN_POINT ( 'NONE',  ( 68.79964045138289919, -193.5000000000000000, 43.25148278810711133 ) ) ;
#44344 = CARTESIAN_POINT ( 'NONE',  ( -0.3054481938615516423, -183.6283474603465606, 115.3442529744090450 ) ) ;
#44345 = VERTEX_POINT ( 'NONE', #894 ) ;
#44346 = DIRECTION ( 'NONE',  ( 0.7765238627180393038, 0.000000000000000000, 0.6300878435817147682 ) ) ;
#44347 = DIRECTION ( 'NONE',  ( 0.000000000000000000, 0.000000000000000000, -1.000000000000000000 ) ) ;
#44348 = AXIS2_PLACEMENT_3D ( 'NONE', #14463, #10496, #26529 ) ;
#44349 = FACE_BOUND ( 'NONE', #39799, .T. ) ;
#44350 = ORIENTED_EDGE ( 'NONE', *, *, #140, .T. ) ;
#44351 = DIRECTION ( 'NONE',  ( -0.000000000000000000, -0.6631226582407885317, 0.7485107481711069655 ) ) ;
#44352 = CARTESIAN_POINT ( 'NONE',  ( -170.0000000000000284, -173.5000000000000284, 60.00000000000000000 ) ) ;
#44353 = EDGE_CURVE ( 'NONE', #47028, #17270, #44531, .T. ) ;
#44354 = VERTEX_POINT ( 'NONE', #36377 ) ;
#44355 = EDGE_CURVE ( 'NONE', #33506, #34708, #8517, .T. ) ;
#44356 = DIRECTION ( 'NONE',  ( 0.9473263538541946138, 0.000000000000000000, -0.3202698538628279690 ) ) ;
#44357 = ORIENTED_EDGE ( 'NONE', *, *, #11877, .F. ) ;
#44358 = EDGE_CURVE ( 'NONE', #42260, #18995, #29536, .T. ) ;
#44359 = EDGE_CURVE ( 'NONE', #48723, #7602, #20892, .T. ) ;
#44360 = PRODUCT_DEFINITION_FORMATION_WITH_SPECIFIED_SOURCE ( 'ANY', '', #20959, .NOT_KNOWN. ) ;
#44361 = DIRECTION ( 'NONE',  ( -0.000000000000000000, 1.000000000000000000, -0.000000000000000000 ) ) ;
#44362 = CIRCLE ( 'NONE', #21702, 125.0000000000000000 ) ;
#44363 = AXIS2_PLACEMENT_3D ( 'NONE', #19162, #50456, #30213 ) ;
#44364 = LINE ( 'NONE', #24377, #33497 ) ;
#44366 = ORIENTED_EDGE ( 'NONE', *, *, #47034, .T. ) ;
#44365 = DIRECTION ( 'NONE',  ( -0.000000000000000000, 1.000000000000000000, -0.000000000000000000 ) ) ;
#44367 = CARTESIAN_POINT ( 'NONE',  ( -60.80616967713025645, -177.1207230881787780, -123.3865623328508150 ) ) ;
#44368 = EDGE_LOOP ( 'NONE', ( #5857, #41025, #18106, #43838 ) ) ;
#44369 = ORIENTED_EDGE ( 'NONE', *, *, #19463, .T. ) ;
#44370 = LINE ( 'NONE', #28048, #36825 ) ;
#44371 = AXIS2_PLACEMENT_3D ( 'NONE', #18823, #6504, #46439 ) ;
#44372 = ORIENTED_EDGE ( 'NONE', *, *, #51887, .F. ) ;
#44373 = PRODUCT_DEFINITION ( 'UNKNOWN', '', #6621, #29563 ) ;
#44374 = DIRECTION ( 'NONE',  ( -0.6300878435817203194, 0.000000000000000000, 0.7765238627180349740 ) ) ;
#44375 = DIRECTION ( 'NONE',  ( 0.000000000000000000, 0.000000000000000000, 1.000000000000000000 ) ) ;
#44376 = ADVANCED_FACE ( 'NONE', ( #16697 ), #12975, .T. ) ;
#44377 = VECTOR ( 'NONE', #47490, 1000.000000000000114 ) ;
#44378 = LINE ( 'NONE', #11774, #18369 ) ;
#44379 = DIRECTION ( 'NONE',  ( 0.000000000000000000, 0.000000000000000000, 1.000000000000000000 ) ) ;
#44380 = ORIENTED_EDGE ( 'NONE', *, *, #46865, .F. ) ;
#44383 = ORIENTED_EDGE ( 'NONE', *, *, #5411, .T. ) ;
#44382 = PLANE ( 'NONE',  #18887 ) ;
#44381 = DIRECTION ( 'NONE',  ( 0.000000000000000000, -0.000000000000000000, 1.000000000000000000 ) ) ;
#44384 = ORIENTED_EDGE ( 'NONE', *, *, #36288, .T. ) ;
#44385 = DIRECTION ( 'NONE',  ( 0.9842305779475954974, 0.000000000000000000, 0.1768902751225803205 ) ) ;
#44386 = EDGE_LOOP ( 'NONE', ( #20833, #748, #10295, #47946 ) ) ;
#44387 = CARTESIAN_POINT ( 'NONE',  ( -49.45768324380835423, -177.1207230881787780, 0.2059786187410958813 ) ) ;
#44388 = VERTEX_POINT ( 'NONE', #21128 ) ;
#44389 = FACE_OUTER_BOUND ( 'NONE', #7225, .T. ) ;
#44390 = DIRECTION ( 'NONE',  ( -0.2920567706369833760, 0.000000000000000000, 0.9564009842765202052 ) ) ;
#44391 = ORIENTED_EDGE ( 'NONE', *, *, #5627, .F. ) ;
#44393 = DIRECTION ( 'NONE',  ( 0.000000000000000000, -1.000000000000000000, 0.000000000000000000 ) ) ;
#44392 = CARTESIAN_POINT ( 'NONE',  ( -339.1964088526558498, -157.9941932480463436, 49.09328500076600221 ) ) ;
#44394 = ORIENTED_EDGE ( 'NONE', *, *, #50415, .T. ) ;
#44395 = ORIENTED_EDGE ( 'NONE', *, *, #6717, .F. ) ;
#44396 = DIRECTION ( 'NONE',  ( 0.000000000000000000, 1.000000000000000000, 0.000000000000000000 ) ) ;
#44397 = VECTOR ( 'NONE', #16618, 999.9999999999998863 ) ;
#44398 = CARTESIAN_POINT ( 'NONE',  ( 30.00000000000000711, -43.50000000000000000, -30.00000000000000355 ) ) ;
#44399 = AXIS2_PLACEMENT_3D ( 'NONE', #40982, #44674, #16292 ) ;
#44400 = LINE ( 'NONE', #51502, #12943 ) ;
#44401 = FACE_OUTER_BOUND ( 'NONE', #30221, .T. ) ;
#44402 = CARTESIAN_POINT ( 'NONE',  ( -48.47912675150885065, -183.6283474603465606, 6.938893903907228378E-15 ) ) ;
#44403 = AXIS2_PLACEMENT_3D ( 'NONE', #28321, #44374, #16514 ) ;
#44404 = DIRECTION ( 'NONE',  ( 0.000000000000000000, 1.000000000000000000, 0.000000000000000000 ) ) ;
#44405 = EDGE_LOOP ( 'NONE', ( #23870, #30299, #2293, #29601 ) ) ;
#44406 = CARTESIAN_POINT ( 'NONE',  ( 0.000000000000000000, 0.000000000000000000, 0.000000000000000000 ) ) ;
#44407 = CARTESIAN_POINT ( 'NONE',  ( -88.49718702276014426, -177.1207230881787780, -117.3655938605927531 ) ) ;
#44408 = CARTESIAN_POINT ( 'NONE',  ( -336.3521761649654422, -70.49953203435293858, 25.97334715265942151 ) ) ;
#44409 = LINE ( 'NONE', #39912, #47276 ) ;
#44410 = VERTEX_POINT ( 'NONE', #32699 ) ;
#44411 = VECTOR ( 'NONE', #42989, 1000.000000000000114 ) ;
#44412 = LINE ( 'NONE', #31804, #47516 ) ;
#44413 = CARTESIAN_POINT ( 'NONE',  ( -332.3517673607765914, -181.7525362123217292, 9.724760635742144999 ) ) ;
#44414 = DIRECTION ( 'NONE',  ( 0.000000000000000000, 0.000000000000000000, 1.000000000000000000 ) ) ;
#44415 = EDGE_LOOP ( 'NONE', ( #45177, #24185, #36649, #15365 ) ) ;
#44416 = EDGE_CURVE ( 'NONE', #39427, #9601, #5211, .T. ) ;
#44417 = VERTEX_POINT ( 'NONE', #33216 ) ;
#44418 = ORIENTED_EDGE ( 'NONE', *, *, #30302, .T. ) ;
#44419 = CIRCLE ( 'NONE', #14228, 125.0000000000000000 ) ;
#44420 = DIRECTION ( 'NONE',  ( 0.9960498426152158968, 0.000000000000000000, 0.08879589532294571153 ) ) ;
#44421 = DIRECTION ( 'NONE',  ( 0.000000000000000000, -1.000000000000000000, 0.000000000000000000 ) ) ;
#44422 = DIRECTION ( 'NONE',  ( 0.000000000000000000, -1.420160285666346159E-13, -1.000000000000000000 ) ) ;
#44423 = CYLINDRICAL_SURFACE ( 'NONE', #2728, 15.00000000000000000 ) ;
#44424 = VERTEX_POINT ( 'NONE', #49265 ) ;
#44425 = CARTESIAN_POINT ( 'NONE',  ( -173.4787860028527007, -177.1207230881787780, 0.2918682030023981300 ) ) ;
#44426 = DIRECTION ( 'NONE',  ( 0.000000000000000000, 0.5680647467311569221, 0.8229838658936556861 ) ) ;
#44427 = ORIENTED_EDGE ( 'NONE', *, *, #30225, .F. ) ;
#44428 = ORIENTED_EDGE ( 'NONE', *, *, #15418, .T. ) ;
#44429 = AXIS2_PLACEMENT_3D ( 'NONE', #8530, #11950, #16708 ) ;
#44430 = ORIENTED_EDGE ( 'NONE', *, *, #25647, .T. ) ;
#44431 = EDGE_CURVE ( 'NONE', #37437, #16495, #49699, .T. ) ;
#44432 = PLANE ( 'NONE',  #45205 ) ;
#44433 = VECTOR ( 'NONE', #27218, 1000.000000000000000 ) ;
#44434 = DIRECTION ( 'NONE',  ( -0.000000000000000000, 1.000000000000000000, -0.000000000000000000 ) ) ;
#44435 = DIRECTION ( 'NONE',  ( 0.000000000000000000, 1.000000000000000000, -0.000000000000000000 ) ) ;
#44438 = EDGE_LOOP ( 'NONE', ( #20115, #31133, #37772, #35904, #26103, #32373, #24822, #4692, #22127, #47007, #38957, #35621 ) ) ;
#44437 = CARTESIAN_POINT ( 'NONE',  ( -48.30901192927175458, -193.5000000000000000, -124.9998842437354227 ) ) ;
#44436 = LINE ( 'NONE', #20250, #19099 ) ;
#44439 = EDGE_CURVE ( 'NONE', #37940, #30972, #41354, .T. ) ;
#44440 = LINE ( 'NONE', #8426, #50835 ) ;
#44441 = ORIENTED_EDGE ( 'NONE', *, *, #43981, .T. ) ;
#44442 = DIRECTION ( 'NONE',  ( -0.000000000000000000, 1.000000000000000000, 0.000000000000000000 ) ) ;
#44443 = LINE ( 'NONE', #4497, #35005 ) ;
#44444 = EDGE_LOOP ( 'NONE', ( #50900, #44989, #10803, #51868 ) ) ;
#44445 = CARTESIAN_POINT ( 'NONE',  ( 68.59638248015004081, -177.1207230881787780, -43.79868877201405297 ) ) ;
#44446 = ADVANCED_FACE ( 'NONE', ( #39700 ), #35773, .T. ) ;
#44447 = PLANE ( 'NONE',  #43476 ) ;
#44449 = DIRECTION ( 'NONE',  ( 0.000000000000000000, 0.000000000000000000, -1.000000000000000000 ) ) ;
#44448 = DIRECTION ( 'NONE',  ( 0.000000000000000000, -0.000000000000000000, 1.000000000000000000 ) ) ;
#44450 = VERTEX_POINT ( 'NONE', #11611 ) ;
#44451 = VECTOR ( 'NONE', #6072, 1000.000000000000114 ) ;
#44452 = CARTESIAN_POINT ( 'NONE',  ( -81.14588623932559130, -177.1207230881787780, 120.6560517527617975 ) ) ;
#44453 = CARTESIAN_POINT ( 'NONE',  ( 73.79319191488886531, -183.6283474603465606, 20.63201007055493008 ) ) ;
#44454 = ADVANCED_FACE ( 'NONE', ( #37 ), #43919, .F. ) ;
#44455 = ORIENTED_EDGE ( 'NONE', *, *, #23921, .F. ) ;
#44456 = DIRECTION ( 'NONE',  ( 0.000000000000000000, 0.000000000000000000, 1.000000000000000000 ) ) ;
#44457 = LINE ( 'NONE', #16332, #47552 ) ;
#44458 = EDGE_LOOP ( 'NONE', ( #17567, #41422 ) ) ;
#44459 = DIRECTION ( 'NONE',  ( -1.000000000000000000, 0.000000000000000000, -4.884776371667511665E-16 ) ) ;
#44460 = DIRECTION ( 'NONE',  ( 1.000000000000000000, -0.000000000000000000, 0.000000000000000000 ) ) ;
#44461 = ADVANCED_FACE ( 'NONE', ( #32619 ), #39964, .T. ) ;
#44462 = VERTEX_POINT ( 'NONE', #36040 ) ;
#44463 = DIRECTION ( 'NONE',  ( 0.000000000000000000, 0.000000000000000000, 1.000000000000000000 ) ) ;
#44464 = ORIENTED_EDGE ( 'NONE', *, *, #45256, .F. ) ;
#44465 = AXIS2_PLACEMENT_3D ( 'NONE', #5717, #1752, #21470 ) ;
#44466 = CARTESIAN_POINT ( 'NONE',  ( -48.93575598890255662, -183.6283474603465606, -0.8896570909947461026 ) ) ;
#44467 = DIRECTION ( 'NONE',  ( -1.000000000000000000, -0.000000000000000000, 0.000000000000000000 ) ) ;
#44468 = FACE_OUTER_BOUND ( 'NONE', #17375, .T. ) ;
#44469 = DIRECTION ( 'NONE',  ( 0.000000000000000000, -1.000000000000000000, 0.000000000000000000 ) ) ;
#44470 = LINE ( 'NONE', #8717, #33328 ) ;
#44471 = EDGE_CURVE ( 'NONE', #755, #47167, #4244, .T. ) ;
#44472 = ADVANCED_FACE ( 'NONE', ( #35511 ), #43667, .T. ) ;
#44473 = DIRECTION ( 'NONE',  ( 0.000000000000000000, 1.000000000000000000, 0.000000000000000000 ) ) ;
#44474 = EDGE_CURVE ( 'NONE', #17110, #22066, #12377, .T. ) ;
#44475 = DIRECTION ( 'NONE',  ( -0.4566292373937018145, 0.000000000000000000, -0.8896570909947529859 ) ) ;
#44477 = VERTEX_POINT ( 'NONE', #36547 ) ;
#44476 = CARTESIAN_POINT ( 'NONE',  ( 0.000000000000000000, -63.50000000000000000, 0.000000000000000000 ) ) ;
#44478 = ORIENTED_EDGE ( 'NONE', *, *, #11042, .T. ) ;
#44479 = FACE_OUTER_BOUND ( 'NONE', #22997, .T. ) ;
#44480 = AXIS2_PLACEMENT_3D ( 'NONE', #21354, #41573, #1110 ) ;
#44481 = VECTOR ( 'NONE', #1155, 1000.000000000000000 ) ;
#44482 = CARTESIAN_POINT ( 'NONE',  ( 2.347046875550483230E-15, 0.000000000000000000, 51.00000000000000711 ) ) ;
#44483 = ORIENTED_EDGE ( 'NONE', *, *, #17395, .F. ) ;
#44484 = VERTEX_POINT ( 'NONE', #23686 ) ;
#44485 = EDGE_LOOP ( 'NONE', ( #12534, #25833, #13096, #24506 ) ) ;
#44486 = EDGE_CURVE ( 'NONE', #31562, #3689, #27881, .T. ) ;
#44487 = DIRECTION ( 'NONE',  ( -0.1476465640024918202, 0.000000000000000000, 0.9890401873221624784 ) ) ;
#44488 = CARTESIAN_POINT ( 'NONE',  ( -336.3521761649654422, -106.8245764869328980, 56.65561927337994064 ) ) ;
#44489 = FACE_OUTER_BOUND ( 'NONE', #32855, .T. ) ;
#44490 = EDGE_LOOP ( 'NONE', ( #26999, #38359, #10163, #38559 ) ) ;
#44491 = ORIENTED_EDGE ( 'NONE', *, *, #5168, .F. ) ;
#44492 = ORIENTED_EDGE ( 'NONE', *, *, #17072, .T. ) ;
#44493 = DIRECTION ( 'NONE',  ( -1.000000000000000000, -0.000000000000000000, -0.000000000000000000 ) ) ;
#44494 = DIRECTION ( 'NONE',  ( 0.9960498426152158968, 0.000000000000000000, 0.08879589532294571153 ) ) ;
#44496 = ORIENTED_EDGE ( 'NONE', *, *, #6016, .F. ) ;
#44495 = LINE ( 'NONE', #36340, #45964 ) ;
#44497 = AXIS2_PLACEMENT_3D ( 'NONE', #10223, #45996, #26505 ) ;
#44498 = LINE ( 'NONE', #28702, #16140 ) ;
#44499 = PLANE ( 'NONE',  #40675 ) ;
#44500 = ORIENTED_EDGE ( 'NONE', *, *, #17883, .F. ) ;
#44501 = LINE ( 'NONE', #8484, #18804 ) ;
#44502 = LINE ( 'NONE', #8487, #12321 ) ;
#44503 = PLANE ( 'NONE',  #28973 ) ;
#44504 = DIRECTION ( 'NONE',  ( 1.000000000000000000, -0.000000000000000000, 0.000000000000000000 ) ) ;
#44505 = ORIENTED_EDGE ( 'NONE', *, *, #45194, .F. ) ;
#44506 = VERTEX_POINT ( 'NONE', #47881 ) ;
#44507 = DIRECTION ( 'NONE',  ( 0.000000000000000000, 0.000000000000000000, 1.000000000000000000 ) ) ;
#44508 = DIRECTION ( 'NONE',  ( -0.000000000000000000, -1.000000000000000000, 0.000000000000000000 ) ) ;
#44509 = ORIENTED_EDGE ( 'NONE', *, *, #5067, .T. ) ;
#44510 = PLANE ( 'NONE',  #36636 ) ;
#44511 = DIRECTION ( 'NONE',  ( 0.000000000000000000, -0.000000000000000000, -1.000000000000000000 ) ) ;
#44512 = EDGE_CURVE ( 'NONE', #2310, #47870, #34555, .T. ) ;
#44513 = EDGE_CURVE ( 'NONE', #38668, #10865, #20264, .T. ) ;
#44514 = ORIENTED_EDGE ( 'NONE', *, *, #15202, .F. ) ;
#44515 = LINE ( 'NONE', #3531, #43527 ) ;
#44516 = CARTESIAN_POINT ( 'NONE',  ( -48.59739992243020623, -175.3837268820161057, -0.9929810960135115883 ) ) ;
#44517 = AXIS2_PLACEMENT_3D ( 'NONE', #22973, #6442, #30082 ) ;
#44518 = VECTOR ( 'NONE', #48934, 1000.000000000000000 ) ;
#44519 = ORIENTED_EDGE ( 'NONE', *, *, #9588, .F. ) ;
#44520 = DIRECTION ( 'NONE',  ( 0.4566292373937200777, 0.000000000000000000, -0.8896570909947436601 ) ) ;
#44521 = ORIENTED_EDGE ( 'NONE', *, *, #42030, .T. ) ;
#44522 = DIRECTION ( 'NONE',  ( -0.000000000000000000, 0.000000000000000000, -1.000000000000000000 ) ) ;
#44523 = VERTEX_POINT ( 'NONE', #44453 ) ;
#44524 = LINE ( 'NONE', #32693, #1341 ) ;
#44525 = PLANE ( 'NONE',  #16341 ) ;
#44526 = LINE ( 'NONE', #36118, #9807 ) ;
#44527 = ADVANCED_FACE ( 'NONE', ( #7911 ), #23946, .F. ) ;
#44528 = DIRECTION ( 'NONE',  ( -1.000000000000000000, -0.000000000000000000, 0.000000000000000000 ) ) ;
#44529 = EDGE_CURVE ( 'NONE', #5680, #33758, #32091, .T. ) ;
#44530 = ORIENTED_EDGE ( 'NONE', *, *, #24585, .F. ) ;
#44531 = LINE ( 'NONE', #651, #24501 ) ;
#44532 = VERTEX_POINT ( 'NONE', #44710 ) ;
#44533 = VERTEX_POINT ( 'NONE', #12103 ) ;
#44534 = EDGE_CURVE ( 'NONE', #22690, #23646, #41276, .T. ) ;
#44535 = AXIS2_PLACEMENT_3D ( 'NONE', #1757, #45928, #33305 ) ;
#44536 = LINE ( 'NONE', #8521, #21840 ) ;
#44538 = ORIENTED_EDGE ( 'NONE', *, *, #6777, .T. ) ;
#44537 = CARTESIAN_POINT ( 'NONE',  ( -146.8460685364478309, -193.5000000000000000, 75.49882471933938177 ) ) ;
#44539 = EDGE_CURVE ( 'NONE', #38792, #1503, #51557, .T. ) ;
#44540 = ORIENTED_EDGE ( 'NONE', *, *, #25364, .T. ) ;
#44541 = DIRECTION ( 'NONE',  ( -0.000000000000000000, 1.000000000000000000, -0.000000000000000000 ) ) ;
#44542 = LINE ( 'NONE', #8529, #27089 ) ;
#44543 = EDGE_CURVE ( 'NONE', #15537, #1436, #8186, .T. ) ;
#44544 = LINE ( 'NONE', #51662, #12535 ) ;
#44545 = EDGE_LOOP ( 'NONE', ( #8099, #33884, #41420, #14361 ) ) ;
#44546 = CARTESIAN_POINT ( 'NONE',  ( -170.0000000000000284, -113.5000000000000142, 39.99999999999998579 ) ) ;
#44547 = EDGE_LOOP ( 'NONE', ( #22133, #3674, #40461, #29492 ) ) ;
#44548 = FACE_OUTER_BOUND ( 'NONE', #20349, .T. ) ;
#44549 = FACE_OUTER_BOUND ( 'NONE', #42901, .T. ) ;
#44550 = CIRCLE ( 'NONE', #32047, 125.0000000000000000 ) ;
#44551 = PLANE ( 'NONE',  #48746 ) ;
#44552 = CARTESIAN_POINT ( 'NONE',  ( 60.00000000000001421, -63.50000000000000000, 0.000000000000000000 ) ) ;
#44553 = ORIENTED_EDGE ( 'NONE', *, *, #18740, .T. ) ;
#44554 = EDGE_LOOP ( 'NONE', ( #8480, #43487, #25081, #11217 ) ) ;
#44556 = ORIENTED_EDGE ( 'NONE', *, *, #2023, .F. ) ;
#44555 = AXIS2_PLACEMENT_3D ( 'NONE', #42259, #37806, #34391 ) ;
#44557 = LINE ( 'NONE', #27488, #21567 ) ;
#44558 = LINE ( 'NONE', #5148, #8358 ) ;
#44559 = CARTESIAN_POINT ( 'NONE',  ( -336.3521761649654422, -106.5990858529439578, 57.57047073799066794 ) ) ;
#44560 = FACE_BOUND ( 'NONE', #28643, .T. ) ;
#44561 = CARTESIAN_POINT ( 'NONE',  ( 43.63512310656542326, -175.3837268820161057, 84.49831343337136502 ) ) ;
#44562 = VERTEX_POINT ( 'NONE', #40229 ) ;
#44563 = ORIENTED_EDGE ( 'NONE', *, *, #14581, .F. ) ;
#44565 = ORIENTED_EDGE ( 'NONE', *, *, #7064, .T. ) ;
#44564 = DIRECTION ( 'NONE',  ( 0.000000000000000000, -0.8854560256532126861, -0.4647231720437631775 ) ) ;
#44566 = EDGE_LOOP ( 'NONE', ( #40638, #40409, #2557, #16179 ) ) ;
#44567 = VECTOR ( 'NONE', #34834, 1000.000000000000000 ) ;
#44568 = CARTESIAN_POINT ( 'NONE',  ( 38.71172987070728055, -193.5000000000000000, -89.56983042009262874 ) ) ;
#44569 = CARTESIAN_POINT ( 'NONE',  ( -92.16375985330358844, -189.7472609257535510, 117.1181148702521710 ) ) ;
#44570 = EDGE_CURVE ( 'NONE', #38201, #49836, #290, .T. ) ;
#44571 = LINE ( 'NONE', #12514, #38895 ) ;
#44572 = ADVANCED_FACE ( 'NONE', ( #21051, #1848 ), #5036, .T. ) ;
#44573 = EDGE_CURVE ( 'NONE', #15652, #40282, #26028, .T. ) ;
#44574 = DIRECTION ( 'NONE',  ( 0.000000000000000000, 0.000000000000000000, 1.000000000000000000 ) ) ;
#44575 = EDGE_LOOP ( 'NONE', ( #10073, #16208, #25699, #5518 ) ) ;
#44576 = DIRECTION ( 'NONE',  ( -0.5586467658036594619, 0.000000000000000000, 0.8294056854501971054 ) ) ;
#44577 = ORIENTED_EDGE ( 'NONE', *, *, #28252, .F. ) ;
#44578 = EDGE_CURVE ( 'NONE', #37802, #33969, #25509, .T. ) ;
#44579 = VERTEX_POINT ( 'NONE', #10016 ) ;
#44580 = DIRECTION ( 'NONE',  ( -0.9151456172430237901, 0.000000000000000000, 0.4031234292879600778 ) ) ;
#44581 = ADVANCED_FACE ( 'NONE', ( #33652 ), #29974, .F. ) ;
#44582 = CARTESIAN_POINT ( 'NONE',  ( -48.93575598890255662, -175.3837268820161057, -0.8896570909947461026 ) ) ;
#44583 = DIRECTION ( 'NONE',  ( 0.000000000000000000, 0.000000000000000000, 1.000000000000000000 ) ) ;
#44584 = DIRECTION ( 'NONE',  ( 0.000000000000000000, 0.000000000000000000, 1.000000000000000000 ) ) ;
#44585 = CARTESIAN_POINT ( 'NONE',  ( -156.7610986364826999, -183.6283474603465606, -62.45009659481510766 ) ) ;
#44586 = DIRECTION ( 'NONE',  ( -0.000000000000000000, 1.000000000000000000, -0.000000000000000000 ) ) ;
#44587 = ADVANCED_FACE ( 'NONE', ( #41526 ), #16862, .F. ) ;
#44588 = ORIENTED_EDGE ( 'NONE', *, *, #40693, .T. ) ;
#44589 = CARTESIAN_POINT ( 'NONE',  ( -48.47912675150885065, -189.7472609257535510, 6.938893903907228378E-15 ) ) ;
#44590 = CARTESIAN_POINT ( 'NONE',  ( -40.90423906728906900, -189.7472609257535510, -124.7702732086912505 ) ) ;
#44591 = EDGE_CURVE ( 'NONE', #37488, #34495, #33414, .T. ) ;
#44592 = AXIS2_PLACEMENT_3D ( 'NONE', #23586, #39088, #39600 ) ;
#44593 = FACE_OUTER_BOUND ( 'NONE', #14092, .T. ) ;
#44594 = FACE_BOUND ( 'NONE', #49082, .T. ) ;
#44595 = EDGE_LOOP ( 'NONE', ( #5621, #22712, #7984, #24505 ) ) ;
#44596 = ADVANCED_FACE ( 'NONE', ( #29704 ), #9744, .T. ) ;
#44597 = AXIS2_PLACEMENT_3D ( 'NONE', #17984, #45839, #21132 ) ;
#44598 = FACE_OUTER_BOUND ( 'NONE', #31618, .T. ) ;
#44599 = EDGE_LOOP ( 'NONE', ( #19859, #50881, #9318, #14354 ) ) ;
#44600 = CARTESIAN_POINT ( 'NONE',  ( -339.1964088526558498, -143.9541802141663709, 55.34326076196097688 ) ) ;
#44601 = EDGE_CURVE ( 'NONE', #4155, #16698, #12753, .T. ) ;
#44602 = VERTEX_POINT ( 'NONE', #1068 ) ;
#44603 = LINE ( 'NONE', #23846, #38035 ) ;
#44604 = ORIENTED_EDGE ( 'NONE', *, *, #33529, .F. ) ;
#44605 = ADVANCED_FACE ( 'NONE', ( #37332 ), #25775, .F. ) ;
#44606 = CARTESIAN_POINT ( 'NONE',  ( -48.47912675150885065, -189.7472609257535510, 6.938893903907228378E-15 ) ) ;
#44607 = VECTOR ( 'NONE', #33170, 1000.000000000000000 ) ;
#44608 = FACE_BOUND ( 'NONE', #26881, .T. ) ;
#44610 = ORIENTED_EDGE ( 'NONE', *, *, #37849, .F. ) ;
#44609 = DIRECTION ( 'NONE',  ( 0.000000000000000000, 0.000000000000000000, -1.000000000000000000 ) ) ;
#44611 = CARTESIAN_POINT ( 'NONE',  ( -213.8817838414232426, -213.5000000000000000, 10.00000000000002842 ) ) ;
#44612 = EDGE_CURVE ( 'NONE', #39243, #26852, #9234, .T. ) ;
#44613 = ORIENTED_EDGE ( 'NONE', *, *, #36803, .F. ) ;
#44614 = ORIENTED_EDGE ( 'NONE', *, *, #44474, .T. ) ;
#44615 = DIRECTION ( 'NONE',  ( 0.000000000000000000, -0.000000000000000000, 1.000000000000000000 ) ) ;
#44616 = VERTEX_POINT ( 'NONE', #33129 ) ;
#44617 = LINE ( 'NONE', #49608, #25928 ) ;
#44618 = LINE ( 'NONE', #25175, #44650 ) ;
#44619 = DIRECTION ( 'NONE',  ( 0.000000000000000000, -1.000000000000000000, 0.000000000000000000 ) ) ;
#44620 = VECTOR ( 'NONE', #4325, 1000.000000000000000 ) ;
#44621 = AXIS2_PLACEMENT_3D ( 'NONE', #43739, #19064, #31136 ) ;
#44622 = VECTOR ( 'NONE', #36847, 1000.000000000000114 ) ;
#44623 = LINE ( 'NONE', #28836, #29268 ) ;
#44624 = EDGE_CURVE ( 'NONE', #16474, #31485, #5555, .T. ) ;
#44625 = DIRECTION ( 'NONE',  ( -0.000000000000000000, -0.7485107481711024136, -0.6631226582407937498 ) ) ;
#44626 = ORIENTED_EDGE ( 'NONE', *, *, #24697, .T. ) ;
#44629 = ORIENTED_EDGE ( 'NONE', *, *, #6815, .T. ) ;
#44628 = CARTESIAN_POINT ( 'NONE',  ( -172.7479958471414250, -177.1207230881787780, -13.49993235881364129 ) ) ;
#44627 = DIRECTION ( 'NONE',  ( -0.7378332790417285736, 0.000000000000000000, 0.6749830015182091136 ) ) ;
#44630 = ORIENTED_EDGE ( 'NONE', *, *, #39358, .T. ) ;
#44631 = DIRECTION ( 'NONE',  ( 0.000000000000000000, 0.000000000000000000, 1.000000000000000000 ) ) ;
#44632 = ORIENTED_EDGE ( 'NONE', *, *, #31630, .F. ) ;
#44633 = DIRECTION ( 'NONE',  ( 0.000000000000000000, 1.000000000000000000, -0.000000000000000000 ) ) ;
#44634 = EDGE_LOOP ( 'NONE', ( #42400, #28377, #14799, #31008 ) ) ;
#44635 = EDGE_CURVE ( 'NONE', #15096, #39780, #6884, .T. ) ;
#44636 = DIRECTION ( 'NONE',  ( -0.2348860457809842095, 0.000000000000000000, 0.9720229140804107493 ) ) ;
#44637 = ADVANCED_FACE ( 'NONE', ( #1610, #13175, #25256, #48919 ), #17892, .F. ) ;
#44638 = DIRECTION ( 'NONE',  ( 0.000000000000000000, 0.000000000000000000, 1.000000000000000000 ) ) ;
#44639 = ORIENTED_EDGE ( 'NONE', *, *, #11473, .T. ) ;
#44641 = DIRECTION ( 'NONE',  ( 0.000000000000000000, 0.000000000000000000, -1.000000000000000000 ) ) ;
#44640 = CARTESIAN_POINT ( 'NONE',  ( -330.4913330509368166, -151.8251501453679850, 52.89315522109040302 ) ) ;
#44642 = ORIENTED_EDGE ( 'NONE', *, *, #6449, .F. ) ;
#44643 = VECTOR ( 'NONE', #18499, 1000.000000000000000 ) ;
#44644 = EDGE_CURVE ( 'NONE', #10381, #9360, #33906, .T. ) ;
#44645 = ADVANCED_FACE ( 'NONE', ( #13948 ), #30732, .F. ) ;
#44646 = ORIENTED_EDGE ( 'NONE', *, *, #44359, .T. ) ;
#44647 = CARTESIAN_POINT ( 'NONE',  ( -171.6469053867624837, -177.1207230881787780, -14.34663989163545850 ) ) ;
#44648 = AXIS2_PLACEMENT_3D ( 'NONE', #51412, #31415, #5855 ) ;
#44650 = VECTOR ( 'NONE', #32791, 1000.000000000000000 ) ;
#44649 = DIRECTION ( 'NONE',  ( -0.000000000000000000, 1.047444401652940007E-14, 1.000000000000000000 ) ) ;
#44651 = DIRECTION ( 'NONE',  ( 0.000000000000000000, -1.000000000000000000, 0.000000000000000000 ) ) ;
#44652 = FACE_OUTER_BOUND ( 'NONE', #45788, .T. ) ;
#44653 = LINE ( 'NONE', #36484, #8955 ) ;
#44654 = CARTESIAN_POINT ( 'NONE',  ( -332.3517673607765914, -164.5945333327934463, -42.41660376256285048 ) ) ;
#44655 = APPLICATION_PROTOCOL_DEFINITION ( 'draft international standard', 'automotive_design', 1998, #8866 ) ;
#44656 = DIRECTION ( 'NONE',  ( 0.7378332790417285736, 0.000000000000000000, -0.6749830015182091136 ) ) ;
#44657 = LINE ( 'NONE', #47831, #19632 ) ;
#44658 = PLANE ( 'NONE',  #9730 ) ;
#44659 = CARTESIAN_POINT ( 'NONE',  ( 45.24245851652181472, -193.5000000000000000, -81.19354792697731682 ) ) ;
#44660 = EDGE_LOOP ( 'NONE', ( #39255, #7903, #38041, #51124 ) ) ;
#44661 = VERTEX_POINT ( 'NONE', #2102 ) ;
#44662 = FACE_OUTER_BOUND ( 'NONE', #17279, .T. ) ;
#44663 = EDGE_CURVE ( 'NONE', #33019, #33038, #20298, .T. ) ;
#44664 = AXIS2_PLACEMENT_3D ( 'NONE', #1334, #44980, #49950 ) ;
#44665 = DIRECTION ( 'NONE',  ( 0.000000000000000000, 0.000000000000000000, -1.000000000000000000 ) ) ;
#44666 = EDGE_CURVE ( 'NONE', #21902, #47743, #47045, .T. ) ;
#44667 = PLANE ( 'NONE',  #39664 ) ;
#44668 = EDGE_LOOP ( 'NONE', ( #32134, #37985, #45321, #392 ) ) ;
#44669 = VERTEX_POINT ( 'NONE', #10259 ) ;
#44670 = CIRCLE ( 'NONE', #18633, 125.0000000000000000 ) ;
#44671 = ORIENTED_EDGE ( 'NONE', *, *, #24050, .F. ) ;
#44672 = EDGE_CURVE ( 'NONE', #11150, #38873, #6835, .T. ) ;
#44673 = VECTOR ( 'NONE', #22049, 1000.000000000000227 ) ;
#44674 = DIRECTION ( 'NONE',  ( 0.000000000000000000, 1.000000000000000000, 0.000000000000000000 ) ) ;
#44675 = CARTESIAN_POINT ( 'NONE',  ( -71.40672220061269115, -193.5000000000000000, -122.8793122007208751 ) ) ;
#44676 = DIRECTION ( 'NONE',  ( 0.000000000000000000, -1.000000000000000000, 0.000000000000000000 ) ) ;
#44677 = DIRECTION ( 'NONE',  ( 0.000000000000000000, -1.000000000000000000, 0.000000000000000000 ) ) ;
#44678 = ORIENTED_EDGE ( 'NONE', *, *, #1245, .T. ) ;
#44679 = DIRECTION ( 'NONE',  ( -0.6528221181905280446, 0.000000000000000000, 0.7575112421616145841 ) ) ;
#44680 = LINE ( 'NONE', #4478, #50364 ) ;
#44681 = VECTOR ( 'NONE', #21339, 1000.000000000000000 ) ;
#44682 = VERTEX_POINT ( 'NONE', #3148 ) ;
#44683 = CIRCLE ( 'NONE', #19497, 125.0000000000000000 ) ;
#44684 = LINE ( 'NONE', #49666, #32349 ) ;
#44685 = ORIENTED_EDGE ( 'NONE', *, *, #31098, .T. ) ;
#44686 = CIRCLE ( 'NONE', #33798, 60.00000000000000000 ) ;
#44687 = CIRCLE ( 'NONE', #12783, 4.000000000000003553 ) ;
#44688 = ORIENTED_EDGE ( 'NONE', *, *, #3174, .T. ) ;
#44689 = DIRECTION ( 'NONE',  ( 0.000000000000000000, 0.000000000000000000, 1.000000000000000000 ) ) ;
#44690 = SURFACE_SIDE_STYLE ('',( #51812 ) ) ;
#44691 = CARTESIAN_POINT ( 'NONE',  ( -339.1964088526558498, -144.8891964568526305, -54.98865587491811624 ) ) ;
#44694 = ORIENTED_EDGE ( 'NONE', *, *, #18794, .T. ) ;
#44693 = CARTESIAN_POINT ( 'NONE',  ( -48.47912675150885065, -177.1207230881787780, 6.938893903907228378E-15 ) ) ;
#44692 = DIRECTION ( 'NONE',  ( -0.000000000000000000, -0.6631226582407989678, -0.7485107481710977506 ) ) ;
#44695 = DIRECTION ( 'NONE',  ( 1.043714542225393381E-14, -0.8229838658936575735, -0.5680647467311540355 ) ) ;
#44696 = ORIENTED_EDGE ( 'NONE', *, *, #12004, .T. ) ;
#44697 = LINE ( 'NONE', #16854, #3753 ) ;
#44698 = VECTOR ( 'NONE', #13887, 1000.000000000000000 ) ;
#44699 = FACE_OUTER_BOUND ( 'NONE', #33284, .T. ) ;
#44700 = ORIENTED_EDGE ( 'NONE', *, *, #37238, .F. ) ;
#44701 = EDGE_CURVE ( 'NONE', #35572, #14767, #50996, .T. ) ;
#44703 = ADVANCED_FACE ( 'NONE', ( #2382 ), #18915, .T. ) ;
#44702 = LINE ( 'NONE', #49619, #11497 ) ;
#44704 = DIRECTION ( 'NONE',  ( 0.000000000000000000, -0.000000000000000000, -1.000000000000000000 ) ) ;
#44706 = CARTESIAN_POINT ( 'NONE',  ( 61.69163308845453031, -177.1207230881787780, -56.90809649257491287 ) ) ;
#44705 = DIRECTION ( 'NONE',  ( -1.000000000000000000, 0.000000000000000000, 0.000000000000000000 ) ) ;
#44707 = EDGE_LOOP ( 'NONE', ( #11109, #40735, #16508, #36466 ) ) ;
#44708 = VECTOR ( 'NONE', #35226, 1000.000000000000000 ) ;
#44709 = FACE_OUTER_BOUND ( 'NONE', #48207, .T. ) ;
#44710 = CARTESIAN_POINT ( 'NONE',  ( -109.0835867659424565, -177.1207230881787780, -109.3256576763154726 ) ) ;
#44711 = CARTESIAN_POINT ( 'NONE',  ( 46.40005841627162653, -177.1207230881787780, 81.38144888055276738 ) ) ;
#44712 = ORIENTED_EDGE ( 'NONE', *, *, #46373, .F. ) ;
#44713 = CARTESIAN_POINT ( 'NONE',  ( -305.0000000000000568, -123.5000000000000284, 0.000000000000000000 ) ) ;
#44714 = PLANE ( 'NONE',  #9781 ) ;
#44715 = DIRECTION ( 'NONE',  ( 0.9027978299657416494, 0.000000000000000000, 0.4300652022765245608 ) ) ;
#44716 = ORIENTED_EDGE ( 'NONE', *, *, #32453, .T. ) ;
#44717 = AXIS2_PLACEMENT_3D ( 'NONE', #5455, #21473, #37495 ) ;
#44718 = PLANE ( 'NONE',  #48292 ) ;
#44719 = ORIENTED_EDGE ( 'NONE', *, *, #7346, .T. ) ;
#44720 = DIRECTION ( 'NONE',  ( 0.000000000000000000, -1.000000000000000000, -0.000000000000000000 ) ) ;
#44721 = ORIENTED_EDGE ( 'NONE', *, *, #45900, .T. ) ;
#44722 = AXIS2_PLACEMENT_3D ( 'NONE', #17001, #48277, #24875 ) ;
#44723 = CIRCLE ( 'NONE', #31277, 60.00000000000000000 ) ;
#44724 = CARTESIAN_POINT ( 'NONE',  ( 32.59960422616972409, -189.7472609257535510, -93.82025162277999186 ) ) ;
#44725 = FACE_OUTER_BOUND ( 'NONE', #867, .T. ) ;
#44726 = ADVANCED_FACE ( 'NONE', ( #10775 ), #18413, .T. ) ;
#44727 = FACE_OUTER_BOUND ( 'NONE', #49033, .T. ) ;
#44728 = DIRECTION ( 'NONE',  ( -1.000000000000000000, -0.000000000000000000, -0.000000000000000000 ) ) ;
#44729 = DIRECTION ( 'NONE',  ( 0.000000000000000000, 0.000000000000000000, 1.000000000000000000 ) ) ;
#44730 = VECTOR ( 'NONE', #41767, 1000.000000000000000 ) ;
#44731 = EDGE_CURVE ( 'NONE', #30632, #40004, #11272, .T. ) ;
#44732 = DIRECTION ( 'NONE',  ( -0.3482016354343995812, 0.000000000000000000, 0.9374196611341205632 ) ) ;
#44733 = CARTESIAN_POINT ( 'NONE',  ( -49.38192458147459973, -193.5000000000000000, 0.4300652022765185656 ) ) ;
#44734 = DIRECTION ( 'NONE',  ( 1.000000000000000000, -0.000000000000000000, 0.000000000000000000 ) ) ;
#44736 = VERTEX_POINT ( 'NONE', #6319 ) ;
#44735 = LINE ( 'NONE', #17144, #21981 ) ;
#44737 = VECTOR ( 'NONE', #33786, 1000.000000000000114 ) ;
#44738 = ORIENTED_EDGE ( 'NONE', *, *, #27572, .T. ) ;
#44739 = PLANE ( 'NONE',  #39213 ) ;
#44740 = ADVANCED_FACE ( 'NONE', ( #14470 ), #22083, .T. ) ;
#44741 = VECTOR ( 'NONE', #34767, 1000.000000000000114 ) ;
#44742 = LINE ( 'NONE', #40000, #21266 ) ;
#44743 = VERTEX_POINT ( 'NONE', #22613 ) ;
#44744 = ORIENTED_EDGE ( 'NONE', *, *, #19532, .F. ) ;
#44745 = VERTEX_POINT ( 'NONE', #27309 ) ;
#44746 = CARTESIAN_POINT ( 'NONE',  ( -48.47912675150885065, -175.3837268820161057, 6.938893903907228378E-15 ) ) ;
#44747 = DIRECTION ( 'NONE',  ( 0.000000000000000000, 0.000000000000000000, 1.000000000000000000 ) ) ;
#44748 = PLANE ( 'NONE',  #28307 ) ;
#44750 = ORIENTED_EDGE ( 'NONE', *, *, #34059, .F. ) ;
#44749 = VECTOR ( 'NONE', #494, 1000.000000000000000 ) ;
#44751 = VECTOR ( 'NONE', #15149, 999.9999999999998863 ) ;
#44752 = VERTEX_POINT ( 'NONE', #14216 ) ;
#44753 = EDGE_CURVE ( 'NONE', #6309, #28688, #50475, .T. ) ;
#44754 = CARTESIAN_POINT ( 'NONE',  ( -131.8938452225253855, -177.1207230881787780, 93.09664195018558530 ) ) ;
#44755 = PLANE ( 'NONE',  #50383 ) ;
#44757 = ORIENTED_EDGE ( 'NONE', *, *, #23754, .T. ) ;
#44756 = PLANE ( 'NONE',  #7347 ) ;
#44758 = AXIS2_PLACEMENT_3D ( 'NONE', #49975, #10036, #5576 ) ;
#44759 = DIRECTION ( 'NONE',  ( 0.000000000000000000, -1.000000000000000000, 0.000000000000000000 ) ) ;
#44760 = CYLINDRICAL_SURFACE ( 'NONE', #23913, 125.0000000000000000 ) ;
#44761 = ORIENTED_EDGE ( 'NONE', *, *, #19564, .T. ) ;
#44762 = FACE_OUTER_BOUND ( 'NONE', #31465, .T. ) ;
#44763 = EDGE_LOOP ( 'NONE', ( #14890, #49445, #31483, #23238 ) ) ;
#44764 = ADVANCED_FACE ( 'NONE', ( #38371 ), #26796, .F. ) ;
#44765 = AXIS2_PLACEMENT_3D ( 'NONE', #4656, #16230, #19910 ) ;
#44766 = CARTESIAN_POINT ( 'NONE',  ( -330.4913330509368166, -175.9742670995615015, -26.97593913775547136 ) ) ;
#44767 = EDGE_CURVE ( 'NONE', #49365, #7639, #38882, .T. ) ;
#44768 = CARTESIAN_POINT ( 'NONE',  ( -161.4019114581581391, -189.7472609257535510, 53.60452120946272458 ) ) ;
#44769 = LINE ( 'NONE', #32674, #8968 ) ;
#44770 = ORIENTED_EDGE ( 'NONE', *, *, #3683, .F. ) ;
#44771 = ADVANCED_FACE ( 'NONE', ( #10503 ), #2626, .T. ) ;
#44772 = ORIENTED_EDGE ( 'NONE', *, *, #7927, .F. ) ;
#44773 = DIRECTION ( 'NONE',  ( 0.000000000000000000, -1.000000000000000000, 0.000000000000000000 ) ) ;
#44774 = DIRECTION ( 'NONE',  ( 0.000000000000000000, 1.000000000000000000, 0.000000000000000000 ) ) ;
#44775 = EDGE_LOOP ( 'NONE', ( #35698, #9416, #43306, #22012 ) ) ;
#44776 = CARTESIAN_POINT ( 'NONE',  ( -52.47502265695602119, -177.1207230881787780, -124.9361149384469485 ) ) ;
#44777 = VECTOR ( 'NONE', #15901, 1000.000000000000227 ) ;
#44778 = DIRECTION ( 'NONE',  ( -0.000000000000000000, 1.000000000000000000, -0.000000000000000000 ) ) ;
#44779 = ORIENTED_EDGE ( 'NONE', *, *, #44439, .F. ) ;
#44780 = CARTESIAN_POINT ( 'NONE',  ( -105.2524431885210703, -189.7472609257535510, 110.2396968984195382 ) ) ;
#44781 = DIRECTION ( 'NONE',  ( 1.000000000000000000, -0.000000000000000000, -0.000000000000000000 ) ) ;
#44782 = EDGE_LOOP ( 'NONE', ( #42299, #34849 ) ) ;
#44783 = DIRECTION ( 'NONE',  ( -0.000000000000000000, 1.000000000000000000, -0.000000000000000000 ) ) ;
#44784 = ORIENTED_EDGE ( 'NONE', *, *, #30759, .F. ) ;
#44785 = CARTESIAN_POINT ( 'NONE',  ( -170.7635349987907603, -193.5000000000000000, -25.91377046305877130 ) ) ;
#44786 = EDGE_CURVE ( 'NONE', #28153, #34735, #51251, .T. ) ;
#44787 = ORIENTED_EDGE ( 'NONE', *, *, #3640, .T. ) ;
#44788 = EDGE_CURVE ( 'NONE', #22822, #13519, #46363, .T. ) ;
#44789 = DIRECTION ( 'NONE',  ( 0.8757349421956310831, 0.000000000000000000, 0.4827922027307550712 ) ) ;
#44790 = LINE ( 'NONE', #41883, #38980 ) ;
#44791 = DIRECTION ( 'NONE',  ( -0.000000000000000000, 1.000000000000000000, -0.000000000000000000 ) ) ;
#44792 = PLANE ( 'NONE',  #29942 ) ;
#44793 = ORIENTED_EDGE ( 'NONE', *, *, #7905, .T. ) ;
#44794 = CARTESIAN_POINT ( 'NONE',  ( -38.66762320617017679, -183.6283474603465606, -124.6143426664033740 ) ) ;
#44795 = EDGE_LOOP ( 'NONE', ( #1132, #25107, #5983, #51295 ) ) ;
#44796 = APPLICATION_CONTEXT ( 'automotive_design' ) ;
#44797 = VERTEX_POINT ( 'NONE', #19180 ) ;
#44798 = VECTOR ( 'NONE', #30660, 1000.000000000000000 ) ;
#44799 = CARTESIAN_POINT ( 'NONE',  ( -330.4913330509368166, -151.3613951634084742, 52.00954392751779665 ) ) ;
#44801 = VERTEX_POINT ( 'NONE', #23624 ) ;
#44800 = CARTESIAN_POINT ( 'NONE',  ( -47.92047998570520662, -177.1207230881787780, 0.8294056854502119824 ) ) ;
#44802 = ORIENTED_EDGE ( 'NONE', *, *, #3513, .F. ) ;
#44803 = CARTESIAN_POINT ( 'NONE',  ( -48.77118352214583297, -183.6283474603465606, 0.9564009842765270886 ) ) ;
#44804 = CARTESIAN_POINT ( 'NONE',  ( -339.1964088526558498, -70.14212160686578557, 27.43969411971455585 ) ) ;
#44805 = ORIENTED_EDGE ( 'NONE', *, *, #11561, .F. ) ;
#44806 = DIRECTION ( 'NONE',  ( -0.000000000000000000, 1.000000000000000000, -0.000000000000000000 ) ) ;
#44807 = VERTEX_POINT ( 'NONE', #51764 ) ;
#44808 = DIRECTION ( 'NONE',  ( 0.000000000000000000, 0.000000000000000000, -1.000000000000000000 ) ) ;
#44809 = DIRECTION ( 'NONE',  ( 0.000000000000000000, -1.000000000000000000, -0.000000000000000000 ) ) ;
#44810 = VECTOR ( 'NONE', #8394, 999.9999999999998863 ) ;
#44811 = EDGE_CURVE ( 'NONE', #20535, #9367, #21177, .T. ) ;
#44812 = LINE ( 'NONE', #20369, #12666 ) ;
#44813 = CARTESIAN_POINT ( 'NONE',  ( -365.0000000000001137, -168.5000000000000284, 0.000000000000000000 ) ) ;
#44814 = ORIENTED_EDGE ( 'NONE', *, *, #10464, .T. ) ;
#44815 = ORIENTED_EDGE ( 'NONE', *, *, #15225, .F. ) ;
#44816 = AXIS2_PLACEMENT_3D ( 'NONE', #44343, #8068, #48276 ) ;
#44817 = ORIENTED_EDGE ( 'NONE', *, *, #30459, .F. ) ;
#44818 = LINE ( 'NONE', #9856, #23253 ) ;
#44819 = DIRECTION ( 'NONE',  ( -0.000000000000000000, 1.000000000000000000, -0.000000000000000000 ) ) ;
#44820 = FACE_OUTER_BOUND ( 'NONE', #25035, .T. ) ;
#44821 = FACE_BOUND ( 'NONE', #41045, .T. ) ;
#44822 = FACE_OUTER_BOUND ( 'NONE', #32351, .T. ) ;
#44823 = ORIENTED_EDGE ( 'NONE', *, *, #41272, .F. ) ;
#44824 = ADVANCED_FACE ( 'NONE', ( #4190 ), #11549, .T. ) ;
#44825 = AXIS2_PLACEMENT_3D ( 'NONE', #19929, #44619, #35961 ) ;
#44826 = ADVANCED_FACE ( 'NONE', ( #47564 ), #43606, .F. ) ;
#44827 = ORIENTED_EDGE ( 'NONE', *, *, #1573, .F. ) ;
#44829 = VERTEX_POINT ( 'NONE', #15778 ) ;
#44828 = DIRECTION ( 'NONE',  ( 0.000000000000000000, -0.5680647467311457088, 0.8229838658936633466 ) ) ;
#44830 = EDGE_LOOP ( 'NONE', ( #25603, #14857, #31880, #1026 ) ) ;
#44831 = EDGE_CURVE ( 'NONE', #12470, #19399, #16541, .T. ) ;
#44832 = CARTESIAN_POINT ( 'NONE',  ( -154.6193097927903182, -175.3837268820161057, -66.02470404298124151 ) ) ;
#44833 = EDGE_CURVE ( 'NONE', #43316, #37774, #15499, .T. ) ;
#44834 = CARTESIAN_POINT ( 'NONE',  ( -170.0000000000000284, -173.5000000000000284, -60.00000000000001421 ) ) ;
#44835 = DIRECTION ( 'NONE',  ( 0.000000000000000000, 1.000000000000000000, 0.000000000000000000 ) ) ;
#44836 = DIRECTION ( 'NONE',  ( 1.000000000000000000, 0.000000000000000000, 8.718379230999705894E-17 ) ) ;
#44837 = EDGE_LOOP ( 'NONE', ( #31557, #25633, #30297, #35142 ) ) ;
#44838 = CARTESIAN_POINT ( 'NONE',  ( -154.2693405752510500, -189.7472609257535510, 66.58401203837827609 ) ) ;
#44839 = EDGE_LOOP ( 'NONE', ( #50007, #33992 ) ) ;
#44840 = ORIENTED_EDGE ( 'NONE', *, *, #38428, .T. ) ;
#44841 = DIRECTION ( 'NONE',  ( 0.000000000000000000, 0.000000000000000000, -1.000000000000000000 ) ) ;
#44842 = LINE ( 'NONE', #45378, #14400 ) ;
#44843 = DIRECTION ( 'NONE',  ( 0.000000000000000000, 0.000000000000000000, 1.000000000000000000 ) ) ;
#44844 = AXIS2_PLACEMENT_3D ( 'NONE', #26335, #46325, #22143 ) ;
#44845 = LINE ( 'NONE', #32757, #7142 ) ;
#44846 = VECTOR ( 'NONE', #50932, 1000.000000000000000 ) ;
#44847 = DIRECTION ( 'NONE',  ( -1.000000000000000000, -0.000000000000000000, -0.000000000000000000 ) ) ;
#44848 = CARTESIAN_POINT ( 'NONE',  ( -330.4913330509368166, -172.3400804610910200, 33.10432812419180948 ) ) ;
#44849 = CARTESIAN_POINT ( 'NONE',  ( -124.4642912599203726, -175.3837268820161057, 99.25348746834863789 ) ) ;
#44850 = VERTEX_POINT ( 'NONE', #32025 ) ;
#44851 = PLANE ( 'NONE',  #5395 ) ;
#44852 = CARTESIAN_POINT ( 'NONE',  ( -169.6464974000608379, -193.5000000000000000, 26.35287080855540154 ) ) ;
#44853 = AXIS2_PLACEMENT_3D ( 'NONE', #13767, #32694, #20887 ) ;
#44854 = CARTESIAN_POINT ( 'NONE',  ( -336.3521761649654422, -107.7955183043589500, 56.89493493766750731 ) ) ;
#44855 = FACE_BOUND ( 'NONE', #2410, .T. ) ;
#44856 = ORIENTED_EDGE ( 'NONE', *, *, #12695, .T. ) ;
#44857 = DIRECTION ( 'NONE',  ( 1.000000000000000000, -0.000000000000000000, -0.000000000000000000 ) ) ;
#44858 = ORIENTED_EDGE ( 'NONE', *, *, #45601, .T. ) ;
#44859 = CARTESIAN_POINT ( 'NONE',  ( 0.000000000000000000, -130.6116641350643022, -58.56982357178517873 ) ) ;
#44860 = ORIENTED_EDGE ( 'NONE', *, *, #32356, .F. ) ;
#44861 = CARTESIAN_POINT ( 'NONE',  ( -332.3517673607765914, -149.4733471526596134, 53.00046796564699036 ) ) ;
#44862 = VECTOR ( 'NONE', #10891, 1000.000000000000227 ) ;
#44863 = ORIENTED_EDGE ( 'NONE', *, *, #20547, .F. ) ;
#44864 = PRODUCT_DEFINITION_SHAPE ( 'NONE', 'NONE',  #52041 ) ;
#44865 = PLANE ( 'NONE',  #42738 ) ;
#44866 = CARTESIAN_POINT ( 'NONE',  ( -336.3521761649654422, -155.6724726690323450, 49.48329383994676078 ) ) ;
#44868 = VERTEX_POINT ( 'NONE', #28075 ) ;
#44867 = LINE ( 'NONE', #9643, #38849 ) ;
#44869 = EDGE_CURVE ( 'NONE', #11668, #25203, #47823, .T. ) ;
#44870 = ADVANCED_FACE ( 'NONE', ( #20461 ), #31508, .F. ) ;
#44871 = EDGE_CURVE ( 'NONE', #34929, #20197, #1893, .T. ) ;
#44872 = CARTESIAN_POINT ( 'NONE',  ( -330.4913330509368166, -137.1341532842523918, 57.40522506028099770 ) ) ;
#44873 = EDGE_LOOP ( 'NONE', ( #41886, #5382, #27244, #36697 ) ) ;
#44874 = ADVANCED_FACE ( 'NONE', ( #40174 ), #11793, .T. ) ;
#44875 = ORIENTED_EDGE ( 'NONE', *, *, #1414, .F. ) ;
#44876 = DIRECTION ( 'NONE',  ( 0.5586467658036476935, 0.000000000000000000, 0.8294056854502049880 ) ) ;
#44877 = CARTESIAN_POINT ( 'NONE',  ( -134.9506378406916554, -193.5000000000000000, 90.26448786734091811 ) ) ;
#44878 = EDGE_LOOP ( 'NONE', ( #41524, #48367, #29522, #28339 ) ) ;
#44879 = CARTESIAN_POINT ( 'NONE',  ( -305.0000000000000568, -96.06030588028460215, -53.35787839313380232 ) ) ;
#44880 = ADVANCED_FACE ( 'NONE', ( #43856 ), #7856, .T. ) ;
#44881 = VECTOR ( 'NONE', #9221, 1000.000000000000000 ) ;
#44882 = CARTESIAN_POINT ( 'NONE',  ( 73.32083127613157103, -193.5000000000000000, 28.10285082451656535 ) ) ;
#44883 = LINE ( 'NONE', #13348, #45661 ) ;
#44884 = AXIS2_PLACEMENT_3D ( 'NONE', #7608, #35993, #20214 ) ;
#44885 = EDGE_CURVE ( 'NONE', #44797, #27513, #3927, .T. ) ;
#44886 = AXIS2_PLACEMENT_3D ( 'NONE', #51326, #16097, #32109 ) ;
#44887 = EDGE_CURVE ( 'NONE', #8253, #18899, #48605, .T. ) ;
#44888 = CARTESIAN_POINT ( 'NONE',  ( -48.18706998087187543, -175.3837268820161057, -0.9564009842765152092 ) ) ;
#44889 = CARTESIAN_POINT ( 'NONE',  ( -44.48323084606168720, -193.5000000000000000, 123.9361149384469769 ) ) ;
#44890 = EDGE_LOOP ( 'NONE', ( #25556, #49554, #10962, #37483 ) ) ;
#44893 = ORIENTED_EDGE ( 'NONE', *, *, #35916, .T. ) ;
#44892 = DIRECTION ( 'NONE',  ( 0.000000000000000000, -1.000000000000000000, 0.000000000000000000 ) ) ;
#44891 = FACE_OUTER_BOUND ( 'NONE', #20950, .T. ) ;
#44894 = ORIENTED_EDGE ( 'NONE', *, *, #20427, .F. ) ;
#44895 = EDGE_CURVE ( 'NONE', #42517, #6623, #35985, .T. ) ;
#44896 = AXIS2_PLACEMENT_3D ( 'NONE', #23867, #48589, #12566 ) ;
#44897 = LINE ( 'NONE', #32014, #34865 ) ;
#44898 = ORIENTED_EDGE ( 'NONE', *, *, #3814, .T. ) ;
#44899 = CARTESIAN_POINT ( 'NONE',  ( -137.6740394605055826, -193.5000000000000000, -86.14171647324862136 ) ) ;
#44900 = VERTEX_POINT ( 'NONE', #48067 ) ;
#44901 = EDGE_CURVE ( 'NONE', #26369, #13489, #40422, .T. ) ;
#44902 = CARTESIAN_POINT ( 'NONE',  ( 0.000000000000000000, -43.50000000000000000, 0.000000000000000000 ) ) ;
#44903 = DIRECTION ( 'NONE',  ( 0.000000000000000000, -1.000000000000000000, 0.000000000000000000 ) ) ;
#44904 = ORIENTED_EDGE ( 'NONE', *, *, #32353, .T. ) ;
#44905 = DIRECTION ( 'NONE',  ( 1.000000000000000000, -0.000000000000000000, -0.000000000000000000 ) ) ;
#44906 = VECTOR ( 'NONE', #19796, 999.9999999999998863 ) ;
#44907 = EDGE_LOOP ( 'NONE', ( #50337, #26624, #16070, #10609 ) ) ;
#44908 = ORIENTED_EDGE ( 'NONE', *, *, #14112, .F. ) ;
#44909 = FACE_OUTER_BOUND ( 'NONE', #40169, .T. ) ;
#44910 = FACE_OUTER_BOUND ( 'NONE', #9267, .T. ) ;
#44911 = PLANE ( 'NONE',  #27198 ) ;
#44912 = CARTESIAN_POINT ( 'NONE',  ( -48.47912675150885065, -175.3837268820161057, 6.938893903907228378E-15 ) ) ;
#44913 = ORIENTED_EDGE ( 'NONE', *, *, #12934, .T. ) ;
#44914 = LINE ( 'NONE', #32818, #31441 ) ;
#44915 =( NAMED_UNIT ( * ) SI_UNIT ( $, .STERADIAN. ) SOLID_ANGLE_UNIT ( ) );
#44916 = DIRECTION ( 'NONE',  ( -0.9473263538541899509, 0.000000000000000000, -0.3202698538628415692 ) ) ;
#44917 = CARTESIAN_POINT ( 'NONE',  ( -330.4913330509368166, -151.3613951634091848, -52.00954392751743427 ) ) ;
#44918 = ADVANCED_FACE ( 'NONE', ( #225 ), #48331, .T. ) ;
#44919 = DIRECTION ( 'NONE',  ( 0.05924062789370748011, 0.000000000000000000, 0.9982437317643217956 ) ) ;
#44920 = PLANE ( 'NONE',  #35506 ) ;
#44921 = ORIENTED_EDGE ( 'NONE', *, *, #51905, .F. ) ;
#44922 = VECTOR ( 'NONE', #1787, 1000.000000000000000 ) ;
#44923 = LINE ( 'NONE', #21009, #22330 ) ;
#44924 = AXIS2_PLACEMENT_3D ( 'NONE', #34921, #11008, #27037 ) ;
#44925 = CIRCLE ( 'NONE', #10513, 125.0000000000000000 ) ;
#44926 = DIRECTION ( 'NONE',  ( 0.7378332790417285736, 0.000000000000000000, -0.6749830015182091136 ) ) ;
#44927 = CARTESIAN_POINT ( 'NONE',  ( 33.25242634436024503, -193.5000000000000000, -94.57776286494160445 ) ) ;
#44928 = ORIENTED_EDGE ( 'NONE', *, *, #48739, .F. ) ;
#44929 = ORIENTED_EDGE ( 'NONE', *, *, #34011, .F. ) ;
#44930 = VERTEX_POINT ( 'NONE', #4443 ) ;
#44931 = AXIS2_PLACEMENT_3D ( 'NONE', #19075, #22510, #38523 ) ;
#44932 = ADVANCED_FACE ( 'NONE', ( #4975 ), #17581, .T. ) ;
#44933 = DIRECTION ( 'NONE',  ( 0.000000000000000000, -0.8229838658936613482, -0.5680647467311485954 ) ) ;
#44934 = DIRECTION ( 'NONE',  ( 0.000000000000000000, 0.000000000000000000, 1.000000000000000000 ) ) ;
#44935 = VECTOR ( 'NONE', #4618, 1000.000000000000000 ) ;
#44936 = CARTESIAN_POINT ( 'NONE',  ( -339.1964088526558498, -95.63860483659122735, -52.00954392751761191 ) ) ;
#44937 = LINE ( 'NONE', #8411, #1873 ) ;
#44938 = VECTOR ( 'NONE', #42922, 1000.000000000000000 ) ;
#44939 = VERTEX_POINT ( 'NONE', #760 ) ;
#44940 = EDGE_CURVE ( 'NONE', #39601, #21117, #29572, .T. ) ;
#44941 = EDGE_CURVE ( 'NONE', #37560, #45837, #13100, .T. ) ;
#44942 = EDGE_CURVE ( 'NONE', #48882, #30259, #33071, .T. ) ;
#44943 = FACE_OUTER_BOUND ( 'NONE', #11840, .T. ) ;
#44944 = ADVANCED_FACE ( 'NONE', ( #41740 ), #45434, .T. ) ;
#44945 = AXIS2_PLACEMENT_3D ( 'NONE', #7590, #43073, #51752 ) ;
#44946 = DIRECTION ( 'NONE',  ( -0.000000000000000000, 1.000000000000000000, -0.000000000000000000 ) ) ;
#44947 = EDGE_LOOP ( 'NONE', ( #15419, #41866, #7106, #9905 ) ) ;
#44948 = EDGE_CURVE ( 'NONE', #36522, #5943, #4700, .T. ) ;
#44949 = CARTESIAN_POINT ( 'NONE',  ( -336.3521761649654422, -123.5000000000000284, 0.000000000000000000 ) ) ;
#44950 = ORIENTED_EDGE ( 'NONE', *, *, #2650, .T. ) ;
#44951 = VECTOR ( 'NONE', #45228, 1000.000000000000114 ) ;
#44952 = CARTESIAN_POINT ( 'NONE',  ( -336.3521761649654422, -86.34605966037949543, -45.90766452162698386 ) ) ;
#44953 = ORIENTED_EDGE ( 'NONE', *, *, #18375, .F. ) ;
#44954 = ADVANCED_FACE ( 'NONE', ( #48861 ), #12836, .T. ) ;
#44955 = ADVANCED_FACE ( 'NONE', ( #49381 ), #40678, .F. ) ;
#44956 = CARTESIAN_POINT ( 'NONE',  ( -48.47912675150885065, -175.3837268820161057, 6.938893903907228378E-15 ) ) ;
#44957 = ADVANCED_FACE ( 'NONE', ( #44909 ), #45692, .T. ) ;
#44958 = EDGE_CURVE ( 'NONE', #30858, #28774, #1269, .T. ) ;
#44959 = CARTESIAN_POINT ( 'NONE',  ( -47.78257572244586271, -177.1207230881787780, 0.7175072570443418174 ) ) ;
#44960 = LINE ( 'NONE', #48648, #31943 ) ;
#44963 = ORIENTED_EDGE ( 'NONE', *, *, #23976, .F. ) ;
#44962 = LINE ( 'NONE', #32851, #19089 ) ;
#44961 = CARTESIAN_POINT ( 'NONE',  ( -330.4913330509368166, -75.22798428563942252, 33.92731199008440512 ) ) ;
#44964 = AXIS2_PLACEMENT_3D ( 'NONE', #4516, #560, #40494 ) ;
#44965 = ADVANCED_FACE ( 'NONE', ( #21254 ), #17828, .T. ) ;
#44966 = DIRECTION ( 'NONE',  ( -0.000000000000000000, 1.000000000000000000, -0.000000000000000000 ) ) ;
#44967 = AXIS2_PLACEMENT_3D ( 'NONE', #16916, #40029, #4053 ) ;
#44968 = ORIENTED_EDGE ( 'NONE', *, *, #46430, .F. ) ;
#44969 = CARTESIAN_POINT ( 'NONE',  ( 41.41233698655026529, -193.5000000000000000, 86.85922373029363541 ) ) ;
#44970 = LINE ( 'NONE', #5288, #28287 ) ;
#44971 = EDGE_LOOP ( 'NONE', ( #44276, #24928, #14045, #22311 ) ) ;
#44972 = VECTOR ( 'NONE', #24234, 1000.000000000000000 ) ;
#44973 = EDGE_CURVE ( 'NONE', #47693, #39559, #25382, .T. ) ;
#44974 = LINE ( 'NONE', #24727, #22515 ) ;
#44976 = LINE ( 'NONE', #16602, #34050 ) ;
#44975 = LINE ( 'NONE', #5550, #19913 ) ;
#44977 = ORIENTED_EDGE ( 'NONE', *, *, #23034, .T. ) ;
#44978 = EDGE_CURVE ( 'NONE', #34020, #5922, #17846, .T. ) ;
#44979 = DIRECTION ( 'NONE',  ( -0.000000000000000000, 1.000000000000000000, -0.000000000000000000 ) ) ;
#44980 = DIRECTION ( 'NONE',  ( 1.043714542225393539E-14, -0.9709418174260527890, -0.2393156642875547968 ) ) ;
#44981 = CARTESIAN_POINT ( 'NONE',  ( -11.17913199888832843, -175.3837268820161057, 119.3051146910914326 ) ) ;
#44982 = VERTEX_POINT ( 'NONE', #44647 ) ;
#44983 = VECTOR ( 'NONE', #40874, 1000.000000000000000 ) ;
#44984 = FACE_OUTER_BOUND ( 'NONE', #40058, .T. ) ;
#44985 = CARTESIAN_POINT ( 'NONE',  ( -339.1964088526558498, -66.33409060400673241, -14.60509510167901404 ) ) ;
#44986 = DIRECTION ( 'NONE',  ( -1.000000000000000000, 9.241633304753606050E-15, 4.850383327711861546E-15 ) ) ;
#44987 = VECTOR ( 'NONE', #34517, 1000.000000000000000 ) ;
#44988 = DIRECTION ( 'NONE',  ( -0.000000000000000000, 1.000000000000000000, -0.000000000000000000 ) ) ;
#44989 = ORIENTED_EDGE ( 'NONE', *, *, #44353, .F. ) ;
#44990 = AXIS2_PLACEMENT_3D ( 'NONE', #49103, #44385, #28062 ) ;
#44991 = LINE ( 'NONE', #1862, #13017 ) ;
#44992 = EDGE_CURVE ( 'NONE', #5970, #37898, #1009, .T. ) ;
#44993 = VECTOR ( 'NONE', #45417, 1000.000000000000114 ) ;
#44994 = LINE ( 'NONE', #41283, #26285 ) ;
#44995 = ORIENTED_EDGE ( 'NONE', *, *, #48018, .T. ) ;
#44996 = CARTESIAN_POINT ( 'NONE',  ( 66.03142248012326831, -183.6283474603465606, 50.12318939044041599 ) ) ;
#44997 = LINE ( 'NONE', #832, #34488 ) ;
#44998 = LINE ( 'NONE', #28418, #12615 ) ;
#44999 = LINE ( 'NONE', #16878, #12149 ) ;
#45000 = DIRECTION ( 'NONE',  ( -0.2635871660690648488, 0.000000000000000000, -0.9646355819083595184 ) ) ;
#45001 = CARTESIAN_POINT ( 'NONE',  ( -339.1964088526558498, -180.9052250602809977, -13.63415328425247885 ) ) ;
#45002 = CIRCLE ( 'NONE', #11396, 60.00000000000000000 ) ;
#45003 = CIRCLE ( 'NONE', #20680, 60.00000000000000000 ) ;
#45004 = PLANE ( 'NONE',  #13567 ) ;
#45005 = CYLINDRICAL_SURFACE ( 'NONE', #14485, 125.0000000000000000 ) ;
#45007 = VERTEX_POINT ( 'NONE', #49632 ) ;
#45006 = PLANE ( 'NONE',  #36227 ) ;
#45008 = AXIS2_PLACEMENT_3D ( 'NONE', #24734, #1069, #28919 ) ;
#45009 = AXIS2_PLACEMENT_3D ( 'NONE', #28616, #16561, #8655 ) ;
#45010 = ORIENTED_EDGE ( 'NONE', *, *, #25886, .F. ) ;
#45011 = EDGE_CURVE ( 'NONE', #25286, #42685, #15325, .T. ) ;
#45012 = EDGE_CURVE ( 'NONE', #7333, #29626, #49117, .T. ) ;
#45013 = CARTESIAN_POINT ( 'NONE',  ( 73.62243227112291777, -193.5000000000000000, 21.61797988633237821 ) ) ;
#45014 = FACE_OUTER_BOUND ( 'NONE', #11999, .T. ) ;
#45015 = EDGE_LOOP ( 'NONE', ( #50264, #35153, #44031, #36218 ) ) ;
#45016 = ORIENTED_EDGE ( 'NONE', *, *, #51709, .F. ) ;
#45017 = VECTOR ( 'NONE', #20621, 999.9999999999998863 ) ;
#45018 = VERTEX_POINT ( 'NONE', #25198 ) ;
#45019 = DIRECTION ( 'NONE',  ( 0.08879589532293853671, 0.000000000000000000, -0.9960498426152166740 ) ) ;
#45020 = CIRCLE ( 'NONE', #24858, 125.0000000000000000 ) ;
#45021 = VECTOR ( 'NONE', #50480, 1000.000000000000000 ) ;
#45023 = AXIS2_PLACEMENT_3D ( 'NONE', #25255, #20794, #49453 ) ;
#45022 = LINE ( 'NONE', #9013, #44607 ) ;
#45024 = DIRECTION ( 'NONE',  ( -0.000000000000000000, 1.000000000000000000, -0.000000000000000000 ) ) ;
#45025 = VERTEX_POINT ( 'NONE', #38042 ) ;
#45026 = VERTEX_POINT ( 'NONE', #2821 ) ;
#45027 = AXIS2_PLACEMENT_3D ( 'NONE', #29846, #21967, #46409 ) ;
#45028 = PLANE ( 'NONE',  #45359 ) ;
#45030 = VERTEX_POINT ( 'NONE', #34110 ) ;
#45029 = DIRECTION ( 'NONE',  ( 0.000000000000000000, 0.000000000000000000, 1.000000000000000000 ) ) ;
#45031 = EDGE_CURVE ( 'NONE', #33001, #37750, #46463, .T. ) ;
#45032 = CYLINDRICAL_SURFACE ( 'NONE', #10485, 10.00000000000000178 ) ;
#45033 = VERTEX_POINT ( 'NONE', #23059 ) ;
#45034 = LINE ( 'NONE', #9025, #27196 ) ;
#45035 = ORIENTED_EDGE ( 'NONE', *, *, #15735, .T. ) ;
#45036 = CARTESIAN_POINT ( 'NONE',  ( -166.1003692892502102, -177.1207230881787780, -42.31126686685032467 ) ) ;
#45037 = CARTESIAN_POINT ( 'NONE',  ( -74.51199343215203896, -177.1207230881787780, -122.2591094863194598 ) ) ;
#45038 = LINE ( 'NONE', #41325, #28234 ) ;
#45039 = EDGE_CURVE ( 'NONE', #3419, #30279, #34370, .T. ) ;
#45040 = EDGE_LOOP ( 'NONE', ( #50916, #358, #44079, #26316 ) ) ;
#45041 = VECTOR ( 'NONE', #16758, 1000.000000000000000 ) ;
#45042 = ORIENTED_EDGE ( 'NONE', *, *, #50955, .T. ) ;
#45043 = DIRECTION ( 'NONE',  ( 1.000000000000000000, 0.000000000000000000, 0.000000000000000000 ) ) ;
#45044 = VECTOR ( 'NONE', #46609, 1000.000000000000000 ) ;
#45045 = CARTESIAN_POINT ( 'NONE',  ( 0.000000000000000000, -162.6242368362071602, -44.16213414209478572 ) ) ;
#45046 = ORIENTED_EDGE ( 'NONE', *, *, #47196, .T. ) ;
#45047 = DIRECTION ( 'NONE',  ( 0.000000000000000000, 0.000000000000000000, 1.000000000000000000 ) ) ;
#45048 = VECTOR ( 'NONE', #13955, 999.9999999999998863 ) ;
#45049 = CARTESIAN_POINT ( 'NONE',  ( -12.76653800058363863, -189.7472609257535510, -119.7898618611245070 ) ) ;
#45050 = ORIENTED_EDGE ( 'NONE', *, *, #48097, .T. ) ;
#45051 = DIRECTION ( 'NONE',  ( 0.000000000000000000, 0.000000000000000000, 1.000000000000000000 ) ) ;
#45052 = CARTESIAN_POINT ( 'NONE',  ( -305.0000000000000568, -123.0000000000002700, -59.99791663049643375 ) ) ;
#45053 = EDGE_LOOP ( 'NONE', ( #2854, #3771, #47813, #43726 ) ) ;
#45054 = DIRECTION ( 'NONE',  ( 0.000000000000000000, -0.4647231720437789981, -0.8854560256532044704 ) ) ;
#45055 = ORIENTED_EDGE ( 'NONE', *, *, #21838, .T. ) ;
#45056 = FACE_BOUND ( 'NONE', #24323, .T. ) ;
#45057 = AXIS2_PLACEMENT_3D ( 'NONE', #13003, #20914, #13536 ) ;
#45058 = DIRECTION ( 'NONE',  ( 0.000000000000000000, 1.000000000000000000, 0.000000000000000000 ) ) ;
#45059 = AXIS2_PLACEMENT_3D ( 'NONE', #28080, #39646, #8643 ) ;
#45060 = CARTESIAN_POINT ( 'NONE',  ( -31.30262293407084329, -183.6283474603465606, -123.8142468240611436 ) ) ;
#45061 = ORIENTED_EDGE ( 'NONE', *, *, #41508, .T. ) ;
#45062 = VECTOR ( 'NONE', #21973, 1000.000000000000000 ) ;
#45063 = AXIS2_PLACEMENT_3D ( 'NONE', #37142, #13247, #36899 ) ;
#45064 = FACE_OUTER_BOUND ( 'NONE', #48778, .T. ) ;
#45065 = CARTESIAN_POINT ( 'NONE',  ( 46.00000000000000711, 20.00000000000000000, -51.00000000000000000 ) ) ;
#45066 = CARTESIAN_POINT ( 'NONE',  ( 62.86098202833237281, -177.1207230881787780, 56.81883646197908178 ) ) ;
#45067 = VECTOR ( 'NONE', #23300, 1000.000000000000000 ) ;
#45068 = DIRECTION ( 'NONE',  ( 0.000000000000000000, 0.000000000000000000, -1.000000000000000000 ) ) ;
#45069 = EDGE_LOOP ( 'NONE', ( #12508, #6322, #4235, #18054 ) ) ;
#45071 = CIRCLE ( 'NONE', #13127, 125.0000000000000000 ) ;
#45070 = CARTESIAN_POINT ( 'NONE',  ( 62.59443091842027940, -177.1207230881787780, -57.33816169485140790 ) ) ;
#45072 = ORIENTED_EDGE ( 'NONE', *, *, #42015, .F. ) ;
#45073 = ORIENTED_EDGE ( 'NONE', *, *, #21466, .T. ) ;
#45074 = LINE ( 'NONE', #23217, #8397 ) ;
#45076 = ORIENTED_EDGE ( 'NONE', *, *, #12364, .F. ) ;
#45075 = CARTESIAN_POINT ( 'NONE',  ( -48.47912675150885065, -177.1207230881787780, 6.938893903907228378E-15 ) ) ;
#45077 = ORIENTED_EDGE ( 'NONE', *, *, #32622, .F. ) ;
#45078 = CARTESIAN_POINT ( 'NONE',  ( 72.68824389704327871, -193.5000000000000000, -26.35287080855459507 ) ) ;
#45079 = ADVANCED_FACE ( 'NONE', ( #50928 ), #35140, .F. ) ;
#45080 = DIRECTION ( 'NONE',  ( 0.000000000000000000, 0.000000000000000000, 1.000000000000000000 ) ) ;
#45081 = DIRECTION ( 'NONE',  ( -0.9785564922995060311, 0.000000000000000000, 0.2059786187410889424 ) ) ;
#45082 = VECTOR ( 'NONE', #19574, 1000.000000000000000 ) ;
#45083 = AXIS2_PLACEMENT_3D ( 'NONE', #48681, #835, #28158 ) ;
#45084 = VERTEX_POINT ( 'NONE', #14156 ) ;
#45085 = CARTESIAN_POINT ( 'NONE',  ( -48.30901192927175458, -189.7472609257535510, -124.9998842437354227 ) ) ;
#45086 = ORIENTED_EDGE ( 'NONE', *, *, #14298, .F. ) ;
#45087 = LINE ( 'NONE', #29803, #32541 ) ;
#45088 = DIRECTION ( 'NONE',  ( 0.000000000000000000, 0.3546048870425463906, 0.9350162426854107256 ) ) ;
#45089 = VECTOR ( 'NONE', #30568, 1000.000000000000000 ) ;
#45090 = LINE ( 'NONE', #37181, #34474 ) ;
#45091 = DIRECTION ( 'NONE',  ( 0.000000000000000000, 0.000000000000000000, -1.000000000000000000 ) ) ;
#45092 = VERTEX_POINT ( 'NONE', #10444 ) ;
#45093 = ORIENTED_EDGE ( 'NONE', *, *, #23689, .T. ) ;
#45094 = ORIENTED_EDGE ( 'NONE', *, *, #30513, .T. ) ;
#45095 = DIRECTION ( 'NONE',  ( -0.2920567706369833760, 0.000000000000000000, 0.9564009842765202052 ) ) ;
#45096 = DIRECTION ( 'NONE',  ( 0.000000000000000000, -0.2393156642875482742, 0.9709418174260544543 ) ) ;
#45097 = VECTOR ( 'NONE', #35060, 999.9999999999998863 ) ;
#45098 = VECTOR ( 'NONE', #11839, 1000.000000000000000 ) ;
#45099 = EDGE_CURVE ( 'NONE', #42685, #46449, #39072, .T. ) ;
#45100 = DIRECTION ( 'NONE',  ( -0.000000000000000000, -0.9927088740980548609, -0.1205366802553164696 ) ) ;
#45101 = AXIS2_PLACEMENT_3D ( 'NONE', #12626, #15824, #35765 ) ;
#45103 = VECTOR ( 'NONE', #42897, 1000.000000000000000 ) ;
#45102 = FACE_BOUND ( 'NONE', #7875, .T. ) ;
#45104 = DIRECTION ( 'NONE',  ( 0.000000000000000000, -1.000000000000000000, 0.000000000000000000 ) ) ;
#45105 = ORIENTED_EDGE ( 'NONE', *, *, #30815, .T. ) ;
#45106 = ORIENTED_EDGE ( 'NONE', *, *, #41954, .T. ) ;
#45108 = EDGE_LOOP ( 'NONE', ( #2381, #29063, #40283, #47858 ) ) ;
#45107 = DIRECTION ( 'NONE',  ( -0.9960498426152177842, 0.000000000000000000, 0.08879589532292482545 ) ) ;
#45109 = VERTEX_POINT ( 'NONE', #50413 ) ;
#45110 = DIRECTION ( 'NONE',  ( -1.000000000000000000, 0.000000000000000000, 0.000000000000000000 ) ) ;
#45111 = CARTESIAN_POINT ( 'NONE',  ( -336.3521761649654422, -136.0347666902908372, 57.67619951860663718 ) ) ;
#45112 = CARTESIAN_POINT ( 'NONE',  ( -165.2002711502080672, -183.6283474603465606, 44.73448837594998651 ) ) ;
#45113 = CARTESIAN_POINT ( 'NONE',  ( -339.1964088526558498, -68.15673923803898049, 20.45418021416614351 ) ) ;
#45114 = DIRECTION ( 'NONE',  ( 0.000000000000000000, -1.000000000000000000, -0.000000000000000000 ) ) ;
#45115 = VERTEX_POINT ( 'NONE', #34869 ) ;
#45116 = LINE ( 'NONE', #5166, #4026 ) ;
#45117 = VERTEX_POINT ( 'NONE', #22278 ) ;
#45118 = ORIENTED_EDGE ( 'NONE', *, *, #43094, .F. ) ;
#45119 = CARTESIAN_POINT ( 'NONE',  ( -336.3521761649654422, -92.15051119686104641, -50.05135858667769355 ) ) ;
#45120 = AXIS2_PLACEMENT_3D ( 'NONE', #26140, #34037, #29314 ) ;
#45121 = AXIS2_PLACEMENT_3D ( 'NONE', #23878, #39894, #49112 ) ;
#45122 = CARTESIAN_POINT ( 'NONE',  ( -339.1964088526558498, -71.02573290043878274, -26.97593913775585506 ) ) ;
#45123 = AXIS2_PLACEMENT_3D ( 'NONE', #36136, #24065, #28505 ) ;
#45124 = EDGE_CURVE ( 'NONE', #1095, #19776, #25965, .T. ) ;
#45125 = CARTESIAN_POINT ( 'NONE',  ( -170.0000000000000284, -113.5000000000000142, -60.00000000000001421 ) ) ;
#45126 = LINE ( 'NONE', #9371, #35569 ) ;
#45127 = DIRECTION ( 'NONE',  ( -0.000000000000000000, 1.000000000000000000, -0.000000000000000000 ) ) ;
#45128 = ORIENTED_EDGE ( 'NONE', *, *, #7699, .F. ) ;
#45129 = PLANE ( 'NONE',  #45681 ) ;
#45130 = DIRECTION ( 'NONE',  ( 0.000000000000000000, -1.091719307548070640E-13, 1.000000000000000000 ) ) ;
#45131 = EDGE_CURVE ( 'NONE', #5355, #20985, #22039, .T. ) ;
#45132 = LINE ( 'NONE', #9121, #7666 ) ;
#45133 = FACE_BOUND ( 'NONE', #47401, .T. ) ;
#45134 = ORIENTED_EDGE ( 'NONE', *, *, #20858, .T. ) ;
#45135 = VECTOR ( 'NONE', #39803, 1000.000000000000000 ) ;
#45136 = AXIS2_PLACEMENT_3D ( 'NONE', #30218, #21565, #9728 ) ;
#45137 = CARTESIAN_POINT ( 'NONE',  ( -336.3521761649654422, -93.31268025388605736, 51.85292399224829296 ) ) ;
#45138 = ORIENTED_EDGE ( 'NONE', *, *, #30325, .F. ) ;
#45139 = AXIS2_PLACEMENT_3D ( 'NONE', #25130, #33262, #41401 ) ;
#45140 = CARTESIAN_POINT ( 'NONE',  ( -171.2727421180348415, -177.1207230881787780, 23.38221600314376047 ) ) ;
#45141 = VERTEX_POINT ( 'NONE', #29902 ) ;
#45142 = DIRECTION ( 'NONE',  ( 0.8858462335218260097, 0.000000000000000000, 0.4639789333096864810 ) ) ;
#45143 = EDGE_CURVE ( 'NONE', #30058, #41128, #5998, .T. ) ;
#45144 = AXIS2_PLACEMENT_3D ( 'NONE', #11855, #17650, #5300 ) ;
#45145 = VERTEX_POINT ( 'NONE', #34616 ) ;
#45146 = EDGE_CURVE ( 'NONE', #2933, #27449, #11931, .T. ) ;
#45147 = AXIS2_PLACEMENT_3D ( 'NONE', #27622, #7897, #23927 ) ;
#45148 = CARTESIAN_POINT ( 'NONE',  ( -125.5794209599708751, -183.6283474603465606, 97.11716833071891131 ) ) ;
#45149 = EDGE_CURVE ( 'NONE', #43478, #40260, #10967, .T. ) ;
#45150 = FACE_BOUND ( 'NONE', #30336, .T. ) ;
#45152 = EDGE_LOOP ( 'NONE', ( #11269, #19402 ) ) ;
#45151 = DIRECTION ( 'NONE',  ( 0.000000000000000000, 0.000000000000000000, -1.000000000000000000 ) ) ;
#45153 = DIRECTION ( 'NONE',  ( 0.000000000000000000, 0.000000000000000000, 1.000000000000000000 ) ) ;
#45154 = ORIENTED_EDGE ( 'NONE', *, *, #41769, .F. ) ;
#45155 = ORIENTED_EDGE ( 'NONE', *, *, #44039, .T. ) ;
#45156 = ORIENTED_EDGE ( 'NONE', *, *, #16489, .T. ) ;
#45157 = CARTESIAN_POINT ( 'NONE',  ( -105.7090724259147976, -175.3837268820161057, 111.1293539894142697 ) ) ;
#45158 = VECTOR ( 'NONE', #39273, 1000.000000000000000 ) ;
#45159 = CARTESIAN_POINT ( 'NONE',  ( 49.03269102277813829, 35.00000000000000000, -50.83217377521822300 ) ) ;
#45160 = AXIS2_PLACEMENT_3D ( 'NONE', #2376, #37847, #42047 ) ;
#45161 = VERTEX_POINT ( 'NONE', #22801 ) ;
#45162 = EDGE_CURVE ( 'NONE', #4141, #48781, #22021, .T. ) ;
#45163 = DIRECTION ( 'NONE',  ( 0.000000000000000000, 0.000000000000000000, 1.000000000000000000 ) ) ;
#45164 = CARTESIAN_POINT ( 'NONE',  ( -135.4258661347518000, -189.7472609257535510, -89.80681772907016125 ) ) ;
#45165 = LINE ( 'NONE', #45939, #2012 ) ;
#45166 = ORIENTED_EDGE ( 'NONE', *, *, #37875, .F. ) ;
#45167 = CIRCLE ( 'NONE', #42629, 125.0000000000000000 ) ;
#45168 = PLANE ( 'NONE',  #1595 ) ;
#45169 = CARTESIAN_POINT ( 'NONE',  ( 0.000000000000000000, -182.0698235717851787, 7.111664135064491354 ) ) ;
#45170 = ORIENTED_EDGE ( 'NONE', *, *, #26937, .F. ) ;
#45173 = ORIENTED_EDGE ( 'NONE', *, *, #41548, .F. ) ;
#45172 = FACE_OUTER_BOUND ( 'NONE', #40938, .T. ) ;
#45171 = CARTESIAN_POINT ( 'NONE',  ( -49.17567778057185990, -193.5000000000000000, 0.7175072570443320474 ) ) ;
#45174 = VECTOR ( 'NONE', #50059, 1000.000000000000000 ) ;
#45175 = VERTEX_POINT ( 'NONE', #38301 ) ;
#45176 = CARTESIAN_POINT ( 'NONE',  ( 57.66105628977221187, -175.3837268820161057, 66.02470404298190942 ) ) ;
#45177 = ORIENTED_EDGE ( 'NONE', *, *, #37206, .F. ) ;
#45178 = CARTESIAN_POINT ( 'NONE',  ( 76.31829002442924548, -177.1207230881787780, 7.113702696402420145 ) ) ;
#45179 = ORIENTED_EDGE ( 'NONE', *, *, #49427, .T. ) ;
#45180 = CARTESIAN_POINT ( 'NONE',  ( -36.15208382588832592, -177.1207230881787780, 123.3865623328509145 ) ) ;
#45181 = CARTESIAN_POINT ( 'NONE',  ( -172.2804936848317823, -177.1207230881787780, -7.024906801078572016 ) ) ;
#45182 = ORIENTED_EDGE ( 'NONE', *, *, #48140, .F. ) ;
#45183 = LINE ( 'NONE', #20991, #22498 ) ;
#45184 = VERTEX_POINT ( 'NONE', #18085 ) ;
#45185 = VECTOR ( 'NONE', #37600, 1000.000000000000000 ) ;
#45186 = VERTEX_POINT ( 'NONE', #3080 ) ;
#45187 = CARTESIAN_POINT ( 'NONE',  ( -305.0000000000000568, -66.84097189748108292, 19.74220186498881091 ) ) ;
#45188 = CARTESIAN_POINT ( 'NONE',  ( -147.6585554144535593, -183.6283474603465606, 76.08180419845380982 ) ) ;
#45189 = DIRECTION ( 'NONE',  ( -0.000000000000000000, 1.000000000000000000, 0.000000000000000000 ) ) ;
#45190 = PLANE ( 'NONE',  #47572 ) ;
#45191 = ORIENTED_EDGE ( 'NONE', *, *, #33007, .T. ) ;
#45192 = CARTESIAN_POINT ( 'NONE',  ( -339.1964088526558498, -123.5000000000000284, 0.000000000000000000 ) ) ;
#45193 = EDGE_CURVE ( 'NONE', #37367, #46084, #50161, .T. ) ;
#45194 = EDGE_CURVE ( 'NONE', #7784, #5668, #26210, .T. ) ;
#45195 = SHAPE_DEFINITION_REPRESENTATION ( #50371, #15324 ) ;
#45196 = DIRECTION ( 'NONE',  ( 0.000000000000000000, 0.000000000000000000, 1.000000000000000000 ) ) ;
#45197 = PLANE ( 'NONE',  #50545 ) ;
#45198 = DIRECTION ( 'NONE',  ( 0.000000000000000000, 0.2393156642875548246, -0.9709418174260527890 ) ) ;
#45199 = DIRECTION ( 'NONE',  ( 0.000000000000000000, 0.000000000000000000, -1.000000000000000000 ) ) ;
#45200 = DIRECTION ( 'NONE',  ( 0.8757349421956379665, 0.000000000000000000, -0.4827922027307427477 ) ) ;
#45201 = VECTOR ( 'NONE', #14014, 1000.000000000000000 ) ;
#45202 = VERTEX_POINT ( 'NONE', #2569 ) ;
#45203 = AXIS2_PLACEMENT_3D ( 'NONE', #40611, #24100, #40110 ) ;
#45204 = VECTOR ( 'NONE', #37836, 1000.000000000000000 ) ;
#45205 = AXIS2_PLACEMENT_3D ( 'NONE', #8418, #15809, #24199 ) ;
#45206 = CARTESIAN_POINT ( 'NONE',  ( -330.4913330509368166, -79.00630452878473875, -38.74998146212148953 ) ) ;
#45207 = CARTESIAN_POINT ( 'NONE',  ( 66.42899531795131907, -177.1207230881787780, 49.20491319441622124 ) ) ;
#45208 = ORIENTED_EDGE ( 'NONE', *, *, #49129, .T. ) ;
#45209 = LINE ( 'NONE', #37293, #36313 ) ;
#45210 = EDGE_CURVE ( 'NONE', #43643, #12625, #6258, .T. ) ;
#45211 = EDGE_LOOP ( 'NONE', ( #50325, #25007, #49602, #4716 ) ) ;
#45212 = EDGE_CURVE ( 'NONE', #23257, #36997, #50663, .T. ) ;
#45213 = FACE_OUTER_BOUND ( 'NONE', #22661, .T. ) ;
#45214 = EDGE_CURVE ( 'NONE', #20956, #12246, #10712, .T. ) ;
#45215 = FACE_OUTER_BOUND ( 'NONE', #35956, .T. ) ;
#45216 = DIRECTION ( 'NONE',  ( 0.000000000000000000, -0.000000000000000000, -1.000000000000000000 ) ) ;
#45217 = DIRECTION ( 'NONE',  ( 0.000000000000000000, 0.000000000000000000, 1.000000000000000000 ) ) ;
#45218 = EDGE_CURVE ( 'NONE', #37576, #43853, #51975, .T. ) ;
#45219 = ORIENTED_EDGE ( 'NONE', *, *, #14086, .T. ) ;
#45220 = DIRECTION ( 'NONE',  ( 0.000000000000000000, 1.794860556477336491E-13, -1.000000000000000000 ) ) ;
#45221 = DIRECTION ( 'NONE',  ( 0.000000000000000000, -0.000000000000000000, 1.000000000000000000 ) ) ;
#45222 = CIRCLE ( 'NONE', #22555, 125.0000000000000000 ) ;
#45223 = DIRECTION ( 'NONE',  ( 0.3202698538628279690, 0.000000000000000000, 0.9473263538541946138 ) ) ;
#45224 = ORIENTED_EDGE ( 'NONE', *, *, #17913, .F. ) ;
#45225 = DIRECTION ( 'NONE',  ( -0.000000000000000000, -1.000000000000000000, 0.000000000000000000 ) ) ;
#45226 = ORIENTED_EDGE ( 'NONE', *, *, #12811, .T. ) ;
#45227 = LINE ( 'NONE', #33388, #1557 ) ;
#45228 = DIRECTION ( 'NONE',  ( 0.1768902751225733261, 0.000000000000000000, -0.9842305779475966077 ) ) ;
#45229 = PRODUCT_DEFINITION_FORMATION_WITH_SPECIFIED_SOURCE ( 'ANY', '', #12961, .NOT_KNOWN. ) ;
#45232 = EDGE_LOOP ( 'NONE', ( #45797, #34728 ) ) ;
#45231 = CARTESIAN_POINT ( 'NONE',  ( -330.4913330509368166, -175.5095439275173419, 27.86139516340933042 ) ) ;
#45230 = LINE ( 'NONE', #37319, #4049 ) ;
#45233 = AXIS2_PLACEMENT_3D ( 'NONE', #8250, #3788, #19814 ) ;
#45234 = AXIS2_PLACEMENT_3D ( 'NONE', #41189, #13081, #33046 ) ;
#45235 = DIRECTION ( 'NONE',  ( 0.000000000000000000, -0.9350162426854146114, 0.3546048870425363986 ) ) ;
#45236 = VERTEX_POINT ( 'NONE', #31450 ) ;
#45237 = LINE ( 'NONE', #21830, #31440 ) ;
#45238 = LINE ( 'NONE', #28911, #26644 ) ;
#45239 = EDGE_LOOP ( 'NONE', ( #38568, #45860, #22942, #33526 ) ) ;
#45240 = CARTESIAN_POINT ( 'NONE',  ( 74.03660210627325000, -189.7472609257535510, -19.12855698118388048 ) ) ;
#45243 = EDGE_LOOP ( 'NONE', ( #26747, #33771, #48720, #45915 ) ) ;
#45242 = CARTESIAN_POINT ( 'NONE',  ( -339.1964088526558498, -130.2355952558260412, 59.62073260661674823 ) ) ;
#45241 = CARTESIAN_POINT ( 'NONE',  ( -330.4913330509368166, -84.75001853787871653, -44.49369547121542467 ) ) ;
#45244 = ORIENTED_EDGE ( 'NONE', *, *, #10672, .F. ) ;
#45245 = EDGE_CURVE ( 'NONE', #117, #41297, #47498, .T. ) ;
#45246 = CIRCLE ( 'NONE', #22579, 125.0000000000000000 ) ;
#45247 = DIRECTION ( 'NONE',  ( -0.1182731709213523247, 0.000000000000000000, -0.9929810960135185827 ) ) ;
#45248 = DIRECTION ( 'NONE',  ( -0.000000000000000000, 1.000000000000000000, -0.000000000000000000 ) ) ;
#45249 = LINE ( 'NONE', #9235, #34884 ) ;
#45250 = ORIENTED_EDGE ( 'NONE', *, *, #34843, .F. ) ;
#45251 = CYLINDRICAL_SURFACE ( 'NONE', #33264, 125.0000000000000000 ) ;
#45252 = CARTESIAN_POINT ( 'NONE',  ( -48.47912675150885065, -175.3837268820161057, 6.938893903907228378E-15 ) ) ;
#45253 = DIRECTION ( 'NONE',  ( 0.000000000000000000, 0.000000000000000000, -1.000000000000000000 ) ) ;
#45254 = DIRECTION ( 'NONE',  ( 0.000000000000000000, 0.000000000000000000, 1.000000000000000000 ) ) ;
#45255 = EDGE_CURVE ( 'NONE', #11111, #36214, #39340, .T. ) ;
#45256 = EDGE_CURVE ( 'NONE', #49289, #11294, #3868, .T. ) ;
#45257 = EDGE_LOOP ( 'NONE', ( #9544, #50225, #33065, #11540 ) ) ;
#45258 = ADVANCED_FACE ( 'NONE', ( #11990 ), #27514, .T. ) ;
#45259 = CARTESIAN_POINT ( 'NONE',  ( -332.3517673607765914, -123.5000000000000284, 0.000000000000000000 ) ) ;
#45260 = DIRECTION ( 'NONE',  ( 0.000000000000000000, -1.850371707708594366E-15, -1.000000000000000000 ) ) ;
#45261 = EDGE_CURVE ( 'NONE', #33448, #7384, #19628, .T. ) ;
#45262 = VECTOR ( 'NONE', #12245, 1000.000000000000000 ) ;
#45263 = LINE ( 'NONE', #20534, #43396 ) ;
#45264 = EDGE_LOOP ( 'NONE', ( #31872, #44805, #37241, #31480 ) ) ;
#45265 = CARTESIAN_POINT ( 'NONE',  ( 0.000000000000000000, -102.5783116644905562, -55.16595831843955722 ) ) ;
#45266 = EDGE_CURVE ( 'NONE', #37774, #25331, #11738, .T. ) ;
#45267 = CARTESIAN_POINT ( 'NONE',  ( -72.72541169915515979, -177.1207230881787780, 121.6072260099955429 ) ) ;
#45268 = DIRECTION ( 'NONE',  ( 0.000000000000000000, -0.4845575045900850641, -0.8747594096352605542 ) ) ;
#45269 = CARTESIAN_POINT ( 'NONE',  ( -163.3872488209693756, -193.5000000000000000, -49.20491319441543254 ) ) ;
#45270 = EDGE_CURVE ( 'NONE', #33816, #36764, #20400, .T. ) ;
#45271 = EDGE_CURVE ( 'NONE', #46508, #23360, #51460, .T. ) ;
#45272 = FACE_OUTER_BOUND ( 'NONE', #17555, .T. ) ;
#45273 = ADVANCED_FACE ( 'NONE', ( #16211 ), #32226, .F. ) ;
#45274 = LINE ( 'NONE', #48683, #34562 ) ;
#45275 = DIRECTION ( 'NONE',  ( -0.4566292373937200777, 0.000000000000000000, 0.8896570909947436601 ) ) ;
#45277 = VERTEX_POINT ( 'NONE', #7292 ) ;
#45276 = CARTESIAN_POINT ( 'NONE',  ( -339.1964088526558498, -71.49045607248255862, -27.86139516340906397 ) ) ;
#45278 = EDGE_CURVE ( 'NONE', #3888, #50437, #39584, .T. ) ;
#45279 = ORIENTED_EDGE ( 'NONE', *, *, #555, .F. ) ;
#45280 = FACE_OUTER_BOUND ( 'NONE', #27965, .T. ) ;
#45281 = EDGE_CURVE ( 'NONE', #2342, #7429, #43550, .T. ) ;
#45282 = EDGE_CURVE ( 'NONE', #32802, #39370, #47764, .T. ) ;
#45283 = DIRECTION ( 'NONE',  ( 0.000000000000000000, 0.000000000000000000, 1.000000000000000000 ) ) ;
#45285 = ORIENTED_EDGE ( 'NONE', *, *, #13814, .T. ) ;
#45284 = CARTESIAN_POINT ( 'NONE',  ( -336.3521761649654422, -82.40546666720629787, 42.41660376256258047 ) ) ;
#45286 = EDGE_LOOP ( 'NONE', ( #27722, #9946, #16826, #11781 ) ) ;
#45287 = ORIENTED_EDGE ( 'NONE', *, *, #14673, .T. ) ;
#45288 = CARTESIAN_POINT ( 'NONE',  ( 45.18203132788821108, 28.00000000000000355, -44.69668003214260210 ) ) ;
#45289 = DIRECTION ( 'NONE',  ( -0.7765238627180437447, 0.000000000000000000, 0.6300878435817094392 ) ) ;
#45290 = PLANE ( 'NONE',  #30831 ) ;
#45291 = ORIENTED_EDGE ( 'NONE', *, *, #1601, .F. ) ;
#45292 = EDGE_CURVE ( 'NONE', #41684, #30672, #43798, .T. ) ;
#45293 = AXIS2_PLACEMENT_3D ( 'NONE', #31129, #47696, #27176 ) ;
#45294 = DIRECTION ( 'NONE',  ( 0.000000000000000000, 1.191176786837407622E-13, 1.000000000000000000 ) ) ;
#45296 = ORIENTED_EDGE ( 'NONE', *, *, #46878, .F. ) ;
#45295 = FACE_OUTER_BOUND ( 'NONE', #42210, .T. ) ;
#45297 = PLANE ( 'NONE',  #42380 ) ;
#45298 = ORIENTED_EDGE ( 'NONE', *, *, #28332, .T. ) ;
#45299 = PLANE ( 'NONE',  #44844 ) ;
#45300 = ORIENTED_EDGE ( 'NONE', *, *, #11281, .T. ) ;
#45301 = FACE_OUTER_BOUND ( 'NONE', #22915, .T. ) ;
#45302 = CARTESIAN_POINT ( 'NONE',  ( -71.40672220061267694, -189.7472609257535510, -122.8793122007208751 ) ) ;
#45303 = DIRECTION ( 'NONE',  ( -0.000000000000000000, 0.000000000000000000, 1.000000000000000000 ) ) ;
#45304 = ORIENTED_EDGE ( 'NONE', *, *, #34825, .F. ) ;
#45305 = ORIENTED_EDGE ( 'NONE', *, *, #42917, .T. ) ;
#45306 = FACE_OUTER_BOUND ( 'NONE', #2502, .T. ) ;
#45308 = VECTOR ( 'NONE', #39029, 1000.000000000000227 ) ;
#45307 = FACE_OUTER_BOUND ( 'NONE', #11919, .T. ) ;
#45309 = ORIENTED_EDGE ( 'NONE', *, *, #35555, .T. ) ;
#45310 = CARTESIAN_POINT ( 'NONE',  ( 76.47090317495664635, -175.3837268820161057, -3.534122433557446374 ) ) ;
#45311 = VECTOR ( 'NONE', #7405, 1000.000000000000114 ) ;
#45312 = EDGE_CURVE ( 'NONE', #22578, #34663, #15181, .T. ) ;
#45313 = EDGE_CURVE ( 'NONE', #1806, #18280, #39840, .T. ) ;
#45314 = EDGE_LOOP ( 'NONE', ( #32343, #7114, #18187, #50942 ) ) ;
#45315 = DIRECTION ( 'NONE',  ( -0.9993203489176063492, 0.000000000000000000, -0.03686245026030392224 ) ) ;
#45316 = CARTESIAN_POINT ( 'NONE',  ( -129.9529520667707914, -193.5000000000000000, -94.79987230211959570 ) ) ;
#45317 = EDGE_CURVE ( 'NONE', #6723, #46797, #49777, .T. ) ;
#45318 = ADVANCED_FACE ( 'NONE', ( #27245 ), #9110, .F. ) ;
#45319 = VERTEX_POINT ( 'NONE', #36420 ) ;
#45320 = PLANE ( 'NONE',  #28225 ) ;
#45321 = ORIENTED_EDGE ( 'NONE', *, *, #286, .F. ) ;
#45322 = DIRECTION ( 'NONE',  ( 1.000000000000000000, 1.050884489711603377E-17, -8.654812430365582767E-17 ) ) ;
#45323 = DIRECTION ( 'NONE',  ( 0.000000000000000000, 1.000000000000000000, -0.000000000000000000 ) ) ;
#45324 = ORIENTED_EDGE ( 'NONE', *, *, #47421, .F. ) ;
#45325 = DIRECTION ( 'NONE',  ( 1.000000000000000000, 0.000000000000000000, 0.000000000000000000 ) ) ;
#45326 = CARTESIAN_POINT ( 'NONE',  ( -106.4764934152196645, -213.5000000000000000, 110.7307791902283043 ) ) ;
#45327 = CARTESIAN_POINT ( 'NONE',  ( -101.5170032742336446, -193.5000000000000000, 112.0852863853383354 ) ) ;
#45328 = CARTESIAN_POINT ( 'NONE',  ( -332.3517673607765914, -172.9832938399466684, -32.17247266903247294 ) ) ;
#45329 = AXIS2_PLACEMENT_3D ( 'NONE', #41962, #6505, #22248 ) ;
#45330 = ORIENTED_EDGE ( 'NONE', *, *, #14759, .T. ) ;
#45331 = CARTESIAN_POINT ( 'NONE',  ( -99.02518858244150124, -189.7472609257535510, 114.3245189510261355 ) ) ;
#45332 = ORIENTED_EDGE ( 'NONE', *, *, #24879, .F. ) ;
#45333 = EDGE_LOOP ( 'NONE', ( #8619, #33291, #46041, #32465 ) ) ;
#45334 = EDGE_CURVE ( 'NONE', #10698, #51182, #29606, .T. ) ;
#45335 = CARTESIAN_POINT ( 'NONE',  ( 68.59638248015004081, -177.1207230881787780, -43.79868877201405297 ) ) ;
#45337 = ORIENTED_EDGE ( 'NONE', *, *, #33380, .T. ) ;
#45336 = CARTESIAN_POINT ( 'NONE',  ( -128.7986236165182561, -175.3837268820161057, 94.47107458416955694 ) ) ;
#45338 = ORIENTED_EDGE ( 'NONE', *, *, #24055, .F. ) ;
#45339 = DIRECTION ( 'NONE',  ( 1.000000000000000000, -0.000000000000000000, -0.000000000000000000 ) ) ;
#45340 = ADVANCED_FACE ( 'NONE', ( #8569 ), #1198, .T. ) ;
#45341 = DIRECTION ( 'NONE',  ( -1.000000000000000000, 0.000000000000000000, -0.000000000000000000 ) ) ;
#45342 = VERTEX_POINT ( 'NONE', #420 ) ;
#45343 = VECTOR ( 'NONE', #29016, 1000.000000000000000 ) ;
#45344 = LINE ( 'NONE', #29545, #424 ) ;
#45345 = ORIENTED_EDGE ( 'NONE', *, *, #49903, .T. ) ;
#45346 = DIRECTION ( 'NONE',  ( 1.000000000000000000, 0.000000000000000000, 0.000000000000000000 ) ) ;
#45347 = DIRECTION ( 'NONE',  ( 0.000000000000000000, -1.000000000000000000, 0.000000000000000000 ) ) ;
#45348 = FACE_OUTER_BOUND ( 'NONE', #14083, .T. ) ;
#45349 = LINE ( 'NONE', #9080, #29931 ) ;
#45350 = EDGE_LOOP ( 'NONE', ( #35010, #25511, #8096, #42884 ) ) ;
#45351 = ORIENTED_EDGE ( 'NONE', *, *, #7569, .T. ) ;
#45352 = VERTEX_POINT ( 'NONE', #948 ) ;
#45353 = CARTESIAN_POINT ( 'NONE',  ( -330.4913330509368166, -90.39567187580871632, -48.84008046109136814 ) ) ;
#45354 = CARTESIAN_POINT ( 'NONE',  ( 71.15591247552653442, -193.5000000000000000, 36.22785377504035154 ) ) ;
#45355 = DIRECTION ( 'NONE',  ( -1.000000000000000000, -0.000000000000000000, -0.000000000000000000 ) ) ;
#45356 = CARTESIAN_POINT ( 'NONE',  ( 48.47907891923915713, -175.3837268820161057, 78.89300572996904748 ) ) ;
#45357 = EDGE_LOOP ( 'NONE', ( #454, #42504 ) ) ;
#45358 = UNCERTAINTY_MEASURE_WITH_UNIT (LENGTH_MEASURE( 1.000000000000000082E-05 ), #4980, 'distance_accuracy_value', 'NONE');
#45359 = AXIS2_PLACEMENT_3D ( 'NONE', #9018, #25053, #41060 ) ;
#45360 = AXIS2_PLACEMENT_3D ( 'NONE', #26627, #14289, #46353 ) ;
#45361 = ORIENTED_EDGE ( 'NONE', *, *, #5775, .F. ) ;
#45363 = VERTEX_POINT ( 'NONE', #13305 ) ;
#45362 = CARTESIAN_POINT ( 'NONE',  ( -336.3521761649654422, -66.84438072661991725, -16.67542351306652648 ) ) ;
#45364 = CYLINDRICAL_SURFACE ( 'NONE', #23813, 125.0000000000000000 ) ;
#45365 = ORIENTED_EDGE ( 'NONE', *, *, #18476, .F. ) ;
#45366 = CARTESIAN_POINT ( 'NONE',  ( -71.40672220061269115, -189.7472609257535510, -122.8793122007208751 ) ) ;
#45367 = DIRECTION ( 'NONE',  ( 0.000000000000000000, 0.000000000000000000, 1.000000000000000000 ) ) ;
#45368 = DIRECTION ( 'NONE',  ( 1.000000000000000000, 0.000000000000000000, 0.000000000000000000 ) ) ;
#45369 = CARTESIAN_POINT ( 'NONE',  ( -169.1033029113419559, -193.5000000000000000, 32.78426643622745473 ) ) ;
#45370 = ADVANCED_FACE ( 'NONE', ( #49048 ), #45376, .F. ) ;
#45371 = DIRECTION ( 'NONE',  ( -0.4827922027307427477, 0.000000000000000000, -0.8757349421956379665 ) ) ;
#45372 = ORIENTED_EDGE ( 'NONE', *, *, #42570, .T. ) ;
#45373 = DIRECTION ( 'NONE',  ( -0.8858462335218260097, -0.000000000000000000, 0.4639789333096864810 ) ) ;
#45374 = ORIENTED_EDGE ( 'NONE', *, *, #42439, .T. ) ;
#45375 = ORIENTED_EDGE ( 'NONE', *, *, #42813, .F. ) ;
#45376 = PLANE ( 'NONE',  #26226 ) ;
#45377 = CIRCLE ( 'NONE', #15992, 60.00000000000000000 ) ;
#45378 = CARTESIAN_POINT ( 'NONE',  ( -330.4913330509368166, -64.86990808808705822, 6.615309698014281814 ) ) ;
#45379 = ORIENTED_EDGE ( 'NONE', *, *, #11188, .F. ) ;
#45380 = DIRECTION ( 'NONE',  ( -0.000000000000000000, 0.8229838658936575735, 0.5680647467311540355 ) ) ;
#45381 = PLANE ( 'NONE',  #12916 ) ;
#45382 = FACE_OUTER_BOUND ( 'NONE', #23529, .T. ) ;
#45383 = DIRECTION ( 'NONE',  ( -0.9842305779475967187, 0.000000000000000000, -0.1768902751225733538 ) ) ;
#45384 = PLANE ( 'NONE',  #23204 ) ;
#45385 = FACE_OUTER_BOUND ( 'NONE', #26518, .T. ) ;
#45386 = CYLINDRICAL_SURFACE ( 'NONE', #9785, 125.0000000000000000 ) ;
#45387 = ORIENTED_EDGE ( 'NONE', *, *, #12054, .T. ) ;
#45388 = EDGE_CURVE ( 'NONE', #42659, #3183, #43861, .T. ) ;
#45389 = CARTESIAN_POINT ( 'NONE',  ( -106.4764934152197497, -213.5000000000000000, -110.7307791902282759 ) ) ;
#45390 = EDGE_LOOP ( 'NONE', ( #3614, #45946, #28458, #18308 ) ) ;
#45391 = PLANE ( 'NONE',  #50499 ) ;
#45392 = ORIENTED_EDGE ( 'NONE', *, *, #43041, .F. ) ;
#45393 = CARTESIAN_POINT ( 'NONE',  ( -11.17913199888832487, -189.7472609257535510, 119.3051146910914468 ) ) ;
#45394 = ORIENTED_EDGE ( 'NONE', *, *, #42456, .T. ) ;
#45395 = VECTOR ( 'NONE', #23, 1000.000000000000000 ) ;
#45396 = EDGE_CURVE ( 'NONE', #6991, #8561, #24868, .T. ) ;
#45397 = VECTOR ( 'NONE', #7873, 1000.000000000000000 ) ;
#45398 = LINE ( 'NONE', #2005, #36888 ) ;
#45399 = DIRECTION ( 'NONE',  ( 0.000000000000000000, 0.000000000000000000, 1.000000000000000000 ) ) ;
#45401 = ORIENTED_EDGE ( 'NONE', *, *, #36343, .T. ) ;
#45400 = CARTESIAN_POINT ( 'NONE',  ( -330.4913330509368166, -64.99044476834247064, -7.608018572113060429 ) ) ;
#45402 = ADVANCED_FACE ( 'NONE', ( #37472 ), #21187, .F. ) ;
#45403 = FACE_OUTER_BOUND ( 'NONE', #37392, .T. ) ;
#45404 = ORIENTED_EDGE ( 'NONE', *, *, #36090, .T. ) ;
#45405 = ORIENTED_EDGE ( 'NONE', *, *, #19267, .F. ) ;
#45406 = ORIENTED_EDGE ( 'NONE', *, *, #6311, .F. ) ;
#45407 = CARTESIAN_POINT ( 'NONE',  ( -47.64924157374594671, -189.7472609257535510, 124.9972451320097377 ) ) ;
#45408 = DIRECTION ( 'NONE',  ( 0.9993203489176063492, 0.000000000000000000, 0.03686245026030503941 ) ) ;
#45409 = AXIS2_PLACEMENT_3D ( 'NONE', #1443, #17496, #13530 ) ;
#45410 = ORIENTED_EDGE ( 'NONE', *, *, #49773, .F. ) ;
#45411 = DIRECTION ( 'NONE',  ( -0.000000000000000000, 1.000000000000000000, -0.000000000000000000 ) ) ;
#45412 = DIRECTION ( 'NONE',  ( 0.000000000000000000, -1.000000000000000000, 0.000000000000000000 ) ) ;
#45413 = DIRECTION ( 'NONE',  ( -1.000000000000000000, 0.000000000000000000, 0.000000000000000000 ) ) ;
#45414 = VERTEX_POINT ( 'NONE', #21445 ) ;
#45415 = EDGE_CURVE ( 'NONE', #23609, #31967, #18703, .T. ) ;
#45416 = DIRECTION ( 'NONE',  ( -0.000000000000000000, 1.000000000000000000, -0.000000000000000000 ) ) ;
#45417 = DIRECTION ( 'NONE',  ( -0.000000000000000000, -0.7485107481710953081, 0.6631226582408016323 ) ) ;
#45418 = ORIENTED_EDGE ( 'NONE', *, *, #4777, .T. ) ;
#45420 = VERTEX_POINT ( 'NONE', #36958 ) ;
#45419 = CARTESIAN_POINT ( 'NONE',  ( -40.30502441601360886, -193.5000000000000000, 123.7303097900624920 ) ) ;
#45421 = ORIENTED_EDGE ( 'NONE', *, *, #45845, .T. ) ;
#45422 = ORIENTED_EDGE ( 'NONE', *, *, #31605, .F. ) ;
#45423 = CARTESIAN_POINT ( 'NONE',  ( -332.3517673607765914, -182.3871109312487420, -4.498567634386014369 ) ) ;
#45424 = AXIS2_PLACEMENT_3D ( 'NONE', #50745, #27062, #2900 ) ;
#45425 = EDGE_LOOP ( 'NONE', ( #18354, #9794, #25389, #45418 ) ) ;
#45426 = DIRECTION ( 'NONE',  ( 0.000000000000000000, 0.000000000000000000, -1.000000000000000000 ) ) ;
#45427 = ADVANCED_FACE ( 'NONE', ( #32753 ), #1476, .T. ) ;
#45428 = CARTESIAN_POINT ( 'NONE',  ( 73.32083127613157103, -183.6283474603465606, 28.10285082451656535 ) ) ;
#45429 = ORIENTED_EDGE ( 'NONE', *, *, #18289, .F. ) ;
#45430 = LINE ( 'NONE', #37784, #3163 ) ;
#45431 = EDGE_LOOP ( 'NONE', ( #46214, #13713, #31751, #36590 ) ) ;
#45432 = AXIS2_PLACEMENT_3D ( 'NONE', #27528, #10983, #27007 ) ;
#45433 = EDGE_LOOP ( 'NONE', ( #43791, #11201, #2456, #30588 ) ) ;
#45434 = PLANE ( 'NONE',  #35453 ) ;
#45435 = EDGE_CURVE ( 'NONE', #41297, #35501, #32940, .T. ) ;
#45436 = FACE_OUTER_BOUND ( 'NONE', #43759, .T. ) ;
#45437 = DIRECTION ( 'NONE',  ( 0.000000000000000000, 0.000000000000000000, 1.000000000000000000 ) ) ;
#45438 = DIRECTION ( 'NONE',  ( 0.000000000000000000, -1.000000000000000000, 0.000000000000000000 ) ) ;
#45439 = ORIENTED_EDGE ( 'NONE', *, *, #41857, .T. ) ;
#45440 = PLANE ( 'NONE',  #19805 ) ;
#45441 = LINE ( 'NONE', #768, #18841 ) ;
#45442 = ADVANCED_FACE ( 'NONE', ( #8830 ), #41410, .T. ) ;
#45443 = APPLICATION_PROTOCOL_DEFINITION ( 'draft international standard', 'automotive_design', 1998, #35726 ) ;
#45444 = PLANE ( 'NONE',  #22983 ) ;
#45445 = CARTESIAN_POINT ( 'NONE',  ( -332.3517673607765914, -81.08339623743702873, -41.09453333279329712 ) ) ;
#45446 = FACE_OUTER_BOUND ( 'NONE', #42475, .T. ) ;
#45447 = DIRECTION ( 'NONE',  ( 0.000000000000000000, 0.000000000000000000, 1.000000000000000000 ) ) ;
#45448 = CARTESIAN_POINT ( 'NONE',  ( -336.3521761649654422, -72.48138011061176655, -29.74944317415788930 ) ) ;
#45449 = ORIENTED_EDGE ( 'NONE', *, *, #10965, .T. ) ;
#45450 = VECTOR ( 'NONE', #30015, 1000.000000000000227 ) ;
#45451 = EDGE_CURVE ( 'NONE', #13962, #6134, #33539, .T. ) ;
#45452 = DIRECTION ( 'NONE',  ( 0.000000000000000000, 1.000000000000000000, -0.000000000000000000 ) ) ;
#45453 = FACE_OUTER_BOUND ( 'NONE', #38373, .T. ) ;
#45454 = ORIENTED_EDGE ( 'NONE', *, *, #47561, .F. ) ;
#45455 = DIRECTION ( 'NONE',  ( 0.9785564922995046988, 0.000000000000000000, -0.2059786187410953262 ) ) ;
#45456 = ORIENTED_EDGE ( 'NONE', *, *, #29055, .F. ) ;
#45457 = PLANE ( 'NONE',  #18399 ) ;
#45458 = CARTESIAN_POINT ( 'NONE',  ( -23.99795575808071035, -193.5000000000000000, -122.5792489240757703 ) ) ;
#45459 = DIRECTION ( 'NONE',  ( -0.000000000000000000, 1.000000000000000000, -0.000000000000000000 ) ) ;
#45460 = DIRECTION ( 'NONE',  ( 0.9785564922995046988, 0.000000000000000000, -0.2059786187410953262 ) ) ;
#45461 = AXIS2_PLACEMENT_3D ( 'NONE', #20611, #45583, #20347 ) ;
#45462 = DIRECTION ( 'NONE',  ( 0.000000000000000000, -1.000000000000000000, 0.000000000000000000 ) ) ;
#45463 = VECTOR ( 'NONE', #15130, 999.9999999999998863 ) ;
#45464 = CARTESIAN_POINT ( 'NONE',  ( -140.0851925571752474, -189.7472609257535510, 83.57229767764225414 ) ) ;
#45465 = EDGE_LOOP ( 'NONE', ( #2673, #44671, #21405, #30561 ) ) ;
#45466 = VECTOR ( 'NONE', #27848, 1000.000000000000000 ) ;
#45467 = CARTESIAN_POINT ( 'NONE',  ( -365.0000000000001137, -168.5000000000000284, 0.000000000000000000 ) ) ;
#45468 = ORIENTED_EDGE ( 'NONE', *, *, #39598, .T. ) ;
#45469 = CARTESIAN_POINT ( 'NONE',  ( -118.4510020108455137, -175.3837268820161057, 103.5805805771131674 ) ) ;
#45470 = ORIENTED_EDGE ( 'NONE', *, *, #13002, .T. ) ;
#45471 = CARTESIAN_POINT ( 'NONE',  ( -11.80936624585915418, -193.5000000000000000, -119.5003291395395735 ) ) ;
#45472 = EDGE_CURVE ( 'NONE', #30320, #1001, #29325, .T. ) ;
#45473 = ORIENTED_EDGE ( 'NONE', *, *, #48234, .T. ) ;
#45474 = EDGE_CURVE ( 'NONE', #6061, #13689, #49576, .T. ) ;
#45475 = AXIS2_PLACEMENT_3D ( 'NONE', #41111, #28490, #40313 ) ;
#45476 = FACE_OUTER_BOUND ( 'NONE', #39662, .T. ) ;
#45477 = DIRECTION ( 'NONE',  ( 0.000000000000000000, 0.000000000000000000, -1.000000000000000000 ) ) ;
#45478 = VERTEX_POINT ( 'NONE', #9618 ) ;
#45481 = ORIENTED_EDGE ( 'NONE', *, *, #8650, .F. ) ;
#45480 = LINE ( 'NONE', #37594, #24981 ) ;
#45479 = DIRECTION ( 'NONE',  ( -0.000000000000000000, 1.000000000000000000, -0.000000000000000000 ) ) ;
#45482 = VECTOR ( 'NONE', #9924, 1000.000000000000000 ) ;
#45483 = DIRECTION ( 'NONE',  ( 0.000000000000000000, 0.000000000000000000, 1.000000000000000000 ) ) ;
#45484 = ORIENTED_EDGE ( 'NONE', *, *, #12095, .F. ) ;
#45485 = DIRECTION ( 'NONE',  ( 0.000000000000000000, 1.156482317317871232E-16, 1.000000000000000000 ) ) ;
#45486 = VERTEX_POINT ( 'NONE', #25636 ) ;
#45487 = ADVANCED_FACE ( 'NONE', ( #37208 ), #5426, .T. ) ;
#45488 = CARTESIAN_POINT ( 'NONE',  ( -339.1964088526558498, -68.51134412508183402, -21.38919645685240312 ) ) ;
#45491 = VERTEX_POINT ( 'NONE', #14600 ) ;
#45490 = DIRECTION ( 'NONE',  ( -0.000000000000000000, 1.000000000000000000, -0.000000000000000000 ) ) ;
#45489 = LINE ( 'NONE', #32861, #7317 ) ;
#45492 = EDGE_LOOP ( 'NONE', ( #4963, #2558, #43187, #37616 ) ) ;
#45493 = EDGE_CURVE ( 'NONE', #42501, #39634, #8644, .T. ) ;
#45494 = DIRECTION ( 'NONE',  ( -0.000000000000000000, -0.1205366802553130001, 0.9927088740980551940 ) ) ;
#45495 = DIRECTION ( 'NONE',  ( 0.000000000000000000, -1.000000000000000000, 0.000000000000000000 ) ) ;
#45496 = EDGE_CURVE ( 'NONE', #1315, #18280, #26928, .T. ) ;
#45497 = DIRECTION ( 'NONE',  ( 0.9473263538541923934, 0.000000000000000000, -0.3202698538628350744 ) ) ;
#45498 = ORIENTED_EDGE ( 'NONE', *, *, #40718, .F. ) ;
#45499 = CARTESIAN_POINT ( 'NONE',  ( -172.2424017797220870, -183.6283474603465606, 7.666780576875855679 ) ) ;
#45500 =( NAMED_UNIT ( * ) SI_UNIT ( $, .STERADIAN. ) SOLID_ANGLE_UNIT ( ) );
#45501 = DIRECTION ( 'NONE',  ( 0.000000000000000000, 0.000000000000000000, -1.000000000000000000 ) ) ;
#45502 = AXIS2_PLACEMENT_3D ( 'NONE', #22341, #7095, #34176 ) ;
#45503 = DIRECTION ( 'NONE',  ( 1.000000000000000000, -0.000000000000000000, -0.000000000000000000 ) ) ;
#45504 = ORIENTED_EDGE ( 'NONE', *, *, #39173, .T. ) ;
#45505 = VECTOR ( 'NONE', #50295, 999.9999999999998863 ) ;
#45506 = DIRECTION ( 'NONE',  ( -0.9646355819083576311, 0.000000000000000000, -0.2635871660690715101 ) ) ;
#45507 = FACE_OUTER_BOUND ( 'NONE', #38052, .T. ) ;
#45508 = VECTOR ( 'NONE', #16884, 1000.000000000000114 ) ;
#45509 = CARTESIAN_POINT ( 'NONE',  ( -29.73468717939733708, -177.1207230881787780, 123.5865930638410930 ) ) ;
#45510 = ORIENTED_EDGE ( 'NONE', *, *, #11556, .F. ) ;
#45511 = CARTESIAN_POINT ( 'NONE',  ( -49.38192458147459973, -189.7472609257535510, 0.4300652022765185656 ) ) ;
#45512 = CYLINDRICAL_SURFACE ( 'NONE', #26087, 125.0000000000000000 ) ;
#45513 = PLANE ( 'NONE',  #30262 ) ;
#45514 = PLANE ( 'NONE',  #14052 ) ;
#45515 = VECTOR ( 'NONE', #34265, 1000.000000000000000 ) ;
#45516 = CARTESIAN_POINT ( 'NONE',  ( 70.98542830588607444, -177.1207230881787780, -36.78613984829961936 ) ) ;
#45517 = VECTOR ( 'NONE', #38050, 1000.000000000000000 ) ;
#45518 = AXIS2_PLACEMENT_3D ( 'NONE', #11135, #48708, #20059 ) ;
#45519 = PLANE ( 'NONE',  #11899 ) ;
#45520 = DIRECTION ( 'NONE',  ( -0.000000000000000000, 1.000000000000000000, -0.000000000000000000 ) ) ;
#45522 = ORIENTED_EDGE ( 'NONE', *, *, #48210, .T. ) ;
#45521 = DIRECTION ( 'NONE',  ( 0.000000000000000000, -0.000000000000000000, 1.000000000000000000 ) ) ;
#45523 = ORIENTED_EDGE ( 'NONE', *, *, #42350, .F. ) ;
#45524 = DIRECTION ( 'NONE',  ( -0.000000000000000000, 1.000000000000000000, -0.000000000000000000 ) ) ;
#45525 = DIRECTION ( 'NONE',  ( -0.6749830015182091136, 0.000000000000000000, -0.7378332790417285736 ) ) ;
#45527 = EDGE_LOOP ( 'NONE', ( #21367, #41516, #4071, #50998 ) ) ;
#45526 = CARTESIAN_POINT ( 'NONE',  ( -34.51936650669028239, -193.5000000000000000, -124.2180546213278092 ) ) ;
#45528 = EDGE_LOOP ( 'NONE', ( #26835, #32152, #31673, #17873 ) ) ;
#45529 = ORIENTED_EDGE ( 'NONE', *, *, #30401, .F. ) ;
#45530 = CARTESIAN_POINT ( 'NONE',  ( -173.3294908491238004, -193.5000000000000000, -6.114457023560960991 ) ) ;
#45531 = ADVANCED_FACE ( 'NONE', ( #46932 ), #25905, .T. ) ;
#45532 = ADVANCED_FACE ( 'NONE', ( #46660 ), #38239, .F. ) ;
#45533 = EDGE_CURVE ( 'NONE', #32182, #16051, #30884, .T. ) ;
#45534 = LINE ( 'NONE', #9525, #8509 ) ;
#45535 = DIRECTION ( 'NONE',  ( 0.000000000000000000, 1.989149585786738886E-13, -1.000000000000000000 ) ) ;
#45536 = ORIENTED_EDGE ( 'NONE', *, *, #18191, .T. ) ;
#45537 = ADVANCED_FACE ( 'NONE', ( #45890 ), #10912, .T. ) ;
#45538 = CIRCLE ( 'NONE', #18707, 125.0000000000000568 ) ;
#45539 = LINE ( 'NONE', #48446, #24374 ) ;
#45541 = ORIENTED_EDGE ( 'NONE', *, *, #31579, .T. ) ;
#45540 = CARTESIAN_POINT ( 'NONE',  ( -336.3521761649654422, -133.3383340306578759, -59.18789727217212970 ) ) ;
#45542 = EDGE_CURVE ( 'NONE', #9916, #27018, #23719, .T. ) ;
#45543 = ADVANCED_FACE ( 'NONE', ( #10134 ), #38511, .F. ) ;
#45544 = CARTESIAN_POINT ( 'NONE',  ( -48.82732838694323618, -183.6283474603465606, -0.9374196611341184537 ) ) ;
#45545 = VERTEX_POINT ( 'NONE', #46154 ) ;
#45546 = LINE ( 'NONE', #17943, #40617 ) ;
#45547 = ORIENTED_EDGE ( 'NONE', *, *, #4403, .T. ) ;
#45548 = CARTESIAN_POINT ( 'NONE',  ( 65.38692482895589819, -183.6283474603465606, -51.57055649762702387 ) ) ;
#45549 = EDGE_CURVE ( 'NONE', #45874, #24651, #2508, .T. ) ;
#45550 = LINE ( 'NONE', #44768, #285 ) ;
#45551 = PLANE ( 'NONE',  #34945 ) ;
#45552 = AXIS2_PLACEMENT_3D ( 'NONE', #29935, #1034, #45217 ) ;
#45553 = CIRCLE ( 'NONE', #25401, 125.0000000000000000 ) ;
#45554 = ADVANCED_FACE ( 'NONE', ( #34049 ), #34308, .F. ) ;
#45555 = ORIENTED_EDGE ( 'NONE', *, *, #39764, .F. ) ;
#45556 = VECTOR ( 'NONE', #11488, 1000.000000000000114 ) ;
#45557 = ORIENTED_EDGE ( 'NONE', *, *, #34960, .T. ) ;
#45558 = VECTOR ( 'NONE', #17717, 1000.000000000000114 ) ;
#45559 = FACE_OUTER_BOUND ( 'NONE', #10348, .T. ) ;
#45560 = ADVANCED_FACE ( 'NONE', ( #22217 ), #37733, .T. ) ;
#45561 = CARTESIAN_POINT ( 'NONE',  ( 46.00000000000000711, 33.00000000000000000, -46.00000000000000000 ) ) ;
#45562 = ORIENTED_EDGE ( 'NONE', *, *, #42983, .F. ) ;
#45563 = CARTESIAN_POINT ( 'NONE',  ( -170.0502155641509319, -177.1207230881787780, -29.07697310430877735 ) ) ;
#45564 = EDGE_CURVE ( 'NONE', #49548, #51496, #18538, .T. ) ;
#45565 = EDGE_LOOP ( 'NONE', ( #31271, #18810, #46910, #51588 ) ) ;
#45566 = CARTESIAN_POINT ( 'NONE',  ( 61.06976976088562026, -193.5000000000000000, -60.19999396110170409 ) ) ;
#45567 = VECTOR ( 'NONE', #23348, 1000.000000000000114 ) ;
#45568 = CYLINDRICAL_SURFACE ( 'NONE', #443, 4.000000000000003553 ) ;
#45569 = VERTEX_POINT ( 'NONE', #34551 ) ;
#45570 = CARTESIAN_POINT ( 'NONE',  ( -109.0835867659423712, -183.6283474603465606, -109.3256576763155294 ) ) ;
#45571 = ORIENTED_EDGE ( 'NONE', *, *, #40051, .F. ) ;
#45572 = DIRECTION ( 'NONE',  ( 0.000000000000000000, -1.000000000000000000, 0.000000000000000000 ) ) ;
#45573 = CARTESIAN_POINT ( 'NONE',  ( -47.60339180931321579, -177.1207230881787780, -0.4827922027307358088 ) ) ;
#45574 = ORIENTED_EDGE ( 'NONE', *, *, #31088, .T. ) ;
#45575 = VECTOR ( 'NONE', #30354, 1000.000000000000114 ) ;
#45576 = DIRECTION ( 'NONE',  ( 0.000000000000000000, 0.000000000000000000, 1.000000000000000000 ) ) ;
#45577 = CARTESIAN_POINT ( 'NONE',  ( 76.52053249983504202, -193.5000000000000000, -0.2918682030015403162 ) ) ;
#45578 = CARTESIAN_POINT ( 'NONE',  ( -147.6585554144535024, -193.5000000000000000, 76.08180419845385245 ) ) ;
#45579 = DIRECTION ( 'NONE',  ( -0.000000000000000000, -1.000000000000000000, 0.000000000000000000 ) ) ;
#45580 = ADVANCED_FACE ( 'NONE', ( #50603 ), #10654, .T. ) ;
#45581 = AXIS2_PLACEMENT_3D ( 'NONE', #10614, #26643, #50564 ) ;
#45582 = ORIENTED_EDGE ( 'NONE', *, *, #29862, .T. ) ;
#45583 = DIRECTION ( 'NONE',  ( 0.000000000000000000, -1.000000000000000000, 0.000000000000000000 ) ) ;
#45584 = ORIENTED_EDGE ( 'NONE', *, *, #37871, .T. ) ;
#45585 = ORIENTED_EDGE ( 'NONE', *, *, #42175, .T. ) ;
#45586 = DIRECTION ( 'NONE',  ( 0.000000000000000000, -0.5680647467311596976, -0.8229838658936536877 ) ) ;
#45588 = EDGE_LOOP ( 'NONE', ( #20296, #34164, #17010, #48855 ) ) ;
#45587 = CARTESIAN_POINT ( 'NONE',  ( -305.0000000000000568, -137.3729703655834840, 58.37414404713479854 ) ) ;
#45589 = ORIENTED_EDGE ( 'NONE', *, *, #35540, .T. ) ;
#45590 = DIRECTION ( 'NONE',  ( -0.000000000000000000, 1.000000000000000000, -0.000000000000000000 ) ) ;
#45591 = AXIS2_PLACEMENT_3D ( 'NONE', #18679, #11031, #51511 ) ;
#45592 = AXIS2_PLACEMENT_3D ( 'NONE', #3368, #31217, #26766 ) ;
#45593 = EDGE_CURVE ( 'NONE', #30158, #32832, #17769, .T. ) ;
#45594 = DIRECTION ( 'NONE',  ( 0.000000000000000000, 0.000000000000000000, 1.000000000000000000 ) ) ;
#45595 = AXIS2_PLACEMENT_3D ( 'NONE', #28422, #5317, #576 ) ;
#45596 = ORIENTED_EDGE ( 'NONE', *, *, #49139, .T. ) ;
#45597 = CARTESIAN_POINT ( 'NONE',  ( -22.44626007086656116, -177.1207230881787780, 122.2591094863196872 ) ) ;
#45598 = EDGE_LOOP ( 'NONE', ( #4330, #37362, #39922, #18955 ) ) ;
#45599 = CARTESIAN_POINT ( 'NONE',  ( 0.000000000000000000, 101.5275612430648380, -100.5543802447186579 ) ) ;
#45600 = CARTESIAN_POINT ( 'NONE',  ( -91.81555821786915317, -193.5000000000000000, 116.1806952091180563 ) ) ;
#45601 = EDGE_CURVE ( 'NONE', #39890, #42685, #22738, .T. ) ;
#45602 = EDGE_CURVE ( 'NONE', #9008, #36633, #105, .T. ) ;
#45603 = EDGE_CURVE ( 'NONE', #172, #19493, #230, .T. ) ;
#45604 = AXIS2_PLACEMENT_3D ( 'NONE', #967, #36974, #10670 ) ;
#45605 = CARTESIAN_POINT ( 'NONE',  ( -161.2555905272864436, -175.3837268820161057, -53.91167979418489864 ) ) ;
#45606 = CARTESIAN_POINT ( 'NONE',  ( 5.015379008610445943, -183.6283474603465606, -112.9749434763326690 ) ) ;
#45607 = ORIENTED_EDGE ( 'NONE', *, *, #25451, .F. ) ;
#45608 = ORIENTED_EDGE ( 'NONE', *, *, #15707, .F. ) ;
#45609 = EDGE_CURVE ( 'NONE', #7466, #4324, #6959, .T. ) ;
#45610 = ORIENTED_EDGE ( 'NONE', *, *, #23402, .F. ) ;
#45611 = DIRECTION ( 'NONE',  ( 0.000000000000000000, -0.6631226582407885317, 0.7485107481711069655 ) ) ;
#45612 = LINE ( 'NONE', #17751, #12552 ) ;
#45613 = DIRECTION ( 'NONE',  ( 0.000000000000000000, -0.7485107481711069655, -0.6631226582407885317 ) ) ;
#45614 = PLANE ( 'NONE',  #25537 ) ;
#45615 = VECTOR ( 'NONE', #41817, 1000.000000000000000 ) ;
#45616 = ORIENTED_EDGE ( 'NONE', *, *, #17663, .T. ) ;
#45617 = ADVANCED_FACE ( 'NONE', ( #51908 ), #36112, .T. ) ;
#45618 = AXIS2_PLACEMENT_3D ( 'NONE', #20043, #44222, #47909 ) ;
#45619 = ORIENTED_EDGE ( 'NONE', *, *, #24780, .F. ) ;
#45621 = ORIENTED_EDGE ( 'NONE', *, *, #47791, .F. ) ;
#45620 = CARTESIAN_POINT ( 'NONE',  ( -49.08592689732745384, -193.5000000000000000, 0.7948544414133550395 ) ) ;
#45622 = ORIENTED_EDGE ( 'NONE', *, *, #39764, .T. ) ;
#45623 = ADVANCED_FACE ( 'NONE', ( #3017 ), #28219, .T. ) ;
#45624 = PLANE ( 'NONE',  #16568 ) ;
#45625 = LINE ( 'NONE', #30094, #4007 ) ;
#45626 = ADVANCED_FACE ( 'NONE', ( #23269 ), #19817, .T. ) ;
#45627 = CARTESIAN_POINT ( 'NONE',  ( -330.4913330509368166, -123.5000000000000284, 0.000000000000000000 ) ) ;
#45628 = CARTESIAN_POINT ( 'NONE',  ( -170.0000000000000284, -93.50000000000001421, -51.54700538379269403 ) ) ;
#45629 = EDGE_LOOP ( 'NONE', ( #27153, #39105, #46539, #9869 ) ) ;
#45630 = CARTESIAN_POINT ( 'NONE',  ( -166.6807411098556031, -193.5000000000000000, 37.47770156625504967 ) ) ;
#45631 = VECTOR ( 'NONE', #31567, 1000.000000000000000 ) ;
#45632 = ORIENTED_EDGE ( 'NONE', *, *, #18120, .F. ) ;
#45633 = EDGE_CURVE ( 'NONE', #46727, #9644, #15128, .T. ) ;
#45634 = EDGE_LOOP ( 'NONE', ( #49385, #21796, #35814, #33463 ) ) ;
#45635 = CARTESIAN_POINT ( 'NONE',  ( -336.3521761649654422, -72.01665693856799066, -28.86398714850468039 ) ) ;
#45636 = AXIS2_PLACEMENT_3D ( 'NONE', #37531, #17313, #45426 ) ;
#45637 = FACE_OUTER_BOUND ( 'NONE', #4035, .T. ) ;
#45638 = VERTEX_POINT ( 'NONE', #12184 ) ;
#45639 = LINE ( 'NONE', #17773, #34860 ) ;
#45640 = FACE_OUTER_BOUND ( 'NONE', #18202, .T. ) ;
#45641 = PLANE ( 'NONE',  #1913 ) ;
#45642 = CARTESIAN_POINT ( 'NONE',  ( -339.1964088526558498, -182.1300919119129560, -6.615309698014600670 ) ) ;
#45643 = EDGE_CURVE ( 'NONE', #37290, #51892, #3645, .T. ) ;
#45644 = PLANE ( 'NONE',  #35349 ) ;
#45645 = FACE_BOUND ( 'NONE', #38853, .T. ) ;
#45646 = EDGE_LOOP ( 'NONE', ( #22152, #197, #7164, #16375 ) ) ;
#45647 = DIRECTION ( 'NONE',  ( 0.000000000000000000, 0.000000000000000000, 1.000000000000000000 ) ) ;
#45648 = VERTEX_POINT ( 'NONE', #51142 ) ;
#45649 = AXIS2_PLACEMENT_3D ( 'NONE', #46227, #14418, #18859 ) ;
#45650 = EDGE_LOOP ( 'NONE', ( #47096, #90, #2339, #12593 ) ) ;
#45651 = PLANE ( 'NONE',  #14573 ) ;
#45652 = VERTEX_POINT ( 'NONE', #27706 ) ;
#45653 = CIRCLE ( 'NONE', #31336, 125.0000000000000000 ) ;
#45654 = CARTESIAN_POINT ( 'NONE',  ( -129.5578577291868214, -175.3837268820161057, 93.82025162278054609 ) ) ;
#45655 = CARTESIAN_POINT ( 'NONE',  ( -48.36085358058748795, -175.3837268820161057, 0.9929810960135245779 ) ) ;
#45657 = ORIENTED_EDGE ( 'NONE', *, *, #9895, .T. ) ;
#45656 = CARTESIAN_POINT ( 'NONE',  ( -104.8182102393454045, -189.7472609257535510, 111.5836353223472770 ) ) ;
#45658 = EDGE_CURVE ( 'NONE', #24439, #31941, #47427, .T. ) ;
#45659 = EDGE_CURVE ( 'NONE', #18186, #33549, #51490, .T. ) ;
#45661 = VECTOR ( 'NONE', #13862, 1000.000000000000227 ) ;
#45660 = CARTESIAN_POINT ( 'NONE',  ( -160.2705093830644216, -193.5000000000000000, -55.92572546981520532 ) ) ;
#45662 = ORIENTED_EDGE ( 'NONE', *, *, #32495, .T. ) ;
#45663 = ORIENTED_EDGE ( 'NONE', *, *, #37824, .F. ) ;
#45664 = ORIENTED_EDGE ( 'NONE', *, *, #34397, .F. ) ;
#45665 = DIRECTION ( 'NONE',  ( 0.000000000000000000, -0.000000000000000000, -1.000000000000000000 ) ) ;
#45666 = CARTESIAN_POINT ( 'NONE',  ( -99.02518858244150124, -189.7472609257535510, 114.3245189510261355 ) ) ;
#45667 = ORIENTED_EDGE ( 'NONE', *, *, #44319, .F. ) ;
#45668 = DIRECTION ( 'NONE',  ( -0.000000000000000000, 1.000000000000000000, -0.000000000000000000 ) ) ;
#45669 = PLANE ( 'NONE',  #29701 ) ;
#45670 = ORIENTED_EDGE ( 'NONE', *, *, #15929, .T. ) ;
#45671 = DIRECTION ( 'NONE',  ( 0.000000000000000000, 0.5680647467311658039, 0.8229838658936494689 ) ) ;
#45672 = DIRECTION ( 'NONE',  ( -0.000000000000000000, -1.000000000000000000, 0.000000000000000000 ) ) ;
#45673 = EDGE_LOOP ( 'NONE', ( #22468, #15619, #12428, #49855 ) ) ;
#45675 = ORIENTED_EDGE ( 'NONE', *, *, #41136, .T. ) ;
#45674 = CARTESIAN_POINT ( 'NONE',  ( -75.48985759771373694, -183.6283474603465606, -122.0467960216648606 ) ) ;
#45676 = ORIENTED_EDGE ( 'NONE', *, *, #13790, .F. ) ;
#45677 = ADVANCED_FACE ( 'NONE', ( #31134 ), #47948, .F. ) ;
#45678 = ORIENTED_EDGE ( 'NONE', *, *, #35291, .F. ) ;
#45679 = DIRECTION ( 'NONE',  ( -1.000000000000000000, 0.000000000000000000, 0.000000000000000000 ) ) ;
#45680 = CARTESIAN_POINT ( 'NONE',  ( 0.000000000000000000, -109.3803758070334737, 57.28556722813694080 ) ) ;
#45681 = AXIS2_PLACEMENT_3D ( 'NONE', #21194, #45383, #49324 ) ;
#45682 = ORIENTED_EDGE ( 'NONE', *, *, #26231, .T. ) ;
#45683 = AXIS2_PLACEMENT_3D ( 'NONE', #36482, #48069, #482 ) ;
#45684 = DIRECTION ( 'NONE',  ( -0.000000000000000000, 1.000000000000000000, -0.000000000000000000 ) ) ;
#45685 = CARTESIAN_POINT ( 'NONE',  ( -30.00000000000000000, 0.000000000000000000, 30.00000000000000355 ) ) ;
#45686 = ORIENTED_EDGE ( 'NONE', *, *, #20192, .F. ) ;
#45687 = CARTESIAN_POINT ( 'NONE',  ( -48.47912675150885065, -117.5479369270332057, 6.938893903907228378E-15 ) ) ;
#45688 = ORIENTED_EDGE ( 'NONE', *, *, #21600, .F. ) ;
#45689 = CIRCLE ( 'NONE', #49851, 4.999999999999997335 ) ;
#45690 = EDGE_CURVE ( 'NONE', #43387, #16147, #33023, .T. ) ;
#45691 = ORIENTED_EDGE ( 'NONE', *, *, #18248, .T. ) ;
#45692 = CYLINDRICAL_SURFACE ( 'NONE', #26190, 125.0000000000000000 ) ;
#45693 = CARTESIAN_POINT ( 'NONE',  ( 74.48795740376235130, -177.1207230881787780, -15.97798378892165871 ) ) ;
#45694 = CARTESIAN_POINT ( 'NONE',  ( -336.3521761649653854, -63.52220716707010695, -1.632288850093980725 ) ) ;
#45695 = FILL_AREA_STYLE_COLOUR ( '', #38279 ) ;
#45696 = ORIENTED_EDGE ( 'NONE', *, *, #45261, .T. ) ;
#45697 = LINE ( 'NONE', #41992, #35746 ) ;
#45698 = CARTESIAN_POINT ( 'NONE',  ( 41.00573479224730988, -183.6283474603465606, -87.27805883780176543 ) ) ;
#45699 = CONTEXT_DEPENDENT_SHAPE_REPRESENTATION ( #31349, #6741 ) ;
#45700 = CARTESIAN_POINT ( 'NONE',  ( -180.0000000000000568, -115.7896721143442278, -60.00000000000000711 ) ) ;
#45701 = DIRECTION ( 'NONE',  ( -0.9473263538541946138, 0.000000000000000000, 0.3202698538628279690 ) ) ;
#45702 = ORIENTED_EDGE ( 'NONE', *, *, #48310, .T. ) ;
#45703 = AXIS2_PLACEMENT_3D ( 'NONE', #39323, #24329, #11721 ) ;
#45704 = PLANE ( 'NONE',  #16259 ) ;
#45705 = DIRECTION ( 'NONE',  ( -0.000000000000000000, -0.2393156642875615969, -0.9709418174260511236 ) ) ;
#45706 = LINE ( 'NONE', #18365, #40826 ) ;
#45707 = EDGE_LOOP ( 'NONE', ( #34615, #37418, #26938, #14195 ) ) ;
#45708 = EDGE_LOOP ( 'NONE', ( #8669, #23161, #33475, #13642 ) ) ;
#45709 = DIRECTION ( 'NONE',  ( 0.000000000000000000, 0.000000000000000000, 1.000000000000000000 ) ) ;
#45710 = CARTESIAN_POINT ( 'NONE',  ( 75.27070168362158142, -193.5000000000000000, 17.63462396184792524 ) ) ;
#45711 = ORIENTED_EDGE ( 'NONE', *, *, #10772, .T. ) ;
#45712 = CARTESIAN_POINT ( 'NONE',  ( -170.6250538923603131, -175.3837268820161057, 26.55884942729649723 ) ) ;
#45713 = VERTEX_POINT ( 'NONE', #47700 ) ;
#45714 = LINE ( 'NONE', #21544, #1630 ) ;
#45715 = CARTESIAN_POINT ( 'NONE',  ( -332.3517673607765914, -181.1761995186066088, -12.53476669029101842 ) ) ;
#45716 = CARTESIAN_POINT ( 'NONE',  ( -107.6930423737362190, -183.6283474603465606, 110.0850225811110761 ) ) ;
#45717 = CIRCLE ( 'NONE', #51595, 125.0000000000000000 ) ;
#45718 = AXIS2_PLACEMENT_3D ( 'NONE', #8903, #5242, #41473 ) ;
#45719 = PLANE ( 'NONE',  #16573 ) ;
#45720 = EDGE_CURVE ( 'NONE', #29784, #18925, #7494, .T. ) ;
#45721 = CARTESIAN_POINT ( 'NONE',  ( 57.12946453413545100, -189.7472609257535510, 66.87170886601998632 ) ) ;
#45722 = EDGE_LOOP ( 'NONE', ( #19610, #34325, #39486, #29969 ) ) ;
#45723 = AXIS2_PLACEMENT_3D ( 'NONE', #48218, #32437, #4321 ) ;
#45724 = DIRECTION ( 'NONE',  ( -0.7948544414133523750, 0.000000000000000000, -0.6068001458185945385 ) ) ;
#45725 = ORIENTED_EDGE ( 'NONE', *, *, #14675, .T. ) ;
#45726 = LINE ( 'NONE', #9718, #35923 ) ;
#45727 = ORIENTED_EDGE ( 'NONE', *, *, #44152, .T. ) ;
#45728 = CYLINDRICAL_SURFACE ( 'NONE', #15000, 4.000000000000003553 ) ;
#45729 = ORIENTED_EDGE ( 'NONE', *, *, #42614, .F. ) ;
#45730 = CIRCLE ( 'NONE', #390, 125.0000000000000000 ) ;
#45731 = CARTESIAN_POINT ( 'NONE',  ( -330.4913330509368166, -123.5000000000000284, 0.000000000000000000 ) ) ;
#45732 = CARTESIAN_POINT ( 'NONE',  ( -336.3521761649654422, -165.9166037625627439, 41.09453333279358134 ) ) ;
#45733 = ORIENTED_EDGE ( 'NONE', *, *, #35816, .F. ) ;
#45736 = EDGE_LOOP ( 'NONE', ( #6832, #1389, #43107, #10922 ) ) ;
#45735 = PLANE ( 'NONE',  #21407 ) ;
#45734 = PLANE ( 'NONE',  #19951 ) ;
#45737 = EDGE_CURVE ( 'NONE', #33164, #45018, #3792, .T. ) ;
#45738 = FACE_OUTER_BOUND ( 'NONE', #4102, .T. ) ;
#45739 = VERTEX_POINT ( 'NONE', #32168 ) ;
#45740 = DIRECTION ( 'NONE',  ( -1.000000000000000000, 0.000000000000000000, 0.000000000000000000 ) ) ;
#45741 = EDGE_LOOP ( 'NONE', ( #46982, #19297, #22144, #9675 ) ) ;
#45742 = DIRECTION ( 'NONE',  ( -0.000000000000000000, 1.000000000000000000, -0.000000000000000000 ) ) ;
#45745 = ORIENTED_EDGE ( 'NONE', *, *, #10889, .T. ) ;
#45744 = DIRECTION ( 'NONE',  ( 1.000000000000000000, 0.000000000000000000, 0.000000000000000000 ) ) ;
#45743 = CARTESIAN_POINT ( 'NONE',  ( -180.0000000000000568, -115.7896721143442278, -18.45401972188387418 ) ) ;
#45746 = EDGE_LOOP ( 'NONE', ( #30127, #50395, #299, #38012 ) ) ;
#45747 = PLANE ( 'NONE',  #40788 ) ;
#45748 = DIRECTION ( 'NONE',  ( 1.000000000000000000, 0.000000000000000000, 0.000000000000000000 ) ) ;
#45749 = AXIS2_PLACEMENT_3D ( 'NONE', #21255, #36481, #50163 ) ;
#45750 = CARTESIAN_POINT ( 'NONE',  ( -330.4913330509368166, -123.5000000000000284, 0.000000000000000000 ) ) ;
#45751 = VERTEX_POINT ( 'NONE', #3533 ) ;
#45752 = DIRECTION ( 'NONE',  ( -1.000000000000000000, 0.000000000000000000, 0.000000000000000000 ) ) ;
#45753 = DIRECTION ( 'NONE',  ( -1.000000000000000000, -0.000000000000000000, 0.000000000000000000 ) ) ;
#45754 = DIRECTION ( 'NONE',  ( 0.000000000000000000, -0.000000000000000000, -1.000000000000000000 ) ) ;
#45755 = AXIS2_PLACEMENT_3D ( 'NONE', #13359, #751, #25443 ) ;
#45756 = PLANE ( 'NONE',  #30772 ) ;
#45757 = VECTOR ( 'NONE', #23572, 999.9999999999998863 ) ;
#45758 = ORIENTED_EDGE ( 'NONE', *, *, #41069, .F. ) ;
#45759 = SHAPE_REPRESENTATION_RELATIONSHIP ( 'NONE' , 'NONE' ,  #15639, #15504 ) ;
#45760 = LINE ( 'NONE', #29983, #5323 ) ;
#45762 = VECTOR ( 'NONE', #33864, 1000.000000000000000 ) ;
#45761 = LINE ( 'NONE', #20808, #30641 ) ;
#45763 = LINE ( 'NONE', #46040, #1077 ) ;
#45764 = ORIENTED_EDGE ( 'NONE', *, *, #24072, .F. ) ;
#45765 = DIRECTION ( 'NONE',  ( -0.000000000000000000, -0.9709418174260534551, -0.2393156642875516327 ) ) ;
#45766 = PLANE ( 'NONE',  #51277 ) ;
#45767 = VECTOR ( 'NONE', #6743, 1000.000000000000114 ) ;
#45768 = CARTESIAN_POINT ( 'NONE',  ( -49.40581635894069024, -193.5000000000000000, 0.3758275821142362250 ) ) ;
#45769 = EDGE_CURVE ( 'NONE', #45837, #3041, #47295, .T. ) ;
#45770 = VECTOR ( 'NONE', #38088, 1000.000000000000000 ) ;
#45771 = DIRECTION ( 'NONE',  ( 0.000000000000000000, -0.5680647467311457088, 0.8229838658936634577 ) ) ;
#45772 = ADVANCED_FACE ( 'NONE', ( #15635 ), #7995, .F. ) ;
#45773 = VECTOR ( 'NONE', #20709, 999.9999999999998863 ) ;
#45774 = CARTESIAN_POINT ( 'NONE',  ( -48.47912675150885065, -193.5000000000000000, 1.000000000000006883 ) ) ;
#45775 = FACE_OUTER_BOUND ( 'NONE', #41384, .T. ) ;
#45777 = EDGE_LOOP ( 'NONE', ( #37321, #28057, #47332, #6239 ) ) ;
#45776 = CARTESIAN_POINT ( 'NONE',  ( 37.99238433767461487, -193.5000000000000000, -90.26448786734027863 ) ) ;
#45778 = ORIENTED_EDGE ( 'NONE', *, *, #12756, .T. ) ;
#45779 = DIRECTION ( 'NONE',  ( -0.4031234292879792847, 0.000000000000000000, 0.9151456172430153524 ) ) ;
#45780 = EDGE_CURVE ( 'NONE', #8838, #29027, #37080, .T. ) ;
#45781 = EDGE_CURVE ( 'NONE', #37883, #37128, #45760, .T. ) ;
#45782 = DIRECTION ( 'NONE',  ( -1.000000000000000000, -0.000000000000000000, 0.000000000000000000 ) ) ;
#45784 = ORIENTED_EDGE ( 'NONE', *, *, #2103, .F. ) ;
#45783 = PLANE ( 'NONE',  #51372 ) ;
#45785 = ORIENTED_EDGE ( 'NONE', *, *, #41082, .F. ) ;
#45786 = EDGE_CURVE ( 'NONE', #27512, #26450, #13439, .T. ) ;
#45787 = AXIS2_PLACEMENT_3D ( 'NONE', #20274, #48671, #31851 ) ;
#45788 = EDGE_LOOP ( 'NONE', ( #13399, #4884, #7956, #10984 ) ) ;
#45789 = DIRECTION ( 'NONE',  ( 1.000000000000000000, -0.000000000000000000, -0.000000000000000000 ) ) ;
#45790 = AXIS2_PLACEMENT_3D ( 'NONE', #32154, #28718, #40808 ) ;
#45791 = AXIS2_PLACEMENT_3D ( 'NONE', #47373, #6663, #6909 ) ;
#45792 = DIRECTION ( 'NONE',  ( 1.000000000000000000, 0.000000000000000000, -0.000000000000000000 ) ) ;
#45793 = DIRECTION ( 'NONE',  ( -0.000000000000000000, 1.000000000000000000, 0.000000000000000000 ) ) ;
#45794 = VERTEX_POINT ( 'NONE', #4314 ) ;
#45795 = DIRECTION ( 'NONE',  ( 0.000000000000000000, -0.5680647467311625842, -0.8229838658936516893 ) ) ;
#45797 = ORIENTED_EDGE ( 'NONE', *, *, #41010, .F. ) ;
#45796 = CARTESIAN_POINT ( 'NONE',  ( -48.47912675150885065, -175.3837268820161057, 6.938893903907228378E-15 ) ) ;
#45798 = AXIS2_PLACEMENT_3D ( 'NONE', #24092, #40099, #404 ) ;
#45799 = ADVANCED_FACE ( 'NONE', ( #24291 ), #22098, .T. ) ;
#45800 = AXIS2_PLACEMENT_3D ( 'NONE', #25643, #29844, #25911 ) ;
#45801 = LINE ( 'NONE', #26073, #38170 ) ;
#45802 = EDGE_LOOP ( 'NONE', ( #30582, #95, #26924, #1054 ) ) ;
#45803 = DIRECTION ( 'NONE',  ( 0.6749830015182142207, 0.000000000000000000, -0.7378332790417239107 ) ) ;
#45804 = ORIENTED_EDGE ( 'NONE', *, *, #21503, .T. ) ;
#45805 = CARTESIAN_POINT ( 'NONE',  ( -98.10897907742936752, -189.7472609257535510, 114.7252272087849292 ) ) ;
#45806 = AXIS2_PLACEMENT_3D ( 'NONE', #16861, #33412, #33128 ) ;
#45807 = DIRECTION ( 'NONE',  ( -1.000000000000000000, 0.000000000000000000, 0.000000000000000000 ) ) ;
#45808 = DIRECTION ( 'NONE',  ( 0.000000000000000000, -1.000000000000000000, -0.000000000000000000 ) ) ;
#45809 = VECTOR ( 'NONE', #15883, 1000.000000000000000 ) ;
#45810 = ORIENTED_EDGE ( 'NONE', *, *, #39738, .T. ) ;
#45811 = ORIENTED_EDGE ( 'NONE', *, *, #22709, .F. ) ;
#45812 = DIRECTION ( 'NONE',  ( 0.000000000000000000, 0.000000000000000000, 1.000000000000000000 ) ) ;
#45813 = CARTESIAN_POINT ( 'NONE',  ( -339.1964088526558498, -79.00630452878473875, -38.74998146212148953 ) ) ;
#45814 = ORIENTED_EDGE ( 'NONE', *, *, #2816, .T. ) ;
#45815 = LINE ( 'NONE', #17708, #13983 ) ;
#45816 = ORIENTED_EDGE ( 'NONE', *, *, #24239, .T. ) ;
#45817 = CARTESIAN_POINT ( 'NONE',  ( -170.0000000000000284, -123.5000000000000284, 0.000000000000000000 ) ) ;
#45818 = DIRECTION ( 'NONE',  ( -1.000000000000000000, 0.000000000000000000, 0.000000000000000000 ) ) ;
#45819 = ORIENTED_EDGE ( 'NONE', *, *, #23915, .T. ) ;
#45820 = DIRECTION ( 'NONE',  ( 0.000000000000000000, 0.000000000000000000, -1.000000000000000000 ) ) ;
#45821 = EDGE_LOOP ( 'NONE', ( #26350, #25565, #9066, #44614 ) ) ;
#45822 = AXIS2_PLACEMENT_3D ( 'NONE', #49392, #41480, #26222 ) ;
#45823 = CARTESIAN_POINT ( 'NONE',  ( -47.49008656418669005, -175.3837268820161057, -0.1476465640024710591 ) ) ;
#45824 = CARTESIAN_POINT ( 'NONE',  ( -305.0000000000000568, -157.9941932480467415, -49.09328500076569668 ) ) ;
#45825 = DIRECTION ( 'NONE',  ( -0.000000000000000000, 1.000000000000000000, -0.000000000000000000 ) ) ;
#45826 = ORIENTED_EDGE ( 'NONE', *, *, #13979, .T. ) ;
#45827 = VECTOR ( 'NONE', #22614, 1000.000000000000000 ) ;
#45828 = AXIS2_PLACEMENT_3D ( 'NONE', #47320, #22876, #38896 ) ;
#45829 = CARTESIAN_POINT ( 'NONE',  ( 42.45000882818163035, -193.5000000000000000, -84.30834960112932208 ) ) ;
#45830 = EDGE_CURVE ( 'NONE', #45025, #42517, #39676, .T. ) ;
#45831 = DIRECTION ( 'NONE',  ( -1.000000000000000000, 0.000000000000000000, 0.000000000000000000 ) ) ;
#45832 = LINE ( 'NONE', #22169, #45907 ) ;
#45833 = EDGE_CURVE ( 'NONE', #15690, #15571, #2115, .T. ) ;
#45834 = CARTESIAN_POINT ( 'NONE',  ( -144.0067397530739584, -177.1207230881787780, -80.61932246194587037 ) ) ;
#45835 = ORIENTED_EDGE ( 'NONE', *, *, #46315, .T. ) ;
#45836 = DIRECTION ( 'NONE',  ( -0.7175072570443395970, 0.000000000000000000, 0.6965510290629882695 ) ) ;
#45837 = VERTEX_POINT ( 'NONE', #33915 ) ;
#45838 = VECTOR ( 'NONE', #38226, 1000.000000000000000 ) ;
#45839 = DIRECTION ( 'NONE',  ( -0.000000000000000000, -1.000000000000000000, -0.000000000000000000 ) ) ;
#45841 = ORIENTED_EDGE ( 'NONE', *, *, #46629, .F. ) ;
#45840 = CARTESIAN_POINT ( 'NONE',  ( 46.00000000000000711, 20.00000000000000000, 51.00000000000000000 ) ) ;
#45842 = EDGE_CURVE ( 'NONE', #33208, #3383, #50234, .T. ) ;
#45843 = AXIS2_PLACEMENT_3D ( 'NONE', #12707, #36903, #25577 ) ;
#45844 = VERTEX_POINT ( 'NONE', #29203 ) ;
#45845 = EDGE_CURVE ( 'NONE', #34872, #37919, #21592, .T. ) ;
#45846 = VECTOR ( 'NONE', #38269, 1000.000000000000114 ) ;
#45847 = EDGE_CURVE ( 'NONE', #29842, #4246, #26039, .T. ) ;
#45848 = AXIS2_PLACEMENT_3D ( 'NONE', #6451, #6952, #47685 ) ;
#45849 = DIRECTION ( 'NONE',  ( -0.000000000000000000, 1.000000000000000000, -0.000000000000000000 ) ) ;
#45850 = ORIENTED_EDGE ( 'NONE', *, *, #22494, .F. ) ;
#45851 = EDGE_CURVE ( 'NONE', #4167, #44745, #29647, .T. ) ;
#45852 = FACE_OUTER_BOUND ( 'NONE', #9663, .T. ) ;
#45853 = ORIENTED_EDGE ( 'NONE', *, *, #39909, .T. ) ;
#45854 = PLANE ( 'NONE',  #9900 ) ;
#45855 = CARTESIAN_POINT ( 'NONE',  ( -339.1964088526558498, -90.39567187580880159, -48.84008046109142498 ) ) ;
#45856 = EDGE_CURVE ( 'NONE', #26482, #3778, #37190, .T. ) ;
#45857 = CARTESIAN_POINT ( 'NONE',  ( -213.8817838414232426, -213.5000000000000000, 10.00000000000002842 ) ) ;
#45858 = DIRECTION ( 'NONE',  ( -0.7575112421616191360, 0.000000000000000000, -0.6528221181905227155 ) ) ;
#45859 = ORIENTED_EDGE ( 'NONE', *, *, #16517, .T. ) ;
#45860 = ORIENTED_EDGE ( 'NONE', *, *, #44097, .F. ) ;
#45861 = ORIENTED_EDGE ( 'NONE', *, *, #28134, .T. ) ;
#45862 = LINE ( 'NONE', #25880, #27434 ) ;
#45863 = CARTESIAN_POINT ( 'NONE',  ( -170.0000000000000284, -93.50000000000002842, 51.54700538379266561 ) ) ;
#45864 = AXIS2_PLACEMENT_3D ( 'NONE', #17778, #33792, #22505 ) ;
#45865 = VECTOR ( 'NONE', #31453, 1000.000000000000000 ) ;
#45866 = DIRECTION ( 'NONE',  ( 0.000000000000000000, 0.000000000000000000, -1.000000000000000000 ) ) ;
#45867 = LINE ( 'NONE', #25883, #23071 ) ;
#45868 = ORIENTED_EDGE ( 'NONE', *, *, #6632, .T. ) ;
#45869 = AXIS2_PLACEMENT_3D ( 'NONE', #14139, #26974, #2554 ) ;
#45870 = VERTEX_POINT ( 'NONE', #5567 ) ;
#45872 = ORIENTED_EDGE ( 'NONE', *, *, #2699, .T. ) ;
#45871 = DIRECTION ( 'NONE',  ( -0.000000000000000000, -1.000000000000000000, 0.000000000000000000 ) ) ;
#45873 = ADVANCED_FACE ( 'NONE', ( #49462 ), #25267, .T. ) ;
#45874 = VERTEX_POINT ( 'NONE', #5305 ) ;
#45875 = VECTOR ( 'NONE', #19313, 1000.000000000000114 ) ;
#45876 = CARTESIAN_POINT ( 'NONE',  ( -48.07600332222087758, -193.5000000000000000, -0.9151456172430111335 ) ) ;
#45877 = VECTOR ( 'NONE', #4873, 1000.000000000000000 ) ;
#45878 = CARTESIAN_POINT ( 'NONE',  ( -330.4913330509368166, -116.7644047441726656, 59.62073260661660612 ) ) ;
#45879 = AXIS2_PLACEMENT_3D ( 'NONE', #9694, #50177, #34388 ) ;
#45880 = CIRCLE ( 'NONE', #50911, 60.00000000000000000 ) ;
#45881 = FACE_OUTER_BOUND ( 'NONE', #33258, .T. ) ;
#45882 = CARTESIAN_POINT ( 'NONE',  ( -339.1964088526558498, -96.52406086224361559, 52.47426709956096147 ) ) ;
#45883 = VERTEX_POINT ( 'NONE', #1618 ) ;
#45884 = CARTESIAN_POINT ( 'NONE',  ( -47.57632892154311577, -177.1207230881787780, 0.4300652022765314997 ) ) ;
#45885 = VECTOR ( 'NONE', #36930, 999.9999999999998863 ) ;
#45886 = ORIENTED_EDGE ( 'NONE', *, *, #30512, .T. ) ;
#45887 = AXIS2_PLACEMENT_3D ( 'NONE', #10570, #3211, #3451 ) ;
#45888 = EDGE_CURVE ( 'NONE', #28628, #50885, #21322, .T. ) ;
#45889 = EDGE_LOOP ( 'NONE', ( #30704, #25622, #24786, #16205 ) ) ;
#45890 = FACE_OUTER_BOUND ( 'NONE', #36185, .T. ) ;
#45891 = AXIS2_PLACEMENT_3D ( 'NONE', #23864, #7074, #19408 ) ;
#45892 = DIRECTION ( 'NONE',  ( 0.9473263538541946138, 0.000000000000000000, -0.3202698538628279690 ) ) ;
#45893 = ORIENTED_EDGE ( 'NONE', *, *, #24947, .F. ) ;
#45894 = EDGE_CURVE ( 'NONE', #840, #3228, #1078, .T. ) ;
#45895 = EDGE_CURVE ( 'NONE', #15769, #40690, #25784, .T. ) ;
#45896 = CARTESIAN_POINT ( 'NONE',  ( -111.3295483157475445, -193.5000000000000000, 108.0501018472332504 ) ) ;
#45897 = EDGE_CURVE ( 'NONE', #24889, #46461, #21850, .T. ) ;
#45898 = FACE_OUTER_BOUND ( 'NONE', #11944, .T. ) ;
#45899 = CARTESIAN_POINT ( 'NONE',  ( -56.71246971489870958, -189.7472609257535510, -124.7285535218267540 ) ) ;
#45900 = EDGE_CURVE ( 'NONE', #38948, #42748, #33854, .T. ) ;
#45901 = CARTESIAN_POINT ( 'NONE',  ( 76.46082103836693022, -193.5000000000000000, 3.874202661595785191 ) ) ;
#45902 = ADVANCED_FACE ( 'NONE', ( #42063 ), #38111, .F. ) ;
#45903 = CARTESIAN_POINT ( 'NONE',  ( -305.0000000000000568, -183.3224719910990643, -4.612141029301910500 ) ) ;
#45904 = FACE_BOUND ( 'NONE', #8249, .T. ) ;
#45905 = EDGE_LOOP ( 'NONE', ( #14979, #1719, #37246, #32064 ) ) ;
#45906 = CIRCLE ( 'NONE', #49277, 125.0000000000000000 ) ;
#45907 = VECTOR ( 'NONE', #42130, 1000.000000000000000 ) ;
#45908 = EDGE_CURVE ( 'NONE', #39220, #43850, #40549, .T. ) ;
#45909 = LINE ( 'NONE', #17269, #33173 ) ;
#45910 = ORIENTED_EDGE ( 'NONE', *, *, #4419, .F. ) ;
#45911 = VECTOR ( 'NONE', #16109, 1000.000000000000114 ) ;
#45912 = EDGE_LOOP ( 'NONE', ( #26325, #15784, #30572, #50791 ) ) ;
#45913 = CARTESIAN_POINT ( 'NONE',  ( -330.4913330509368166, -123.5000000000000284, 0.000000000000000000 ) ) ;
#45914 = EDGE_CURVE ( 'NONE', #40260, #41906, #50486, .T. ) ;
#45915 = ORIENTED_EDGE ( 'NONE', *, *, #18769, .F. ) ;
#45916 = EDGE_CURVE ( 'NONE', #43457, #25456, #2894, .T. ) ;
#45917 = DIRECTION ( 'NONE',  ( -0.7378332790417239107, 0.000000000000000000, -0.6749830015182142207 ) ) ;
#45918 = VECTOR ( 'NONE', #45095, 1000.000000000000114 ) ;
#45919 = ADVANCED_FACE ( 'NONE', ( #22871 ), #39402, .T. ) ;
#45920 = DIRECTION ( 'NONE',  ( 0.000000000000000000, 0.000000000000000000, -1.000000000000000000 ) ) ;
#45921 = VECTOR ( 'NONE', #43470, 1000.000000000000000 ) ;
#45923 = ORIENTED_EDGE ( 'NONE', *, *, #26613, .F. ) ;
#45922 = CARTESIAN_POINT ( 'NONE',  ( -173.4460699164830260, -175.3837268820161057, -2.874563619423225802 ) ) ;
#45924 = VECTOR ( 'NONE', #50275, 1000.000000000000114 ) ;
#45925 = AXIS2_PLACEMENT_3D ( 'NONE', #11865, #47115, #7437 ) ;
#45926 = EDGE_CURVE ( 'NONE', #9084, #32451, #30749, .T. ) ;
#45927 = AXIS2_PLACEMENT_3D ( 'NONE', #35055, #31359, #47148 ) ;
#45928 = DIRECTION ( 'NONE',  ( 0.000000000000000000, 1.000000000000000000, 0.000000000000000000 ) ) ;
#45929 = LINE ( 'NONE', #9914, #45846 ) ;
#45930 = ORIENTED_EDGE ( 'NONE', *, *, #3807, .F. ) ;
#45931 = EDGE_LOOP ( 'NONE', ( #36655, #46640, #5658, #14888 ) ) ;
#45932 = ADVANCED_FACE ( 'NONE', ( #23137 ), #50739, .T. ) ;
#45933 = ORIENTED_EDGE ( 'NONE', *, *, #27131, .T. ) ;
#45934 = CIRCLE ( 'NONE', #11505, 125.0000000000000000 ) ;
#45935 = DIRECTION ( 'NONE',  ( 0.000000000000000000, 0.000000000000000000, -1.000000000000000000 ) ) ;
#45936 = CARTESIAN_POINT ( 'NONE',  ( -330.4913330509368166, -78.25935320507895199, 39.41172259083835172 ) ) ;
#45937 = CARTESIAN_POINT ( 'NONE',  ( -336.3521761649654422, -73.44864141332200802, 31.34948880313848107 ) ) ;
#45938 = DIRECTION ( 'NONE',  ( -0.3482016354344059095, 0.000000000000000000, 0.9374196611341183427 ) ) ;
#45939 = CARTESIAN_POINT ( 'NONE',  ( -130.2106798473772642, -189.7472609257535510, 94.57776286494221551 ) ) ;
#45940 = ORIENTED_EDGE ( 'NONE', *, *, #40463, .F. ) ;
#45941 = EDGE_CURVE ( 'NONE', #14246, #33159, #35207, .T. ) ;
#45942 = EDGE_CURVE ( 'NONE', #6148, #37802, #34943, .T. ) ;
#45943 = PLANE ( 'NONE',  #31590 ) ;
#45944 = VERTEX_POINT ( 'NONE', #10518 ) ;
#45946 = ORIENTED_EDGE ( 'NONE', *, *, #42916, .F. ) ;
#45945 = LINE ( 'NONE', #29367, #19743 ) ;
#45947 = AXIS2_PLACEMENT_3D ( 'NONE', #36816, #1059, #40737 ) ;
#45948 = ORIENTED_EDGE ( 'NONE', *, *, #3033, .T. ) ;
#45949 = CIRCLE ( 'NONE', #50969, 60.00000000000000000 ) ;
#45950 = ORIENTED_EDGE ( 'NONE', *, *, #42964, .F. ) ;
#45951 = CARTESIAN_POINT ( 'NONE',  ( -48.36085358058748795, -189.7472609257535510, 0.9929810960135245779 ) ) ;
#45952 = CARTESIAN_POINT ( 'NONE',  ( -4.176930889631405464, -193.5000000000000000, 116.8859077982279615 ) ) ;
#45953 = ORIENTED_EDGE ( 'NONE', *, *, #25607, .T. ) ;
#45954 = AXIS2_PLACEMENT_3D ( 'NONE', #50193, #30203, #33874 ) ;
#45955 = LINE ( 'NONE', #1779, #19615 ) ;
#45956 = CARTESIAN_POINT ( 'NONE',  ( -332.3517673607765914, -67.40061919120938683, 18.46045550523129819 ) ) ;
#45957 = ORIENTED_EDGE ( 'NONE', *, *, #13811, .T. ) ;
#45958 = CARTESIAN_POINT ( 'NONE',  ( -126.3604277550461319, -183.6283474603465606, 96.49160960477098570 ) ) ;
#45959 = EDGE_LOOP ( 'NONE', ( #4665, #13365, #43734, #48844 ) ) ;
#45960 = ORIENTED_EDGE ( 'NONE', *, *, #14480, .F. ) ;
#45961 = CARTESIAN_POINT ( 'NONE',  ( 0.000000000000000000, -63.50000000000000000, 0.000000000000000000 ) ) ;
#45962 = AXIS2_PLACEMENT_3D ( 'NONE', #38983, #10111, #39257 ) ;
#45963 = CARTESIAN_POINT ( 'NONE',  ( -18.95304271317702671, -175.3837268820161057, -121.4627941443854979 ) ) ;
#45964 = VECTOR ( 'NONE', #40269, 1000.000000000000000 ) ;
#45965 = DIRECTION ( 'NONE',  ( -0.000000000000000000, -1.000000000000000000, -0.000000000000000000 ) ) ;
#45966 = DIRECTION ( 'NONE',  ( 0.9646355819083556327, 0.000000000000000000, 0.2635871660690782825 ) ) ;
#45967 = ORIENTED_EDGE ( 'NONE', *, *, #30472, .T. ) ;
#45968 = AXIS2_PLACEMENT_3D ( 'NONE', #26461, #18587, #34605 ) ;
#45969 = DIRECTION ( 'NONE',  ( 0.000000000000000000, -1.000000000000000000, 0.000000000000000000 ) ) ;
#45970 = DIRECTION ( 'NONE',  ( -0.000000000000000000, 1.000000000000000000, -0.000000000000000000 ) ) ;
#45971 = EDGE_CURVE ( 'NONE', #13962, #13126, #46799, .T. ) ;
#45972 = EDGE_CURVE ( 'NONE', #50885, #18264, #39150, .T. ) ;
#45973 = CARTESIAN_POINT ( 'NONE',  ( -330.4913330509368166, -123.5000000000000284, 0.000000000000000000 ) ) ;
#45974 = CARTESIAN_POINT ( 'NONE',  ( 0.000000000000000000, 101.9200652401092384, -101.2342171097734536 ) ) ;
#45975 = AXIS2_PLACEMENT_3D ( 'NONE', #14220, #26280, #42058 ) ;
#45976 = ORIENTED_EDGE ( 'NONE', *, *, #5144, .F. ) ;
#45977 = CARTESIAN_POINT ( 'NONE',  ( -330.4913330509368166, -156.6043281241916816, -48.84008046109114076 ) ) ;
#45978 = DIRECTION ( 'NONE',  ( 0.000000000000000000, 1.000000000000000000, 0.000000000000000000 ) ) ;
#45979 = EDGE_CURVE ( 'NONE', #14211, #20982, #3407, .T. ) ;
#45980 = VECTOR ( 'NONE', #19233, 1000.000000000000000 ) ;
#45981 = ADVANCED_FACE ( 'NONE', ( #38891 ), #18927, .T. ) ;
#45982 = CARTESIAN_POINT ( 'NONE',  ( -330.4913330509368166, -102.1108035431471279, 54.98865587491800255 ) ) ;
#45983 = ORIENTED_EDGE ( 'NONE', *, *, #35606, .T. ) ;
#45984 = CARTESIAN_POINT ( 'NONE',  ( -332.3517673607765914, -123.5000000000000284, 0.000000000000000000 ) ) ;
#45985 = FACE_OUTER_BOUND ( 'NONE', #34525, .T. ) ;
#45986 = DIRECTION ( 'NONE',  ( -0.000000000000000000, 1.000000000000000000, -0.000000000000000000 ) ) ;
#45987 = VERTEX_POINT ( 'NONE', #15248 ) ;
#45988 = ORIENTED_EDGE ( 'NONE', *, *, #18270, .F. ) ;
#45989 = ORIENTED_EDGE ( 'NONE', *, *, #30393, .F. ) ;
#45990 = CARTESIAN_POINT ( 'NONE',  ( -173.4724443937511751, -183.6283474603465606, 1.292495564989516454 ) ) ;
#45991 = AXIS2_PLACEMENT_3D ( 'NONE', #45687, #5755, #21770 ) ;
#45992 = LINE ( 'NONE', #1813, #31224 ) ;
#45993 = DIRECTION ( 'NONE',  ( 0.000000000000000000, 0.000000000000000000, 1.000000000000000000 ) ) ;
#45994 = VECTOR ( 'NONE', #17218, 1000.000000000000114 ) ;
#45995 = CARTESIAN_POINT ( 'NONE',  ( -339.1964088526558498, -79.66942718702493664, 39.49849221029193558 ) ) ;
#45996 = DIRECTION ( 'NONE',  ( -1.000000000000000000, 0.000000000000000000, -0.000000000000000000 ) ) ;
#45997 = EDGE_LOOP ( 'NONE', ( #22609, #37652, #12786, #17696 ) ) ;
#45998 = EDGE_CURVE ( 'NONE', #17654, #43748, #26550, .T. ) ;
#45999 = DIRECTION ( 'NONE',  ( 0.000000000000000000, 0.000000000000000000, 1.000000000000000000 ) ) ;
#46000 = ORIENTED_EDGE ( 'NONE', *, *, #30039, .T. ) ;
#46001 = DIRECTION ( 'NONE',  ( -0.000000000000000000, -0.7485107481710953081, 0.6631226582408016323 ) ) ;
#46002 = VECTOR ( 'NONE', #35051, 999.9999999999998863 ) ;
#46003 = VERTEX_POINT ( 'NONE', #15004 ) ;
#46004 = FACE_OUTER_BOUND ( 'NONE', #15897, .T. ) ;
#46005 = ORIENTED_EDGE ( 'NONE', *, *, #2217, .F. ) ;
#46006 = VECTOR ( 'NONE', #47543, 1000.000000000000000 ) ;
#46007 = CARTESIAN_POINT ( 'NONE',  ( -365.0000000000001137, -78.50000000000002842, -10.00000000000000711 ) ) ;
#46008 = DIRECTION ( 'NONE',  ( -0.000000000000000000, -0.7485107481711046340, -0.6631226582407911962 ) ) ;
#46009 = ORIENTED_EDGE ( 'NONE', *, *, #39678, .F. ) ;
#46012 = VERTEX_POINT ( 'NONE', #3157 ) ;
#46011 = DIRECTION ( 'NONE',  ( 0.000000000000000000, -1.000000000000000000, 0.000000000000000000 ) ) ;
#46010 = CARTESIAN_POINT ( 'NONE',  ( -4.237343245523132573, 55.36427016545908231, -17.76729481263095067 ) ) ;
#46013 = PLANE ( 'NONE',  #21456 ) ;
#46014 = VERTEX_POINT ( 'NONE', #7103 ) ;
#46015 = PLANE ( 'NONE',  #46620 ) ;
#46016 = ORIENTED_EDGE ( 'NONE', *, *, #17258, .F. ) ;
#46017 = DIRECTION ( 'NONE',  ( 0.000000000000000000, 0.000000000000000000, -1.000000000000000000 ) ) ;
#46020 = EDGE_LOOP ( 'NONE', ( #27811, #30867, #7979, #22128 ) ) ;
#46019 = DIRECTION ( 'NONE',  ( 1.043714542225393381E-14, -0.4647231720437695057, -0.8854560256532093554 ) ) ;
#46018 = CARTESIAN_POINT ( 'NONE',  ( -330.4913330509368166, -64.50000000000000000, -0.4999999999999549249 ) ) ;
#46021 = EDGE_LOOP ( 'NONE', ( #35683, #15435 ) ) ;
#46022 = DIRECTION ( 'NONE',  ( -0.8757349421956379665, 0.000000000000000000, 0.4827922027307427477 ) ) ;
#46023 =( GEOMETRIC_REPRESENTATION_CONTEXT ( 3 ) GLOBAL_UNCERTAINTY_ASSIGNED_CONTEXT ( ( #1713 ) ) GLOBAL_UNIT_ASSIGNED_CONTEXT ( ( #20522, #39453, #291 ) ) REPRESENTATION_CONTEXT ( 'NONE', 'WORKASPACE' ) );
#46024 = ORIENTED_EDGE ( 'NONE', *, *, #28541, .F. ) ;
#46025 = DIRECTION ( 'NONE',  ( 0.000000000000000000, -0.9350162426854181641, -0.3546048870425267951 ) ) ;
#46026 = CONICAL_SURFACE ( 'NONE', #9922, 10.00000000000000711, 0.03490658503988659789 ) ;
#46027 = CARTESIAN_POINT ( 'NONE',  ( -339.1964088526558498, -78.92247586331968989, 40.16023333900940173 ) ) ;
#46028 = ORIENTED_EDGE ( 'NONE', *, *, #19716, .F. ) ;
#46029 = LINE ( 'NONE', #34179, #50703 ) ;
#46030 = CARTESIAN_POINT ( 'NONE',  ( -330.4913330509368166, -90.39567187580801999, 48.84008046109089918 ) ) ;
#46031 = CARTESIAN_POINT ( 'NONE',  ( -336.3521761649654422, -100.1170788342122080, 54.23253582808833073 ) ) ;
#46032 = PLANE ( 'NONE',  #13392 ) ;
#46033 = VECTOR ( 'NONE', #43894, 1000.000000000000000 ) ;
#46034 = DIRECTION ( 'NONE',  ( -8.718379230999708359E-17, 0.5680647467311569221, 0.8229838658936556861 ) ) ;
#46035 = EDGE_LOOP ( 'NONE', ( #8857, #47191, #10396, #39570 ) ) ;
#46036 = EDGE_CURVE ( 'NONE', #47996, #51413, #22357, .T. ) ;
#46037 =( NAMED_UNIT ( * ) SI_UNIT ( $, .STERADIAN. ) SOLID_ANGLE_UNIT ( ) );
#46038 = DIRECTION ( 'NONE',  ( 0.000000000000000000, 0.000000000000000000, 1.000000000000000000 ) ) ;
#46039 = CARTESIAN_POINT ( 'NONE',  ( -48.47912675150885065, -175.3837268820161057, 6.938893903907228378E-15 ) ) ;
#46040 = CARTESIAN_POINT ( 'NONE',  ( -170.2790847791494855, -183.6283474603465606, -28.10285082451569494 ) ) ;
#46041 = ORIENTED_EDGE ( 'NONE', *, *, #22642, .T. ) ;
#46042 = VECTOR ( 'NONE', #2853, 1000.000000000000000 ) ;
#46043 = CARTESIAN_POINT ( 'NONE',  ( -105.8382074681673117, -193.5000000000000000, -109.9360785596604586 ) ) ;
#46044 = PLANE ( 'NONE',  #21932 ) ;
#46045 = CARTESIAN_POINT ( 'NONE',  ( -7.515176836080578404, -193.5000000000000000, 117.0391155081705250 ) ) ;
#46046 = CARTESIAN_POINT ( 'NONE',  ( -48.47912675150885065, -183.6283474603465606, 6.938893903907228378E-15 ) ) ;
#46048 = AXIS2_PLACEMENT_3D ( 'NONE', #18658, #27039, #30991 ) ;
#46047 = DIRECTION ( 'NONE',  ( -0.000000000000000000, -0.8229838658936516893, 0.5680647467311626952 ) ) ;
#46049 = DIRECTION ( 'NONE',  ( 0.9995608365087944591, 0.000000000000000000, -0.02963332782255633305 ) ) ;
#46050 = ADVANCED_FACE ( 'NONE', ( #2637 ), #38382, .T. ) ;
#46051 = DIRECTION ( 'NONE',  ( 0.000000000000000000, -1.000000000000000000, 0.000000000000000000 ) ) ;
#46052 = CARTESIAN_POINT ( 'NONE',  ( -46.00000000000000711, 0.000000000000000000, -4.999999999999988454 ) ) ;
#46053 = ORIENTED_EDGE ( 'NONE', *, *, #2576, .F. ) ;
#46054 = DIRECTION ( 'NONE',  ( 1.000000000000000000, -0.000000000000000000, -0.000000000000000000 ) ) ;
#46055 = CARTESIAN_POINT ( 'NONE',  ( -59.28786813212836648, -183.6283474603465606, 124.5318076226587465 ) ) ;
#46057 = ORIENTED_EDGE ( 'NONE', *, *, #5091, .F. ) ;
#46056 = CARTESIAN_POINT ( 'NONE',  ( -339.1964088526558498, -179.4217241332784454, -21.74306257088698757 ) ) ;
#46058 = AXIS2_PLACEMENT_3D ( 'NONE', #631, #27702, #47945 ) ;
#46059 = ORIENTED_EDGE ( 'NONE', *, *, #45916, .T. ) ;
#46060 = PRESENTATION_LAYER_ASSIGNMENT (  '', '', ( #7446 ) ) ;
#46061 = ORIENTED_EDGE ( 'NONE', *, *, #5327, .F. ) ;
#46062 = DIRECTION ( 'NONE',  ( 0.000000000000000000, 0.000000000000000000, -1.000000000000000000 ) ) ;
#46063 = VECTOR ( 'NONE', #5467, 1000.000000000000000 ) ;
#46064 = ADVANCED_FACE ( 'NONE', ( #27320 ), #43367, .T. ) ;
#46065 = CARTESIAN_POINT ( 'NONE',  ( -145.0195698084541505, -193.5000000000000000, 79.40367028273128369 ) ) ;
#46066 = CARTESIAN_POINT ( 'NONE',  ( -47.63353074800703268, -175.3837268820161057, 0.5338233779648018373 ) ) ;
#46067 = ORIENTED_EDGE ( 'NONE', *, *, #38812, .F. ) ;
#46068 = CARTESIAN_POINT ( 'NONE',  ( 1.734723475976807489E-15, -43.50000000000000000, -30.00000000000000711 ) ) ;
#46069 = DIRECTION ( 'NONE',  ( 0.000000000000000000, 0.000000000000000000, -1.000000000000000000 ) ) ;
#46070 = VECTOR ( 'NONE', #6232, 1000.000000000000114 ) ;
#46072 = ORIENTED_EDGE ( 'NONE', *, *, #29214, .F. ) ;
#46071 = DIRECTION ( 'NONE',  ( 0.000000000000000000, 0.7485107481711046340, 0.6631226582407911962 ) ) ;
#46073 = EDGE_CURVE ( 'NONE', #6422, #47448, #3666, .T. ) ;
#46074 = DIRECTION ( 'NONE',  ( -0.9564009842765223146, 0.000000000000000000, -0.2920567706369764371 ) ) ;
#46075 = ORIENTED_EDGE ( 'NONE', *, *, #47814, .T. ) ;
#46076 = DIRECTION ( 'NONE',  ( 0.000000000000000000, 0.5000000000000012212, -0.8660254037844379305 ) ) ;
#46077 = ORIENTED_EDGE ( 'NONE', *, *, #26485, .F. ) ;
#46078 = CARTESIAN_POINT ( 'NONE',  ( -48.47912675150885065, -175.3837268820161057, 6.938893903907228378E-15 ) ) ;
#46079 = LINE ( 'NONE', #14788, #47314 ) ;
#46080 = LINE ( 'NONE', #37125, #24042 ) ;
#46081 = VECTOR ( 'NONE', #44332, 1000.000000000000000 ) ;
#46082 = EDGE_CURVE ( 'NONE', #21402, #22201, #28084, .T. ) ;
#46083 = ORIENTED_EDGE ( 'NONE', *, *, #8802, .F. ) ;
#46084 = VERTEX_POINT ( 'NONE', #27830 ) ;
#46085 = PLANE ( 'NONE',  #13057 ) ;
#46086 = CARTESIAN_POINT ( 'NONE',  ( 72.95485052494851175, -193.5000000000000000, -29.64437826672757481 ) ) ;
#46087 = ORIENTED_EDGE ( 'NONE', *, *, #45218, .T. ) ;
#46088 = PLANE ( 'NONE',  #23214 ) ;
#46089 = ORIENTED_EDGE ( 'NONE', *, *, #9347, .F. ) ;
#46090 = EDGE_CURVE ( 'NONE', #18701, #20460, #12587, .T. ) ;
#46091 = DIRECTION ( 'NONE',  ( -0.000000000000000000, 1.000000000000000000, -0.000000000000000000 ) ) ;
#46092 = EDGE_CURVE ( 'NONE', #903, #37560, #16555, .T. ) ;
#46093 = FACE_OUTER_BOUND ( 'NONE', #50258, .T. ) ;
#46094 = EDGE_LOOP ( 'NONE', ( #26469, #29479 ) ) ;
#46095 = DIRECTION ( 'NONE',  ( 0.000000000000000000, 0.000000000000000000, 1.000000000000000000 ) ) ;
#46096 = ORIENTED_EDGE ( 'NONE', *, *, #13331, .T. ) ;
#46097 = EDGE_CURVE ( 'NONE', #39066, #22193, #24676, .T. ) ;
#46098 = LINE ( 'NONE', #49253, #4427 ) ;
#46099 = AXIS2_PLACEMENT_3D ( 'NONE', #16829, #32833, #48885 ) ;
#46100 = CARTESIAN_POINT ( 'NONE',  ( -48.65601702663141737, -177.1207230881787780, -0.9842305779475923888 ) ) ;
#46101 = DIRECTION ( 'NONE',  ( -0.000000000000000000, 1.000000000000000000, -0.000000000000000000 ) ) ;
#46102 = EDGE_LOOP ( 'NONE', ( #39004, #1256, #16827, #30056 ) ) ;
#46103 = CIRCLE ( 'NONE', #23426, 16.00000000000000355 ) ;
#46104 = DIRECTION ( 'NONE',  ( 0.000000000000000000, 0.000000000000000000, -1.000000000000000000 ) ) ;
#46105 = DIRECTION ( 'NONE',  ( -8.718379230999707126E-17, 1.000000000000000000, -3.491481338843133355E-15 ) ) ;
#46106 = CARTESIAN_POINT ( 'NONE',  ( -339.1964088526558498, -115.8919814278862503, 58.50955523165745831 ) ) ;
#46107 = ORIENTED_EDGE ( 'NONE', *, *, #39706, .T. ) ;
#46108 = CARTESIAN_POINT ( 'NONE',  ( -336.3521761649654422, -163.8460225846223466, -43.07972642080364523 ) ) ;
#46109 = ORIENTED_EDGE ( 'NONE', *, *, #37169, .T. ) ;
#46110 = AXIS2_PLACEMENT_3D ( 'NONE', #33296, #25162, #12547 ) ;
#46111 = EDGE_CURVE ( 'NONE', #11646, #30315, #15508, .T. ) ;
#46112 = CARTESIAN_POINT ( 'NONE',  ( -121.1142239062970418, -177.1207230881787780, 101.7307360698549132 ) ) ;
#46114 = ORIENTED_EDGE ( 'NONE', *, *, #26313, .T. ) ;
#46113 = CARTESIAN_POINT ( 'NONE',  ( -336.3521761649654422, -154.8494888031386836, 50.05135858667791382 ) ) ;
#46115 = ORIENTED_EDGE ( 'NONE', *, *, #22895, .F. ) ;
#46116 = CYLINDRICAL_SURFACE ( 'NONE', #571, 125.0000000000000000 ) ;
#46117 = EDGE_CURVE ( 'NONE', #38778, #32529, #40584, .T. ) ;
#46118 = VECTOR ( 'NONE', #33657, 1000.000000000000000 ) ;
#46119 = DIRECTION ( 'NONE',  ( -1.000000000000000000, 2.497772389992407926E-15, -1.013386094502326665E-14 ) ) ;
#46120 = EDGE_LOOP ( 'NONE', ( #11072, #1262, #14065, #35918 ) ) ;
#46121 = CARTESIAN_POINT ( 'NONE',  ( -149.1282321233095161, -175.3837268820161057, -72.42760398749013007 ) ) ;
#46122 = ORIENTED_EDGE ( 'NONE', *, *, #2575, .F. ) ;
#46123 = DIRECTION ( 'NONE',  ( -0.000000000000000000, 1.000000000000000000, -0.000000000000000000 ) ) ;
#46124 = CARTESIAN_POINT ( 'NONE',  ( 2.669657140899367676, -175.3837268820161057, 114.0561348912355726 ) ) ;
#46125 = DIRECTION ( 'NONE',  ( 0.000000000000000000, -0.000000000000000000, 1.000000000000000000 ) ) ;
#46126 = CARTESIAN_POINT ( 'NONE',  ( -48.07600332222087758, -183.6283474603465606, -0.9151456172430111335 ) ) ;
#46127 = VERTEX_POINT ( 'NONE', #32033 ) ;
#46128 = VERTEX_POINT ( 'NONE', #28610 ) ;
#46129 = VERTEX_POINT ( 'NONE', #44407 ) ;
#46130 = CARTESIAN_POINT ( 'NONE',  ( -166.9492939735806090, -193.5000000000000000, 39.87254040532603483 ) ) ;
#46131 = DIRECTION ( 'NONE',  ( 0.000000000000000000, 1.000000000000000000, -0.000000000000000000 ) ) ;
#46132 = CIRCLE ( 'NONE', #43593, 60.00000000000000000 ) ;
#46133 = DIRECTION ( 'NONE',  ( -0.9785564922995032555, 0.000000000000000000, -0.2059786187411021818 ) ) ;
#46134 = CARTESIAN_POINT ( 'NONE',  ( -336.3521761649653854, -90.77207769297352513, -50.28800156563429624 ) ) ;
#46135 = ORIENTED_EDGE ( 'NONE', *, *, #5033, .T. ) ;
#46136 = AXIS2_PLACEMENT_3D ( 'NONE', #46068, #28767, #49026 ) ;
#46137 = ADVANCED_FACE ( 'NONE', ( #31521 ), #8136, .T. ) ;
#46138 = EDGE_CURVE ( 'NONE', #29888, #48694, #44657, .T. ) ;
#46139 = PLANE ( 'NONE',  #43318 ) ;
#46140 = EDGE_LOOP ( 'NONE', ( #44357, #3161, #29252, #39041 ) ) ;
#46142 = ORIENTED_EDGE ( 'NONE', *, *, #11005, .F. ) ;
#46141 = CARTESIAN_POINT ( 'NONE',  ( -122.3978016498073345, -183.6283474603465606, -100.8019320314827070 ) ) ;
#46143 = DIRECTION ( 'NONE',  ( 0.000000000000000000, 0.5680647467311656929, 0.8229838658936495799 ) ) ;
#46144 = DIRECTION ( 'NONE',  ( 1.000000000000000000, -0.000000000000000000, -0.000000000000000000 ) ) ;
#46145 = DIRECTION ( 'NONE',  ( -0.000000000000000000, 1.000000000000000000, -0.000000000000000000 ) ) ;
#46146 = LINE ( 'NONE', #10129, #27638 ) ;
#46147 = ORIENTED_EDGE ( 'NONE', *, *, #30745, .F. ) ;
#46148 = EDGE_CURVE ( 'NONE', #31562, #13288, #47576, .T. ) ;
#46149 = CARTESIAN_POINT ( 'NONE',  ( -104.8182102393454045, -193.5000000000000000, 111.5836353223472912 ) ) ;
#46150 = ORIENTED_EDGE ( 'NONE', *, *, #22460, .T. ) ;
#46151 = ADVANCED_FACE ( 'NONE', ( #233 ), #7866, .F. ) ;
#46152 = VECTOR ( 'NONE', #1177, 1000.000000000000114 ) ;
#46153 = ORIENTED_EDGE ( 'NONE', *, *, #22996, .T. ) ;
#46154 = CARTESIAN_POINT ( 'NONE',  ( -332.3517673607765914, -64.61288906875131488, 4.498567634385603142 ) ) ;
#46155 = EDGE_CURVE ( 'NONE', #50347, #3155, #43614, .T. ) ;
#46156 = DIRECTION ( 'NONE',  ( -1.000000000000000000, 0.000000000000000000, 0.000000000000000000 ) ) ;
#46157 = EDGE_LOOP ( 'NONE', ( #10575, #48256 ) ) ;
#46158 = EDGE_CURVE ( 'NONE', #27204, #41453, #35563, .T. ) ;
#46159 = CARTESIAN_POINT ( 'NONE',  ( -78.64590280292340196, -189.7472609257535510, -121.3052580173827266 ) ) ;
#46160 = LINE ( 'NONE', #46408, #29723 ) ;
#46161 = CARTESIAN_POINT ( 'NONE',  ( 75.28414827670442833, -177.1207230881787780, -7.666780576874956843 ) ) ;
#46162 = DIRECTION ( 'NONE',  ( -0.000000000000000000, 1.000000000000000000, -0.000000000000000000 ) ) ;
#46163 = FACE_OUTER_BOUND ( 'NONE', #44795, .T. ) ;
#46164 = ADVANCED_FACE ( 'NONE', ( #35722 ), #39910, .F. ) ;
#46165 = ORIENTED_EDGE ( 'NONE', *, *, #45214, .F. ) ;
#46166 = VECTOR ( 'NONE', #46054, 1000.000000000000000 ) ;
#46167 = CYLINDRICAL_SURFACE ( 'NONE', #10400, 125.0000000000000000 ) ;
#46168 = ORIENTED_EDGE ( 'NONE', *, *, #46865, .T. ) ;
#46169 = VERTEX_POINT ( 'NONE', #16279 ) ;
#46170 = CARTESIAN_POINT ( 'NONE',  ( -305.0000000000000568, -116.7644047441726656, 59.62073260661660612 ) ) ;
#46171 = EDGE_LOOP ( 'NONE', ( #8735, #30915, #2666, #9130 ) ) ;
#46172 = PRODUCT_DEFINITION_SHAPE ( 'NONE', 'NONE',  #19619 ) ;
#46173 = DIRECTION ( 'NONE',  ( 0.000000000000000000, 0.000000000000000000, 1.000000000000000000 ) ) ;
#46174 = DIRECTION ( 'NONE',  ( -0.8757349421956412971, 0.000000000000000000, 0.4827922027307366970 ) ) ;
#46176 = VERTEX_POINT ( 'NONE', #35996 ) ;
#46175 = CARTESIAN_POINT ( 'NONE',  ( -173.4787860028527007, -177.1207230881787780, 0.2918682030023981300 ) ) ;
#46177 = EDGE_LOOP ( 'NONE', ( #11667, #32399 ) ) ;
#46178 = CARTESIAN_POINT ( 'NONE',  ( -336.3521761649654422, -65.24746378767824240, -9.724760635741734660 ) ) ;
#46179 = DIRECTION ( 'NONE',  ( 0.8896570909947436601, 0.000000000000000000, 0.4566292373937200777 ) ) ;
#46180 = DIRECTION ( 'NONE',  ( 0.000000000000000000, -0.000000000000000000, -1.000000000000000000 ) ) ;
#46181 = EDGE_LOOP ( 'NONE', ( #12926, #44577 ) ) ;
#46182 = VERTEX_POINT ( 'NONE', #44131 ) ;
#46184 = VERTEX_POINT ( 'NONE', #48079 ) ;
#46183 = VECTOR ( 'NONE', #47717, 1000.000000000000000 ) ;
#46185 = DIRECTION ( 'NONE',  ( -0.000000000000000000, 0.9350162426854181641, 0.3546048870425267951 ) ) ;
#46186 = PLANE ( 'NONE',  #45329 ) ;
#46187 = ADVANCED_FACE ( 'NONE', ( #32289 ), #24174, .T. ) ;
#46188 = CARTESIAN_POINT ( 'NONE',  ( -18.95304271317703382, -189.7472609257535510, -121.4627941443854837 ) ) ;
#46189 = LINE ( 'NONE', #10168, #50510 ) ;
#46190 = DIRECTION ( 'NONE',  ( 0.000000000000000000, -1.000000000000000000, 0.000000000000000000 ) ) ;
#46191 = ORIENTED_EDGE ( 'NONE', *, *, #22112, .F. ) ;
#46192 = EDGE_CURVE ( 'NONE', #12138, #10791, #36490, .T. ) ;
#46193 = EDGE_CURVE ( 'NONE', #14965, #49533, #4987, .T. ) ;
#46194 = EDGE_CURVE ( 'NONE', #32451, #44682, #39752, .T. ) ;
#46195 = ADVANCED_FACE ( 'NONE', ( #21785 ), #45704, .F. ) ;
#46196 = LINE ( 'NONE', #26722, #7256 ) ;
#46197 = VERTEX_POINT ( 'NONE', #21526 ) ;
#46199 = EDGE_LOOP ( 'NONE', ( #13030, #11701, #11887, #18290 ) ) ;
#46198 = CARTESIAN_POINT ( 'NONE',  ( -144.2430459457361280, -175.3837268820161057, 78.77358243914956404 ) ) ;
#46200 = ORIENTED_EDGE ( 'NONE', *, *, #38757, .T. ) ;
#46201 = AXIS2_PLACEMENT_3D ( 'NONE', #5795, #1819, #30445 ) ;
#46202 = EDGE_CURVE ( 'NONE', #8114, #10774, #13633, .T. ) ;
#46203 = DIRECTION ( 'NONE',  ( 0.000000000000000000, 0.000000000000000000, -1.000000000000000000 ) ) ;
#46204 = ORIENTED_EDGE ( 'NONE', *, *, #11587, .T. ) ;
#46205 = PLANE ( 'NONE',  #46773 ) ;
#46206 = VERTEX_POINT ( 'NONE', #25462 ) ;
#46207 = CARTESIAN_POINT ( 'NONE',  ( -365.0160704661291788, -113.5000000000000000, -40.00000000000001421 ) ) ;
#46208 = DIRECTION ( 'NONE',  ( 0.7378332790417285736, 0.000000000000000000, -0.6749830015182091136 ) ) ;
#46209 = VERTEX_POINT ( 'NONE', #37555 ) ;
#46210 = EDGE_CURVE ( 'NONE', #6055, #2868, #47331, .T. ) ;
#46211 = CARTESIAN_POINT ( 'NONE',  ( -305.0000000000000568, -78.92247586331968989, 40.16023333900940884 ) ) ;
#46212 = VERTEX_POINT ( 'NONE', #1798 ) ;
#46213 = ADVANCED_FACE ( 'NONE', ( #45446 ), #9962, .T. ) ;
#46214 = ORIENTED_EDGE ( 'NONE', *, *, #35540, .F. ) ;
#46215 = CARTESIAN_POINT ( 'NONE',  ( -108.4791267515088435, -132.5479369270331915, 60.00000000000002132 ) ) ;
#46216 = LINE ( 'NONE', #2822, #13858 ) ;
#46217 = ADVANCED_FACE ( 'NONE', ( #41479 ), #25978, .T. ) ;
#46218 = CARTESIAN_POINT ( 'NONE',  ( -23.01747912075234836, -177.1207230881787780, -122.3793467049370634 ) ) ;
#46219 = DIRECTION ( 'NONE',  ( 0.000000000000000000, -0.9350162426854181641, -0.3546048870425267951 ) ) ;
#46220 = ORIENTED_EDGE ( 'NONE', *, *, #28920, .F. ) ;
#46221 = CARTESIAN_POINT ( 'NONE',  ( -133.8011377042516301, -183.6283474603465606, -91.35181687837437892 ) ) ;
#46222 = LINE ( 'NONE', #26217, #31477 ) ;
#46223 = EDGE_CURVE ( 'NONE', #11668, #3041, #33604, .T. ) ;
#46224 = CARTESIAN_POINT ( 'NONE',  ( -55.05561436132772002, -175.3837268820161057, 124.8268793598474105 ) ) ;
#46225 = DIRECTION ( 'NONE',  ( -0.9890401873221623674, 0.000000000000000000, -0.1476465640024917925 ) ) ;
#46226 = ORIENTED_EDGE ( 'NONE', *, *, #20266, .F. ) ;
#46227 = CARTESIAN_POINT ( 'NONE',  ( 19.33815737959698566, -183.6283474603465606, 105.0038855142078233 ) ) ;
#46228 = CARTESIAN_POINT ( 'NONE',  ( -49.45768324380835423, -193.5000000000000000, -0.2059786187411025149 ) ) ;
#46229 = EDGE_CURVE ( 'NONE', #40642, #16896, #28869, .T. ) ;
#46230 = AXIS2_PLACEMENT_3D ( 'NONE', #27620, #39437, #43128 ) ;
#46231 = AXIS2_PLACEMENT_3D ( 'NONE', #30555, #10857, #34252 ) ;
#46232 = DIRECTION ( 'NONE',  ( -0.000000000000000000, -1.000000000000000000, -0.000000000000000000 ) ) ;
#46233 = EDGE_LOOP ( 'NONE', ( #26456, #25177, #22015, #14950 ) ) ;
#46234 = DIRECTION ( 'NONE',  ( -0.000000000000000000, 1.000000000000000000, -0.000000000000000000 ) ) ;
#46235 = LINE ( 'NONE', #18372, #26092 ) ;
#46236 = ORIENTED_EDGE ( 'NONE', *, *, #31394, .T. ) ;
#46237 = CARTESIAN_POINT ( 'NONE',  ( -161.2555905272864436, -175.3837268820161057, -53.91167979418489864 ) ) ;
#46238 = ORIENTED_EDGE ( 'NONE', *, *, #30039, .F. ) ;
#46239 = EDGE_CURVE ( 'NONE', #35941, #45486, #13380, .T. ) ;
#46240 = LINE ( 'NONE', #10214, #7485 ) ;
#46241 = VECTOR ( 'NONE', #24572, 1000.000000000000227 ) ;
#46242 = CARTESIAN_POINT ( 'NONE',  ( 60.00000000000001421, -113.5000000000000000, 60.00000000000000711 ) ) ;
#46243 = LINE ( 'NONE', #14186, #13617 ) ;
#46244 = CARTESIAN_POINT ( 'NONE',  ( 57.66105628977221897, -175.3837268820161057, 66.02470404298190942 ) ) ;
#46245 = CARTESIAN_POINT ( 'NONE',  ( -19.28375372365792728, -175.3837268820161057, 121.5427093402341256 ) ) ;
#46246 = ORIENTED_EDGE ( 'NONE', *, *, #38489, .F. ) ;
#46247 = LINE ( 'NONE', #38338, #457 ) ;
#46248 = VERTEX_POINT ( 'NONE', #17593 ) ;
#46249 = EDGE_CURVE ( 'NONE', #38006, #41381, #41423, .T. ) ;
#46250 = CARTESIAN_POINT ( 'NONE',  ( -151.4272465800706300, -183.6283474603465606, 70.89911581792885897 ) ) ;
#46251 = VERTEX_POINT ( 'NONE', #29392 ) ;
#46252 = LINE ( 'NONE', #26253, #15032 ) ;
#46253 = VECTOR ( 'NONE', #28672, 1000.000000000000114 ) ;
#46254 = ADVANCED_FACE ( 'NONE', ( #33081 ), #13897, .T. ) ;
#46255 = ADVANCED_FACE ( 'NONE', ( #13112 ), #49644, .T. ) ;
#46256 = EDGE_CURVE ( 'NONE', #19012, #34105, #29681, .T. ) ;
#46257 = EDGE_CURVE ( 'NONE', #47856, #34569, #771, .T. ) ;
#46258 = CIRCLE ( 'NONE', #44555, 20.00000000000001776 ) ;
#46259 = CARTESIAN_POINT ( 'NONE',  ( -48.47912675150885065, -183.6283474603465606, 6.938893903907228378E-15 ) ) ;
#46260 = DIRECTION ( 'NONE',  ( -1.000000000000000000, 0.000000000000000000, -0.000000000000000000 ) ) ;
#46261 = ORIENTED_EDGE ( 'NONE', *, *, #34404, .F. ) ;
#46264 = ORIENTED_EDGE ( 'NONE', *, *, #552, .T. ) ;
#46263 = CARTESIAN_POINT ( 'NONE',  ( -49.17567778057184569, -175.3837268820161057, -0.7175072570443327136 ) ) ;
#46262 = DIRECTION ( 'NONE',  ( -0.000000000000000000, -0.4647231720437724478, -0.8854560256532078011 ) ) ;
#46265 = DIRECTION ( 'NONE',  ( 1.000000000000000000, -0.000000000000000000, -0.000000000000000000 ) ) ;
#46266 = ORIENTED_EDGE ( 'NONE', *, *, #25312, .T. ) ;
#46267 = DIRECTION ( 'NONE',  ( 0.000000000000000000, 0.000000000000000000, 1.000000000000000000 ) ) ;
#46268 = EDGE_LOOP ( 'NONE', ( #10871, #36912, #47795, #13573 ) ) ;
#46269 = DIRECTION ( 'NONE',  ( 1.000000000000000000, 0.000000000000000000, -0.000000000000000000 ) ) ;
#46272 = VERTEX_POINT ( 'NONE', #32820 ) ;
#46271 = CARTESIAN_POINT ( 'NONE',  ( -166.9492939735806090, -189.7472609257535510, 39.87254040532606325 ) ) ;
#46270 = CARTESIAN_POINT ( 'NONE',  ( -339.1964088526558498, -144.8891964568517778, 54.98865587491845730 ) ) ;
#46273 = EDGE_LOOP ( 'NONE', ( #17624, #19988, #10617, #19476 ) ) ;
#46274 = CARTESIAN_POINT ( 'NONE',  ( -153.4237445717492392, -193.5000000000000000, 66.05018866041351089 ) ) ;
#46275 = ORIENTED_EDGE ( 'NONE', *, *, #964, .T. ) ;
#46276 = DIRECTION ( 'NONE',  ( -0.000000000000000000, -1.000000000000000000, -0.000000000000000000 ) ) ;
#46278 = CIRCLE ( 'NONE', #28644, 124.9999999999999858 ) ;
#46277 = DIRECTION ( 'NONE',  ( 0.000000000000000000, -1.000000000000000000, 0.000000000000000000 ) ) ;
#46279 = EDGE_CURVE ( 'NONE', #51589, #44868, #2580, .T. ) ;
#46280 = ORIENTED_EDGE ( 'NONE', *, *, #26945, .F. ) ;
#46281 = DIRECTION ( 'NONE',  ( 0.9995608365087946812, 0.000000000000000000, -0.02963332782254913048 ) ) ;
#46282 = CARTESIAN_POINT ( 'NONE',  ( 3.499092996509686644E-32, 65.00000000000000000, 0.000000000000000000 ) ) ;
#46283 = CARTESIAN_POINT ( 'NONE',  ( -339.1964088526558498, -68.15673923803930734, -20.45418021416698551 ) ) ;
#46284 = CARTESIAN_POINT ( 'NONE',  ( 36.19006208304271865, -193.5000000000000000, 90.59430563621340582 ) ) ;
#46285 = DIRECTION ( 'NONE',  ( -1.000000000000000000, 0.000000000000000000, 0.000000000000000000 ) ) ;
#46286 = ADVANCED_FACE ( 'NONE', ( #42253 ), #22288, .T. ) ;
#46287 = VERTEX_POINT ( 'NONE', #27256 ) ;
#46288 =( NAMED_UNIT ( * ) SI_UNIT ( $, .STERADIAN. ) SOLID_ANGLE_UNIT ( ) );
#46289 = CARTESIAN_POINT ( 'NONE',  ( -73.94077438226447896, -177.1207230881787780, 122.3793467049372481 ) ) ;
#46290 = FACE_OUTER_BOUND ( 'NONE', #29253, .T. ) ;
#46291 = ADVANCED_FACE ( 'NONE', ( #50426 ), #15192, .T. ) ;
#46292 = FACE_OUTER_BOUND ( 'NONE', #2030, .T. ) ;
#46293 = VERTEX_POINT ( 'NONE', #47258 ) ;
#46294 = CARTESIAN_POINT ( 'NONE',  ( -37.78865854180984485, -177.1207230881787780, -123.5388265266451242 ) ) ;
#46295 = CARTESIAN_POINT ( 'NONE',  ( -159.0901268547125653, -177.1207230881787780, 58.22548115875958530 ) ) ;
#46296 = AXIS2_PLACEMENT_3D ( 'NONE', #50104, #34563, #42729 ) ;
#46297 = PLANE ( 'NONE',  #5932 ) ;
#46298 = CARTESIAN_POINT ( 'NONE',  ( -84.85683048652070681, -193.5000000000000000, 118.5439281552633304 ) ) ;
#46299 = CIRCLE ( 'NONE', #957, 60.00000000000000000 ) ;
#46300 = CARTESIAN_POINT ( 'NONE',  ( -336.3521761649654422, -74.01670616005314685, 32.17247266903214609 ) ) ;
#46301 = CARTESIAN_POINT ( 'NONE',  ( -336.3521761649654422, -67.40061919120938683, 18.46045550523129819 ) ) ;
#46302 = DIRECTION ( 'NONE',  ( -0.000000000000000000, -0.9927088740980548609, -0.1205366802553164696 ) ) ;
#46303 = CARTESIAN_POINT ( 'NONE',  ( -166.6265240196292439, -189.7472609257535510, 40.81902153125349741 ) ) ;
#46304 = EDGE_LOOP ( 'NONE', ( #23857, #13591, #22492, #6929 ) ) ;
#46305 = LINE ( 'NONE', #30260, #4213 ) ;
#46306 = VECTOR ( 'NONE', #29143, 1000.000000000000114 ) ;
#46307 = CARTESIAN_POINT ( 'NONE',  ( -336.3521761649654422, -126.1322888500942270, -59.00000000000001421 ) ) ;
#46309 = ORIENTED_EDGE ( 'NONE', *, *, #46490, .T. ) ;
#46308 = DIRECTION ( 'NONE',  ( -0.2920567706369833760, 0.000000000000000000, 0.9564009842765202052 ) ) ;
#46310 = ORIENTED_EDGE ( 'NONE', *, *, #38706, .F. ) ;
#46311 = VECTOR ( 'NONE', #36740, 1000.000000000000000 ) ;
#46312 = ORIENTED_EDGE ( 'NONE', *, *, #24947, .T. ) ;
#46313 = LINE ( 'NONE', #2662, #26720 ) ;
#46314 = ADVANCED_FACE ( 'NONE', ( #34122 ), #6790, .F. ) ;
#46315 = EDGE_CURVE ( 'NONE', #39193, #26105, #14168, .T. ) ;
#46316 = DIRECTION ( 'NONE',  ( 0.02963332782256331357, 0.000000000000000000, -0.9995608365087942371 ) ) ;
#46317 = DIRECTION ( 'NONE',  ( 0.9720229140804089729, 0.000000000000000000, 0.2348860457809911206 ) ) ;
#46318 = VERTEX_POINT ( 'NONE', #50174 ) ;
#46319 = CARTESIAN_POINT ( 'NONE',  ( -339.1964088526558498, -109.8658467157464571, 57.40522506028071348 ) ) ;
#46320 = DIRECTION ( 'NONE',  ( 0.000000000000000000, 1.000000000000000000, 0.000000000000000000 ) ) ;
#46322 = EDGE_LOOP ( 'NONE', ( #48827, #23424, #39622, #23937 ) ) ;
#46321 = DIRECTION ( 'NONE',  ( -0.000000000000000000, 0.4647231720437789981, 0.8854560256532044704 ) ) ;
#46323 = DIRECTION ( 'NONE',  ( -0.000000000000000000, 1.000000000000000000, -0.000000000000000000 ) ) ;
#46324 = ORIENTED_EDGE ( 'NONE', *, *, #9124, .T. ) ;
#46325 = DIRECTION ( 'NONE',  ( 0.000000000000000000, 1.000000000000000000, -0.000000000000000000 ) ) ;
#46326 = AXIS2_PLACEMENT_3D ( 'NONE', #24733, #32341, #40746 ) ;
#46327 = ORIENTED_EDGE ( 'NONE', *, *, #48982, .T. ) ;
#46328 = CARTESIAN_POINT ( 'NONE',  ( -336.3521761649654422, -120.8677111499054320, 59.00000000000000000 ) ) ;
#46329 = CARTESIAN_POINT ( 'NONE',  ( -305.0000000000000568, -74.40671499923389831, 34.49419324804615172 ) ) ;
#46330 = AXIS2_PLACEMENT_3D ( 'NONE', #12766, #40889, #17255 ) ;
#46331 = CARTESIAN_POINT ( 'NONE',  ( -49.03777351731250889, -177.1207230881787780, 0.8294056854502042109 ) ) ;
#46332 = VECTOR ( 'NONE', #40508, 1000.000000000000000 ) ;
#46333 = ORIENTED_EDGE ( 'NONE', *, *, #38339, .T. ) ;
#46334 = CARTESIAN_POINT ( 'NONE',  ( -132.6364218684650211, -193.5000000000000000, 92.42591454022807795 ) ) ;
#46335 = FACE_OUTER_BOUND ( 'NONE', #37202, .T. ) ;
#46336 = ORIENTED_EDGE ( 'NONE', *, *, #27541, .T. ) ;
#46337 = EDGE_CURVE ( 'NONE', #23338, #31250, #2335, .T. ) ;
#46338 = CARTESIAN_POINT ( 'NONE',  ( -330.4913330509368166, -66.33409060400650503, 14.60509510167813474 ) ) ;
#46339 = CARTESIAN_POINT ( 'NONE',  ( 34.93559171950835918, -193.5000000000000000, -93.09664195018497423 ) ) ;
#46340 = VERTEX_POINT ( 'NONE', #7303 ) ;
#46341 = FACE_BOUND ( 'NONE', #40040, .T. ) ;
#46342 = VECTOR ( 'NONE', #16104, 1000.000000000000114 ) ;
#46343 = PLANE ( 'NONE',  #40732 ) ;
#46344 = EDGE_CURVE ( 'NONE', #31839, #47039, #26483, .T. ) ;
#46345 = ORIENTED_EDGE ( 'NONE', *, *, #41761, .T. ) ;
#46346 = CARTESIAN_POINT ( 'NONE',  ( -47.47956591500005885, -175.3837268820161057, 0.02963332782257025594 ) ) ;
#46347 = ORIENTED_EDGE ( 'NONE', *, *, #15071, .F. ) ;
#46348 = VECTOR ( 'NONE', #36773, 1000.000000000000000 ) ;
#46349 = VECTOR ( 'NONE', #37715, 1000.000000000000000 ) ;
#46350 = DIRECTION ( 'NONE',  ( 0.9982437317643210184, 0.000000000000000000, 0.05924062789372143423 ) ) ;
#46351 = DIRECTION ( 'NONE',  ( 0.000000000000000000, 1.000000000000000000, 0.000000000000000000 ) ) ;
#46352 = EDGE_LOOP ( 'NONE', ( #16525, #466, #13840, #51983 ) ) ;
#46353 = DIRECTION ( 'NONE',  ( 0.000000000000000000, 0.000000000000000000, -1.000000000000000000 ) ) ;
#46354 = LINE ( 'NONE', #22168, #11254 ) ;
#46355 = FACE_OUTER_BOUND ( 'NONE', #43711, .T. ) ;
#46356 = ORIENTED_EDGE ( 'NONE', *, *, #7872, .T. ) ;
#46357 = DIRECTION ( 'NONE',  ( 0.000000000000000000, 0.9709418174260553425, 0.2393156642875448881 ) ) ;
#46358 = VERTEX_POINT ( 'NONE', #38053 ) ;
#46359 = CARTESIAN_POINT ( 'NONE',  ( -123.6678354051270077, -193.5000000000000000, 99.85818990449067201 ) ) ;
#46360 = CARTESIAN_POINT ( 'NONE',  ( 40.71578595748727736, -193.5000000000000000, 86.14171647324928927 ) ) ;
#46362 = ORIENTED_EDGE ( 'NONE', *, *, #15331, .F. ) ;
#46361 = CARTESIAN_POINT ( 'NONE',  ( -339.1964088526558498, -122.9999999999993747, 59.00000000000002132 ) ) ;
#46363 = CIRCLE ( 'NONE', #39608, 125.0000000000000000 ) ;
#46364 = ORIENTED_EDGE ( 'NONE', *, *, #11119, .F. ) ;
#46365 = LINE ( 'NONE', #19017, #18219 ) ;
#46366 = AXIS2_PLACEMENT_3D ( 'NONE', #49721, #838, #49203 ) ;
#46367 = ADVANCED_FACE ( 'NONE', ( #31204 ), #18612, .T. ) ;
#46368 = LINE ( 'NONE', #10352, #44741 ) ;
#46369 = EDGE_LOOP ( 'NONE', ( #39359, #45086, #31957, #21759 ) ) ;
#46370 = FACE_OUTER_BOUND ( 'NONE', #32287, .T. ) ;
#46371 = ORIENTED_EDGE ( 'NONE', *, *, #42403, .F. ) ;
#46372 = CARTESIAN_POINT ( 'NONE',  ( -339.1964088526558498, -178.4886558749184076, -21.38919645685194837 ) ) ;
#46373 = EDGE_CURVE ( 'NONE', #3759, #37475, #17104, .T. ) ;
#46374 = LINE ( 'NONE', #39497, #49651 ) ;
#46375 = CARTESIAN_POINT ( 'NONE',  ( -339.1964088526558498, -182.1300919119128423, 6.615309698015510165 ) ) ;
#46376 = ORIENTED_EDGE ( 'NONE', *, *, #23677, .T. ) ;
#46377 = AXIS2_PLACEMENT_3D ( 'NONE', #39423, #31281, #43385 ) ;
#46378 = ORIENTED_EDGE ( 'NONE', *, *, #42340, .F. ) ;
#46379 = VECTOR ( 'NONE', #20592, 1000.000000000000000 ) ;
#46380 = ORIENTED_EDGE ( 'NONE', *, *, #18683, .F. ) ;
#46381 = CARTESIAN_POINT ( 'NONE',  ( 73.09196206113300320, -177.1207230881787780, 29.07697310430963356 ) ) ;
#46382 = DIRECTION ( 'NONE',  ( 0.000000000000000000, -1.000000000000000000, 0.000000000000000000 ) ) ;
#46383 = AXIS2_PLACEMENT_3D ( 'NONE', #51203, #19635, #15451 ) ;
#46384 = EDGE_CURVE ( 'NONE', #24976, #39182, #23072, .T. ) ;
#46385 = VECTOR ( 'NONE', #21666, 1000.000000000000000 ) ;
#46386 = DIRECTION ( 'NONE',  ( 0.8757349421956310831, 0.000000000000000000, 0.4827922027307550712 ) ) ;
#46387 = CARTESIAN_POINT ( 'NONE',  ( -339.1964088526558498, -181.6348283828473029, -14.84391218300937432 ) ) ;
#46388 = EDGE_LOOP ( 'NONE', ( #23454, #9833, #12120, #4461 ) ) ;
#46389 = EDGE_CURVE ( 'NONE', #40815, #20971, #6541, .T. ) ;
#46390 = LINE ( 'NONE', #24919, #12250 ) ;
#46391 = ORIENTED_EDGE ( 'NONE', *, *, #37041, .T. ) ;
#46392 = EDGE_LOOP ( 'NONE', ( #46500, #25115, #30537, #41778 ) ) ;
#46393 = DIRECTION ( 'NONE',  ( 0.000000000000000000, 0.8660254037844378194, 0.5000000000000013323 ) ) ;
#46394 = ADVANCED_FACE ( 'NONE', ( #27000 ), #18096, .T. ) ;
#46395 = CARTESIAN_POINT ( 'NONE',  ( -36.09284319799462537, -177.1207230881787780, 124.3848060646152618 ) ) ;
#46396 = AXIS2_PLACEMENT_3D ( 'NONE', #29057, #48547, #12764 ) ;
#46397 = EDGE_CURVE ( 'NONE', #13886, #32088, #10726, .T. ) ;
#46398 = LINE ( 'NONE', #42712, #43022 ) ;
#46399 = DIRECTION ( 'NONE',  ( 0.6528221181905174975, 0.000000000000000000, 0.7575112421616236880 ) ) ;
#46400 = ORIENTED_EDGE ( 'NONE', *, *, #34591, .F. ) ;
#46401 = DIRECTION ( 'NONE',  ( -0.8124868780056825335, 0.000000000000000000, 0.5829794791144703447 ) ) ;
#46402 = AXIS2_PLACEMENT_3D ( 'NONE', #5581, #44734, #8721 ) ;
#46403 = ORIENTED_EDGE ( 'NONE', *, *, #51396, .T. ) ;
#46404 = DIRECTION ( 'NONE',  ( 0.000000000000000000, 0.000000000000000000, 1.000000000000000000 ) ) ;
#46405 = CARTESIAN_POINT ( 'NONE',  ( -339.1964088526558498, -156.6043281241909426, 48.84008046109164525 ) ) ;
#46406 = ORIENTED_EDGE ( 'NONE', *, *, #48032, .T. ) ;
#46407 = CARTESIAN_POINT ( 'NONE',  ( -94.25732089370191602, -183.6283474603465606, 116.3157639405754935 ) ) ;
#46408 = CARTESIAN_POINT ( 'NONE',  ( -66.64622755927952369, -183.6283474603465606, 123.6727797384707372 ) ) ;
#46409 = DIRECTION ( 'NONE',  ( 0.000000000000000000, 0.000000000000000000, 1.000000000000000000 ) ) ;
#46410 = VECTOR ( 'NONE', #34187, 1000.000000000000227 ) ;
#46411 = DIRECTION ( 'NONE',  ( 0.000000000000000000, 0.9927088740980535286, -0.1205366802553268502 ) ) ;
#46412 = VECTOR ( 'NONE', #24134, 1000.000000000000000 ) ;
#46413 = DIRECTION ( 'NONE',  ( -1.000000000000000000, 4.850383327712019318E-15, 9.241633304753524009E-15 ) ) ;
#46414 = ORIENTED_EDGE ( 'NONE', *, *, #11935, .T. ) ;
#46415 = VECTOR ( 'NONE', #23528, 1000.000000000000114 ) ;
#46416 = FACE_OUTER_BOUND ( 'NONE', #37438, .T. ) ;
#46417 = EDGE_LOOP ( 'NONE', ( #5547, #24099, #11845, #39726 ) ) ;
#46418 = EDGE_CURVE ( 'NONE', #28684, #51929, #14945, .T. ) ;
#46419 = EDGE_LOOP ( 'NONE', ( #43248, #29908, #7037, #34497 ) ) ;
#46420 = LINE ( 'NONE', #35351, #6990 ) ;
#46421 = ORIENTED_EDGE ( 'NONE', *, *, #33616, .T. ) ;
#46422 = EDGE_CURVE ( 'NONE', #19489, #6776, #32197, .T. ) ;
#46423 = PLANE ( 'NONE',  #31856 ) ;
#46424 = ORIENTED_EDGE ( 'NONE', *, *, #34955, .F. ) ;
#46425 = DIRECTION ( 'NONE',  ( -0.000000000000000000, 1.000000000000000000, -0.000000000000000000 ) ) ;
#46426 = PLANE ( 'NONE',  #47277 ) ;
#46427 = ORIENTED_EDGE ( 'NONE', *, *, #2238, .T. ) ;
#46428 = DIRECTION ( 'NONE',  ( 1.000000000000000000, -0.000000000000000000, 0.000000000000000000 ) ) ;
#46429 = VECTOR ( 'NONE', #34185, 1000.000000000000000 ) ;
#46430 = EDGE_CURVE ( 'NONE', #24824, #13353, #39080, .T. ) ;
#46431 = CARTESIAN_POINT ( 'NONE',  ( -48.47912675150885065, -177.1207230881787780, 6.938893903907228378E-15 ) ) ;
#46432 = DIRECTION ( 'NONE',  ( 0.000000000000000000, 1.000000000000000000, 0.000000000000000000 ) ) ;
#46433 = ORIENTED_EDGE ( 'NONE', *, *, #27148, .F. ) ;
#46434 = ORIENTED_EDGE ( 'NONE', *, *, #1879, .F. ) ;
#46435 = EDGE_CURVE ( 'NONE', #2077, #51235, #35149, .T. ) ;
#46436 = ADVANCED_FACE ( 'NONE', ( #44069 ), #36177, .F. ) ;
#46437 = VECTOR ( 'NONE', #32379, 1000.000000000000000 ) ;
#46438 = ORIENTED_EDGE ( 'NONE', *, *, #18425, .F. ) ;
#46439 = DIRECTION ( 'NONE',  ( 0.000000000000000000, -0.9927088740980553050, -0.1205366802553130001 ) ) ;
#46440 = DIRECTION ( 'NONE',  ( -0.000000000000000000, 0.000000000000000000, 1.000000000000000000 ) ) ;
#46441 = EDGE_CURVE ( 'NONE', #10769, #8260, #15716, .T. ) ;
#46442 = CARTESIAN_POINT ( 'NONE',  ( -336.3521761649654422, -180.1556192733800117, 16.67542351306693149 ) ) ;
#46443 = FACE_OUTER_BOUND ( 'NONE', #7254, .T. ) ;
#46444 = ORIENTED_EDGE ( 'NONE', *, *, #7143, .F. ) ;
#46445 = AXIS2_PLACEMENT_3D ( 'NONE', #20005, #20133, #20387 ) ;
#46446 = CARTESIAN_POINT ( 'NONE',  ( 72.14504940832446778, -193.5000000000000000, -32.78426643622660208 ) ) ;
#46447 = ORIENTED_EDGE ( 'NONE', *, *, #5328, .F. ) ;
#46449 = VERTEX_POINT ( 'NONE', #11745 ) ;
#46448 = FACE_OUTER_BOUND ( 'NONE', #20190, .T. ) ;
#46450 = VECTOR ( 'NONE', #312, 1000.000000000000000 ) ;
#46451 = ORIENTED_EDGE ( 'NONE', *, *, #6154, .F. ) ;
#46452 = DIRECTION ( 'NONE',  ( 0.000000000000000000, 0.000000000000000000, 1.000000000000000000 ) ) ;
#46453 = VERTEX_POINT ( 'NONE', #4383 ) ;
#46454 = DIRECTION ( 'NONE',  ( -1.000000000000000000, 0.000000000000000000, 0.000000000000000000 ) ) ;
#46455 = EDGE_LOOP ( 'NONE', ( #7436, #41556, #11766, #19108 ) ) ;
#46456 = LINE ( 'NONE', #46207, #289 ) ;
#46457 = AXIS2_PLACEMENT_3D ( 'NONE', #30902, #14357, #14891 ) ;
#46458 = DIRECTION ( 'NONE',  ( -1.000000000000000000, 0.000000000000000000, -0.000000000000000000 ) ) ;
#46459 = VERTEX_POINT ( 'NONE', #48280 ) ;
#46460 = CARTESIAN_POINT ( 'NONE',  ( -128.2395503755045638, -183.6283474603465606, -96.24590808611421267 ) ) ;
#46461 = VERTEX_POINT ( 'NONE', #35662 ) ;
#46462 = EDGE_LOOP ( 'NONE', ( #26031, #23094, #20682, #51535 ) ) ;
#46463 = LINE ( 'NONE', #41987, #44698 ) ;
#46464 = CARTESIAN_POINT ( 'NONE',  ( -19.18792875895802652, -193.5000000000000000, -120.4907712303050715 ) ) ;
#46465 = DIRECTION ( 'NONE',  ( 0.000000000000000000, -0.000000000000000000, 1.000000000000000000 ) ) ;
#46466 = ORIENTED_EDGE ( 'NONE', *, *, #51362, .T. ) ;
#46467 = LINE ( 'NONE', #49386, #24843 ) ;
#46468 = AXIS2_PLACEMENT_3D ( 'NONE', #10977, #43039, #7045 ) ;
#46469 = CARTESIAN_POINT ( 'NONE',  ( -336.3521761649654422, -170.5607375887735770, 35.68215131113770155 ) ) ;
#46470 = DIRECTION ( 'NONE',  ( -0.000000000000000000, 1.000000000000000000, -0.000000000000000000 ) ) ;
#46471 = CARTESIAN_POINT ( 'NONE',  ( 0.7476021451244393434, -193.5000000000000000, -113.8100815915415751 ) ) ;
#46472 = ORIENTED_EDGE ( 'NONE', *, *, #12784, .T. ) ;
#46473 = CARTESIAN_POINT ( 'NONE',  ( -47.82630463331832971, -183.6283474603465606, -0.7575112421616121416 ) ) ;
#46474 = CARTESIAN_POINT ( 'NONE',  ( -332.3517673607765914, -88.08538291676191534, 48.43351006119235080 ) ) ;
#46475 = AXIS2_PLACEMENT_3D ( 'NONE', #38824, #19380, #39345 ) ;
#46476 = CARTESIAN_POINT ( 'NONE',  ( 48.66843973345087448, 30.00000000000000355, -40.95752564483601788 ) ) ;
#46477 = ORIENTED_EDGE ( 'NONE', *, *, #39433, .T. ) ;
#46478 = DIRECTION ( 'NONE',  ( -1.000000000000000000, 6.921107616850682476E-15, -7.812315528781957664E-15 ) ) ;
#46479 = EDGE_CURVE ( 'NONE', #35187, #25387, #28295, .T. ) ;
#46480 = DIRECTION ( 'NONE',  ( 0.000000000000000000, 0.000000000000000000, 1.000000000000000000 ) ) ;
#46481 = EDGE_CURVE ( 'NONE', #33745, #41107, #35931, .T. ) ;
#46482 = VERTEX_POINT ( 'NONE', #43805 ) ;
#46483 = EDGE_CURVE ( 'NONE', #42583, #10747, #35399, .T. ) ;
#46484 = FACE_OUTER_BOUND ( 'NONE', #23533, .T. ) ;
#46485 = VERTEX_POINT ( 'NONE', #39850 ) ;
#46486 = APPLICATION_CONTEXT ( 'automotive_design' ) ;
#46487 = CARTESIAN_POINT ( 'NONE',  ( -48.59739992243020623, -193.5000000000000000, -0.9929810960135115883 ) ) ;
#46488 = CYLINDRICAL_SURFACE ( 'NONE', #38760, 4.000000000000003553 ) ;
#46489 = LINE ( 'NONE', #34895, #1909 ) ;
#46490 = EDGE_CURVE ( 'NONE', #44016, #40473, #27522, .T. ) ;
#46491 = LINE ( 'NONE', #46244, #11518 ) ;
#46492 = EDGE_CURVE ( 'NONE', #13810, #18089, #15453, .T. ) ;
#46493 = CARTESIAN_POINT ( 'NONE',  ( -19.28375372365792728, -193.5000000000000000, 121.5427093402341541 ) ) ;
#46494 = ORIENTED_EDGE ( 'NONE', *, *, #22051, .F. ) ;
#46495 = EDGE_CURVE ( 'NONE', #45117, #33386, #23339, .T. ) ;
#46496 = CARTESIAN_POINT ( 'NONE',  ( -339.1964088526558498, -123.5000000000000284, 0.000000000000000000 ) ) ;
#46497 = ORIENTED_EDGE ( 'NONE', *, *, #49090, .T. ) ;
#46498 = DIRECTION ( 'NONE',  ( 0.000000000000000000, 0.000000000000000000, 1.000000000000000000 ) ) ;
#46499 = EDGE_CURVE ( 'NONE', #26309, #35813, #4142, .T. ) ;
#46500 = ORIENTED_EDGE ( 'NONE', *, *, #43380, .F. ) ;
#46501 = CARTESIAN_POINT ( 'NONE',  ( 12.54192669111252378, -193.5000000000000000, 107.9473519284347276 ) ) ;
#46502 = CIRCLE ( 'NONE', #7882, 60.00000000000000000 ) ;
#46503 = EDGE_CURVE ( 'NONE', #43725, #23668, #12000, .T. ) ;
#46504 = VECTOR ( 'NONE', #39644, 1000.000000000000000 ) ;
#46505 = AXIS2_PLACEMENT_3D ( 'NONE', #23834, #47767, #23574 ) ;
#46506 = DIRECTION ( 'NONE',  ( -0.000000000000000000, 0.9927088740980538617, -0.1205366802553232974 ) ) ;
#46507 = CARTESIAN_POINT ( 'NONE',  ( 76.52053249983504202, -193.5000000000000000, -0.2918682030015403162 ) ) ;
#46508 = VERTEX_POINT ( 'NONE', #47507 ) ;
#46511 = ORIENTED_EDGE ( 'NONE', *, *, #42988, .F. ) ;
#46510 = CARTESIAN_POINT ( 'NONE',  ( -339.1964088526558498, -143.9541802141672235, -55.34326076196065003 ) ) ;
#46509 = LINE ( 'NONE', #43331, #47686 ) ;
#46512 = FACE_OUTER_BOUND ( 'NONE', #1985, .T. ) ;
#46513 = ORIENTED_EDGE ( 'NONE', *, *, #40353, .T. ) ;
#46514 = DIRECTION ( 'NONE',  ( 0.000000000000000000, 1.000000000000000000, 0.000000000000000000 ) ) ;
#46515 = VERTEX_POINT ( 'NONE', #12530 ) ;
#46516 = LINE ( 'NONE', #50468, #3227 ) ;
#46519 = VERTEX_POINT ( 'NONE', #28028 ) ;
#46518 = CARTESIAN_POINT ( 'NONE',  ( -158.9435005891548087, -177.1207230881787780, -56.33604425924758630 ) ) ;
#46517 = DIRECTION ( 'NONE',  ( 0.000000000000000000, 0.000000000000000000, 1.000000000000000000 ) ) ;
#46520 = AXIS2_PLACEMENT_3D ( 'NONE', #6508, #30390, #2021 ) ;
#46521 = EDGE_CURVE ( 'NONE', #28174, #51399, #40124, .T. ) ;
#46522 = VERTEX_POINT ( 'NONE', #20155 ) ;
#46523 = DIRECTION ( 'NONE',  ( -0.000000000000000000, 0.6631226582408039638, 0.7485107481710934207 ) ) ;
#46524 = ORIENTED_EDGE ( 'NONE', *, *, #1927, .F. ) ;
#46525 = DIRECTION ( 'NONE',  ( 0.9027978299657446470, 0.000000000000000000, -0.4300652022765183435 ) ) ;
#46526 = LINE ( 'NONE', #38626, #9732 ) ;
#46527 = ORIENTED_EDGE ( 'NONE', *, *, #42745, .F. ) ;
#46528 = PLANE ( 'NONE',  #28024 ) ;
#46529 = CARTESIAN_POINT ( 'NONE',  ( -124.9871112439422092, -189.7472609257535510, -98.85104101073277150 ) ) ;
#46530 = DIRECTION ( 'NONE',  ( 0.000000000000000000, -0.000000000000000000, 1.000000000000000000 ) ) ;
#46531 = DIRECTION ( 'NONE',  ( -1.000000000000000000, 0.000000000000000000, 0.000000000000000000 ) ) ;
#46532 = CARTESIAN_POINT ( 'NONE',  ( -305.0000000000000568, -181.6348283828471608, 14.84391218300993209 ) ) ;
#46533 = ORIENTED_EDGE ( 'NONE', *, *, #45124, .T. ) ;
#46534 =( NAMED_UNIT ( * ) SI_UNIT ( $, .STERADIAN. ) SOLID_ANGLE_UNIT ( ) );
#46535 = DIRECTION ( 'NONE',  ( 0.4677363560876406923, 0.000000000000000000, 0.8838680338115276758 ) ) ;
#46536 = FACE_OUTER_BOUND ( 'NONE', #40086, .T. ) ;
#46537 = EDGE_CURVE ( 'NONE', #3688, #13519, #39591, .T. ) ;
#46538 = DIRECTION ( 'NONE',  ( 0.000000000000000000, 0.000000000000000000, -1.000000000000000000 ) ) ;
#46539 = ORIENTED_EDGE ( 'NONE', *, *, #29149, .T. ) ;
#46540 = DIRECTION ( 'NONE',  ( 0.6528221181905280446, 0.000000000000000000, -0.7575112421616145841 ) ) ;
#46541 = DIRECTION ( 'NONE',  ( -0.000000000000000000, 0.8229838658936494689, -0.5680647467311658039 ) ) ;
#46542 = VECTOR ( 'NONE', #10565, 1000.000000000000000 ) ;
#46543 = VECTOR ( 'NONE', #43858, 1000.000000000000000 ) ;
#46544 = EDGE_CURVE ( 'NONE', #14073, #15388, #51711, .T. ) ;
#46545 = PLANE ( 'NONE',  #2544 ) ;
#46546 = EDGE_CURVE ( 'NONE', #51547, #13772, #3606, .T. ) ;
#46547 = DIRECTION ( 'NONE',  ( 0.8896570909947499883, 0.000000000000000000, -0.4566292373937077542 ) ) ;
#46548 = EDGE_CURVE ( 'NONE', #36281, #29476, #50702, .T. ) ;
#46549 = EDGE_CURVE ( 'NONE', #4051, #1404, #16297, .T. ) ;
#46550 = VECTOR ( 'NONE', #111, 1000.000000000000000 ) ;
#46551 = ADVANCED_FACE ( 'NONE', ( #19383 ), #3874, .F. ) ;
#46552 = ADVANCED_FACE ( 'NONE', ( #25146 ), #45129, .T. ) ;
#46553 = DIRECTION ( 'NONE',  ( -0.9890401873221623674, 0.000000000000000000, -0.1476465640024917925 ) ) ;
#46554 = DIRECTION ( 'NONE',  ( -5.399917434947259359E-17, -1.000000000000000000, 0.000000000000000000 ) ) ;
#46555 = DIRECTION ( 'NONE',  ( 0.000000000000000000, 1.000000000000000000, 0.000000000000000000 ) ) ;
#46556 = VERTEX_POINT ( 'NONE', #36965 ) ;
#46557 = ADVANCED_FACE ( 'NONE', ( #955 ), #33014, .T. ) ;
#46558 = AXIS2_PLACEMENT_3D ( 'NONE', #24848, #40869, #36939 ) ;
#46559 = CARTESIAN_POINT ( 'NONE',  ( 42.96730897722186171, 30.00000000000000355, -41.16782622478179832 ) ) ;
#46560 = EDGE_CURVE ( 'NONE', #15815, #30216, #20945, .T. ) ;
#46561 = FACE_OUTER_BOUND ( 'NONE', #26027, .T. ) ;
#46562 = EDGE_LOOP ( 'NONE', ( #13873, #52031, #25544, #37830 ) ) ;
#46563 = ORIENTED_EDGE ( 'NONE', *, *, #8285, .F. ) ;
#46564 = EDGE_CURVE ( 'NONE', #44736, #35501, #710, .T. ) ;
#46565 = ORIENTED_EDGE ( 'NONE', *, *, #11504, .F. ) ;
#46566 = LINE ( 'NONE', #10549, #29235 ) ;
#46567 = EDGE_CURVE ( 'NONE', #6623, #4319, #46502, .T. ) ;
#46568 = DIRECTION ( 'NONE',  ( 0.000000000000000000, 0.000000000000000000, -1.000000000000000000 ) ) ;
#46569 = LINE ( 'NONE', #10553, #2843 ) ;
#46570 = ORIENTED_EDGE ( 'NONE', *, *, #47198, .F. ) ;
#46571 = EDGE_CURVE ( 'NONE', #27996, #37301, #20673, .T. ) ;
#46572 = PLANE ( 'NONE',  #4901 ) ;
#46573 = CARTESIAN_POINT ( 'NONE',  ( -56.05401443572774411, -175.3837268820161057, 124.7702732086913073 ) ) ;
#46576 = ORIENTED_EDGE ( 'NONE', *, *, #2036, .F. ) ;
#46575 = PLANE ( 'NONE',  #6492 ) ;
#46574 = DIRECTION ( 'NONE',  ( 0.000000000000000000, 0.000000000000000000, 1.000000000000000000 ) ) ;
#46577 = VECTOR ( 'NONE', #29383, 999.9999999999998863 ) ;
#46578 = LINE ( 'NONE', #14001, #4605 ) ;
#46579 = VECTOR ( 'NONE', #30531, 1000.000000000000000 ) ;
#46580 = ORIENTED_EDGE ( 'NONE', *, *, #30880, .F. ) ;
#46581 = CARTESIAN_POINT ( 'NONE',  ( -336.3521761649654422, -123.5000000000000284, 0.000000000000000000 ) ) ;
#46582 = ORIENTED_EDGE ( 'NONE', *, *, #17856, .F. ) ;
#46583 = VECTOR ( 'NONE', #12131, 1000.000000000000227 ) ;
#46584 = CARTESIAN_POINT ( 'NONE',  ( -48.47912675150885065, -177.1207230881787780, 6.938893903907228378E-15 ) ) ;
#46585 = LINE ( 'NONE', #42882, #26324 ) ;
#46586 = DIRECTION ( 'NONE',  ( 0.000000000000000000, 0.000000000000000000, -1.000000000000000000 ) ) ;
#46587 = EDGE_CURVE ( 'NONE', #2175, #11425, #36423, .T. ) ;
#46588 = EDGE_LOOP ( 'NONE', ( #3191, #50788, #31634, #16906 ) ) ;
#46589 = LINE ( 'NONE', #46334, #25627 ) ;
#46590 = FACE_OUTER_BOUND ( 'NONE', #8468, .T. ) ;
#46591 = VERTEX_POINT ( 'NONE', #17004 ) ;
#46592 = VECTOR ( 'NONE', #24393, 1000.000000000000000 ) ;
#46593 = CARTESIAN_POINT ( 'NONE',  ( 0.000000000000000000, 65.00000000000000000, 0.000000000000000000 ) ) ;
#46594 = AXIS2_PLACEMENT_3D ( 'NONE', #22766, #46953, #6994 ) ;
#46595 = DIRECTION ( 'NONE',  ( -0.000000000000000000, -0.9350162426854121689, 0.3546048870425426158 ) ) ;
#46596 = VERTEX_POINT ( 'NONE', #33280 ) ;
#46597 = CARTESIAN_POINT ( 'NONE',  ( -114.9600645115007040, -177.1207230881787780, 105.8550183720738573 ) ) ;
#46598 = CIRCLE ( 'NONE', #49930, 4.000000000000003553 ) ;
#46599 = DIRECTION ( 'NONE',  ( 5.399917434947259359E-17, 1.000000000000000000, -0.000000000000000000 ) ) ;
#46600 = ORIENTED_EDGE ( 'NONE', *, *, #5117, .F. ) ;
#46601 = DIRECTION ( 'NONE',  ( -0.9266896074318291543, 0.000000000000000000, -0.3758275821142488260 ) ) ;
#46602 = EDGE_LOOP ( 'NONE', ( #25086, #20864, #8448, #50079 ) ) ;
#46603 = LINE ( 'NONE', #39222, #17241 ) ;
#46604 = DIRECTION ( 'NONE',  ( 0.9890401873221654760, 0.000000000000000000, -0.1476465640024710868 ) ) ;
#46605 = ORIENTED_EDGE ( 'NONE', *, *, #23689, .F. ) ;
#46606 = EDGE_CURVE ( 'NONE', #25483, #13304, #39793, .T. ) ;
#46607 = CARTESIAN_POINT ( 'NONE',  ( -330.4913330509368166, -95.63860483659048839, 52.00954392751722111 ) ) ;
#46608 = LINE ( 'NONE', #6913, #1211 ) ;
#46609 = DIRECTION ( 'NONE',  ( -0.000000000000000000, 1.000000000000000000, -0.000000000000000000 ) ) ;
#46610 = ADVANCED_FACE ( 'NONE', ( #13313 ), #44851, .F. ) ;
#46611 = ORIENTED_EDGE ( 'NONE', *, *, #23924, .F. ) ;
#46612 = CARTESIAN_POINT ( 'NONE',  ( -332.3517673607765914, -118.0087234915157381, -58.76657425099333665 ) ) ;
#46613 = EDGE_CURVE ( 'NONE', #24955, #17439, #41457, .T. ) ;
#46614 = EDGE_LOOP ( 'NONE', ( #36016, #34903, #15171, #8371 ) ) ;
#46615 = VECTOR ( 'NONE', #5307, 1000.000000000000000 ) ;
#46616 = DIRECTION ( 'NONE',  ( -0.000000000000000000, -0.3546048870425396182, -0.9350162426854132791 ) ) ;
#46617 = LINE ( 'NONE', #26371, #36069 ) ;
#46619 = ORIENTED_EDGE ( 'NONE', *, *, #21697, .T. ) ;
#46618 = CARTESIAN_POINT ( 'NONE',  ( -63.09433862318517328, -175.3837268820161057, -124.1426420773539405 ) ) ;
#46620 = AXIS2_PLACEMENT_3D ( 'NONE', #7592, #36219, #28064 ) ;
#46621 = VECTOR ( 'NONE', #30552, 1000.000000000000000 ) ;
#46622 = ORIENTED_EDGE ( 'NONE', *, *, #6736, .F. ) ;
#46623 = DIRECTION ( 'NONE',  ( -1.000000000000000000, -0.000000000000000000, 0.000000000000000000 ) ) ;
#46624 = VECTOR ( 'NONE', #4392, 1000.000000000000000 ) ;
#46625 = LINE ( 'NONE', #30317, #38878 ) ;
#46626 = ORIENTED_EDGE ( 'NONE', *, *, #43645, .F. ) ;
#46627 = CARTESIAN_POINT ( 'NONE',  ( 0.000000000000000000, -175.7419055135392227, 27.41866715058277038 ) ) ;
#46629 = EDGE_CURVE ( 'NONE', #42654, #26038, #39754, .T. ) ;
#46628 = VECTOR ( 'NONE', #10953, 1000.000000000000000 ) ;
#46630 = ORIENTED_EDGE ( 'NONE', *, *, #22506, .T. ) ;
#46631 = CARTESIAN_POINT ( 'NONE',  ( -40.90423906728908321, -175.3837268820161057, -124.7702732086912363 ) ) ;
#46632 = CARTESIAN_POINT ( 'NONE',  ( -101.0675409952199999, -193.5000000000000000, 113.3995532942341100 ) ) ;
#46633 = AXIS2_PLACEMENT_3D ( 'NONE', #17862, #18119, #26246 ) ;
#46635 = VECTOR ( 'NONE', #46265, 1000.000000000000000 ) ;
#46634 = DIRECTION ( 'NONE',  ( 0.2920567706369694982, 0.000000000000000000, 0.9564009842765243130 ) ) ;
#46636 = CARTESIAN_POINT ( 'NONE',  ( -99.62791064391784346, -189.7472609257535510, -114.0561348912352173 ) ) ;
#46637 = ORIENTED_EDGE ( 'NONE', *, *, #3190, .F. ) ;
#46638 = EDGE_LOOP ( 'NONE', ( #19337, #14894 ) ) ;
#46639 = ADVANCED_FACE ( 'NONE', ( #3772 ), #12682, .T. ) ;
#46640 = ORIENTED_EDGE ( 'NONE', *, *, #29236, .F. ) ;
#46641 = CIRCLE ( 'NONE', #14752, 124.9999999999999858 ) ;
#46642 = DIRECTION ( 'NONE',  ( 0.000000000000000000, 0.000000000000000000, -1.000000000000000000 ) ) ;
#46643 = DIRECTION ( 'NONE',  ( 1.000000000000000000, 0.000000000000000000, 0.000000000000000000 ) ) ;
#46644 = CARTESIAN_POINT ( 'NONE',  ( -30.00000000000000000, -43.50000000000000000, 0.000000000000000000 ) ) ;
#46645 = CARTESIAN_POINT ( 'NONE',  ( -136.1415351158078693, -193.5000000000000000, -89.10837311819173578 ) ) ;
#46646 = EDGE_LOOP ( 'NONE', ( #506, #20756, #45702, #26589 ) ) ;
#46647 = DIRECTION ( 'NONE',  ( 0.000000000000000000, 1.000000000000000000, 0.000000000000000000 ) ) ;
#46648 = DIRECTION ( 'NONE',  ( -1.000000000000000000, 0.000000000000000000, 0.000000000000000000 ) ) ;
#46649 = EDGE_LOOP ( 'NONE', ( #965, #47672, #42735, #27147 ) ) ;
#46650 = VERTEX_POINT ( 'NONE', #607 ) ;
#46651 = VECTOR ( 'NONE', #35723, 1000.000000000000000 ) ;
#46652 = CARTESIAN_POINT ( 'NONE',  ( 72.31641062551800303, -189.7472609257535510, 32.14713283941990341 ) ) ;
#46653 = VECTOR ( 'NONE', #23191, 1000.000000000000000 ) ;
#46654 = CIRCLE ( 'NONE', #36539, 125.0000000000000000 ) ;
#46655 = DIRECTION ( 'NONE',  ( 0.9473263538541899509, 0.000000000000000000, 0.3202698538628415692 ) ) ;
#46656 = DIRECTION ( 'NONE',  ( 0.000000000000000000, -0.000000000000000000, 1.000000000000000000 ) ) ;
#46657 = EDGE_LOOP ( 'NONE', ( #22898, #41003, #20966, #50560 ) ) ;
#46658 = CARTESIAN_POINT ( 'NONE',  ( -47.97059563285962724, -177.1207230881787780, -0.8610436117673480050 ) ) ;
#46659 = ORIENTED_EDGE ( 'NONE', *, *, #42330, .F. ) ;
#46660 = FACE_OUTER_BOUND ( 'NONE', #28484, .T. ) ;
#46661 = VECTOR ( 'NONE', #48915, 1000.000000000000000 ) ;
#46662 = LINE ( 'NONE', #5698, #988 ) ;
#46663 = ORIENTED_EDGE ( 'NONE', *, *, #18815, .F. ) ;
#46664 = FACE_OUTER_BOUND ( 'NONE', #2292, .T. ) ;
#46665 = LINE ( 'NONE', #42449, #345 ) ;
#46666 = DIRECTION ( 'NONE',  ( -0.000000000000000000, 1.000000000000000000, -0.000000000000000000 ) ) ;
#46667 = ADVANCED_FACE ( 'NONE', ( #48455 ), #3511, .F. ) ;
#46668 = CIRCLE ( 'NONE', #45806, 125.0000000000000000 ) ;
#46669 = CARTESIAN_POINT ( 'NONE',  ( -238.7407812814481076, -213.5000000000000000, -9.999999999999987566 ) ) ;
#46671 = VECTOR ( 'NONE', #19328, 1000.000000000000000 ) ;
#46670 = DIRECTION ( 'NONE',  ( -1.000000000000000000, 0.000000000000000000, 0.000000000000000000 ) ) ;
#46672 = ORIENTED_EDGE ( 'NONE', *, *, #19191, .T. ) ;
#46673 = DIRECTION ( 'NONE',  ( -0.000000000000000000, 1.000000000000000000, -0.000000000000000000 ) ) ;
#46674 = ORIENTED_EDGE ( 'NONE', *, *, #2583, .T. ) ;
#46675 = VERTEX_POINT ( 'NONE', #12160 ) ;
#46676 = DIRECTION ( 'NONE',  ( -0.4566292373937200777, 0.000000000000000000, 0.8896570909947436601 ) ) ;
#46677 = ORIENTED_EDGE ( 'NONE', *, *, #12317, .T. ) ;
#46678 = LINE ( 'NONE', #38772, #20951 ) ;
#46679 = VECTOR ( 'NONE', #3354, 1000.000000000000000 ) ;
#46680 = VECTOR ( 'NONE', #36171, 1000.000000000000000 ) ;
#46681 = ORIENTED_EDGE ( 'NONE', *, *, #49713, .T. ) ;
#46682 = FACE_OUTER_BOUND ( 'NONE', #41200, .T. ) ;
#46683 = CARTESIAN_POINT ( 'NONE',  ( -336.3521761649654422, -81.08339623743702873, -41.09453333279329712 ) ) ;
#46684 = ADVANCED_FACE ( 'NONE', ( #43972 ), #23747, .T. ) ;
#46685 = ORIENTED_EDGE ( 'NONE', *, *, #23100, .F. ) ;
#46686 = DIRECTION ( 'NONE',  ( 0.000000000000000000, -0.000000000000000000, 1.000000000000000000 ) ) ;
#46687 = AXIS2_PLACEMENT_3D ( 'NONE', #50997, #30482, #14994 ) ;
#46688 = AXIS2_PLACEMENT_3D ( 'NONE', #32350, #11858, #7917 ) ;
#46689 = DIRECTION ( 'NONE',  ( 0.000000000000000000, 0.9927088740980534176, -0.1205366802553268502 ) ) ;
#46690 = DIRECTION ( 'NONE',  ( 0.000000000000000000, 0.000000000000000000, 1.000000000000000000 ) ) ;
#46691 = ORIENTED_EDGE ( 'NONE', *, *, #7912, .F. ) ;
#46692 = VERTEX_POINT ( 'NONE', #36347 ) ;
#46693 = ORIENTED_EDGE ( 'NONE', *, *, #24061, .T. ) ;
#46694 = DIRECTION ( 'NONE',  ( 0.000000000000000000, 6.846375318521798245E-14, 1.000000000000000000 ) ) ;
#46695 = CARTESIAN_POINT ( 'NONE',  ( -171.4559849729830603, -193.5000000000000000, 22.39848972532369942 ) ) ;
#46696 = VECTOR ( 'NONE', #24798, 1000.000000000000000 ) ;
#46697 = AXIS2_PLACEMENT_3D ( 'NONE', #1339, #25779, #33911 ) ;
#46698 = CARTESIAN_POINT ( 'NONE',  ( -103.4012653778457462, -193.5000000000000000, -112.2878385610366649 ) ) ;
#46699 = VECTOR ( 'NONE', #8909, 1000.000000000000000 ) ;
#46701 = VECTOR ( 'NONE', #38572, 1000.000000000000000 ) ;
#46700 = LINE ( 'NONE', #43255, #33729 ) ;
#46702 = CARTESIAN_POINT ( 'NONE',  ( -30.31202594373734627, -177.1207230881787780, -123.6727797384705809 ) ) ;
#46703 = ORIENTED_EDGE ( 'NONE', *, *, #34041, .T. ) ;
#46704 = ADVANCED_FACE ( 'NONE', ( #44762 ), #12433, .F. ) ;
#46705 = AXIS2_PLACEMENT_3D ( 'NONE', #42298, #30479, #2100 ) ;
#46706 = VECTOR ( 'NONE', #36093, 1000.000000000000000 ) ;
#46707 = CARTESIAN_POINT ( 'NONE',  ( -48.47912675150885065, -189.7472609257535510, 6.938893903907228378E-15 ) ) ;
#46708 = ORIENTED_EDGE ( 'NONE', *, *, #14336, .F. ) ;
#46710 = VERTEX_POINT ( 'NONE', #20062 ) ;
#46709 = CARTESIAN_POINT ( 'NONE',  ( -48.47912675150885065, -177.1207230881787780, 6.938893903907228378E-15 ) ) ;
#46711 = ORIENTED_EDGE ( 'NONE', *, *, #39173, .F. ) ;
#46712 = FACE_OUTER_BOUND ( 'NONE', #44873, .T. ) ;
#46713 = ORIENTED_EDGE ( 'NONE', *, *, #21870, .F. ) ;
#46714 = CYLINDRICAL_SURFACE ( 'NONE', #21277, 125.0000000000000000 ) ;
#46715 = DIRECTION ( 'NONE',  ( -1.000000000000000000, 0.000000000000000000, 0.000000000000000000 ) ) ;
#46716 = ORIENTED_EDGE ( 'NONE', *, *, #7285, .T. ) ;
#46717 = LINE ( 'NONE', #35135, #20832 ) ;
#46718 = ORIENTED_EDGE ( 'NONE', *, *, #31716, .T. ) ;
#46719 = EDGE_CURVE ( 'NONE', #25876, #30123, #28454, .T. ) ;
#46720 = ORIENTED_EDGE ( 'NONE', *, *, #6, .F. ) ;
#46721 = DIRECTION ( 'NONE',  ( 0.6528221181905174975, 0.000000000000000000, 0.7575112421616236880 ) ) ;
#46722 = CIRCLE ( 'NONE', #43381, 125.0000000000000000 ) ;
#46723 = DIRECTION ( 'NONE',  ( 0.000000000000000000, 0.000000000000000000, -1.000000000000000000 ) ) ;
#46724 = VECTOR ( 'NONE', #34504, 1000.000000000000000 ) ;
#46725 = DIRECTION ( 'NONE',  ( 0.000000000000000000, -0.000000000000000000, -1.000000000000000000 ) ) ;
#46726 = DIRECTION ( 'NONE',  ( -0.000000000000000000, 1.000000000000000000, -0.000000000000000000 ) ) ;
#46727 = VERTEX_POINT ( 'NONE', #15615 ) ;
#46728 = DIRECTION ( 'NONE',  ( -0.9995608365087940150, 0.000000000000000000, -0.02963332782257007206 ) ) ;
#46729 = PLANE ( 'NONE',  #44050 ) ;
#46730 = VECTOR ( 'NONE', #31258, 1000.000000000000000 ) ;
#46731 = DIRECTION ( 'NONE',  ( 0.000000000000000000, 0.000000000000000000, 1.000000000000000000 ) ) ;
#46732 = DIRECTION ( 'NONE',  ( 0.5586467658036476935, 0.000000000000000000, 0.8294056854502049880 ) ) ;
#46733 = EDGE_CURVE ( 'NONE', #11828, #10147, #44501, .T. ) ;
#46734 = ORIENTED_EDGE ( 'NONE', *, *, #24780, .T. ) ;
#46735 = DIRECTION ( 'NONE',  ( 0.000000000000000000, -0.9350162426854107256, 0.3546048870425463906 ) ) ;
#46736 = DIRECTION ( 'NONE',  ( -0.000000000000000000, 1.000000000000000000, -0.000000000000000000 ) ) ;
#46737 = ADVANCED_FACE ( 'NONE', ( #19543 ), #24517, .F. ) ;
#46738 = DIRECTION ( 'NONE',  ( 0.8470055835512242393, 0.000000000000000000, 0.5315839928299667116 ) ) ;
#46739 = ORIENTED_EDGE ( 'NONE', *, *, #32988, .F. ) ;
#46740 = CIRCLE ( 'NONE', #15678, 125.0000000000000000 ) ;
#46741 = EDGE_CURVE ( 'NONE', #24085, #13319, #20579, .T. ) ;
#46742 = AXIS2_PLACEMENT_3D ( 'NONE', #50229, #15244, #22349 ) ;
#46743 = LINE ( 'NONE', #10982, #34813 ) ;
#46744 = AXIS2_PLACEMENT_3D ( 'NONE', #29497, #1906, #29756 ) ;
#46745 = VECTOR ( 'NONE', #10331, 1000.000000000000000 ) ;
#46746 = DIRECTION ( 'NONE',  ( 0.8455960035018199594, 0.000000000000000000, 0.5338233779648003940 ) ) ;
#46747 = ORIENTED_EDGE ( 'NONE', *, *, #34656, .T. ) ;
#46748 = CARTESIAN_POINT ( 'NONE',  ( -339.1964088526558498, -65.36517161715264024, 14.84391218300897108 ) ) ;
#46749 = AXIS2_PLACEMENT_3D ( 'NONE', #14313, #45858, #50324 ) ;
#46750 = ORIENTED_EDGE ( 'NONE', *, *, #18120, .T. ) ;
#46751 = DIRECTION ( 'NONE',  ( -0.000000000000000000, 0.8854560256532043594, -0.4647231720437789981 ) ) ;
#46752 = CARTESIAN_POINT ( 'NONE',  ( -26.20043062753591201, -189.7472609257535510, -122.9986166548862911 ) ) ;
#46753 = PLANE ( 'NONE',  #49753 ) ;
#46754 = EDGE_CURVE ( 'NONE', #50412, #19338, #32669, .T. ) ;
#46755 = FACE_OUTER_BOUND ( 'NONE', #41343, .T. ) ;
#46756 = LINE ( 'NONE', #43824, #27718 ) ;
#46757 = ORIENTED_EDGE ( 'NONE', *, *, #49119, .T. ) ;
#46758 = PLANE ( 'NONE',  #39062 ) ;
#46759 = VERTEX_POINT ( 'NONE', #27688 ) ;
#46760 = CARTESIAN_POINT ( 'NONE',  ( 38.48673058372651923, -193.5000000000000000, 88.39086586114802913 ) ) ;
#46761 = AXIS2_PLACEMENT_3D ( 'NONE', #20030, #40506, #12397 ) ;
#46762 = ORIENTED_EDGE ( 'NONE', *, *, #38670, .T. ) ;
#46763 = CARTESIAN_POINT ( 'NONE',  ( -49.17567778057184569, -193.5000000000000000, -0.7175072570443327136 ) ) ;
#46764 = CIRCLE ( 'NONE', #29947, 125.0000000000000000 ) ;
#46765 = DIRECTION ( 'NONE',  ( 0.000000000000000000, 0.000000000000000000, 1.000000000000000000 ) ) ;
#46766 = FACE_OUTER_BOUND ( 'NONE', #45650, .T. ) ;
#46767 = ORIENTED_EDGE ( 'NONE', *, *, #25418, .F. ) ;
#46770 = EDGE_LOOP ( 'NONE', ( #34389, #35893, #35329, #2774 ) ) ;
#46769 = DIRECTION ( 'NONE',  ( -0.000000000000000000, 1.000000000000000000, -0.000000000000000000 ) ) ;
#46768 = CARTESIAN_POINT ( 'NONE',  ( -330.4913330509368166, -96.52406086224361559, 52.47426709956096147 ) ) ;
#46771 = VECTOR ( 'NONE', #22197, 1000.000000000000114 ) ;
#46772 = AXIS2_PLACEMENT_3D ( 'NONE', #12677, #28700, #45029 ) ;
#46773 = AXIS2_PLACEMENT_3D ( 'NONE', #10181, #17815, #38562 ) ;
#46774 = CARTESIAN_POINT ( 'NONE',  ( -161.4184887245413904, -183.6283474603465606, 51.19472891551358629 ) ) ;
#46775 = ORIENTED_EDGE ( 'NONE', *, *, #10868, .F. ) ;
#46776 = DIRECTION ( 'NONE',  ( 0.000000000000000000, 1.000000000000000000, 0.000000000000000000 ) ) ;
#46777 = VERTEX_POINT ( 'NONE', #16130 ) ;
#46778 = EDGE_CURVE ( 'NONE', #39629, #24186, #32146, .T. ) ;
#46779 = ADVANCED_FACE ( 'NONE', ( #48190 ), #28194, .T. ) ;
#46780 = AXIS2_PLACEMENT_3D ( 'NONE', #28181, #44230, #12931 ) ;
#46781 = DIRECTION ( 'NONE',  ( -0.000000000000000000, -1.000000000000000000, 0.000000000000000000 ) ) ;
#46784 = EDGE_LOOP ( 'NONE', ( #41396, #6189, #39711, #25611 ) ) ;
#46783 = CARTESIAN_POINT ( 'NONE',  ( -48.47912675150885065, -183.6283474603465606, 6.938893903907228378E-15 ) ) ;
#46782 = DIRECTION ( 'NONE',  ( -8.718379230999705894E-17, -0.9350162426854181641, -0.3546048870425267951 ) ) ;
#46785 = ORIENTED_EDGE ( 'NONE', *, *, #25356, .F. ) ;
#46786 = CIRCLE ( 'NONE', #30007, 125.0000000000000000 ) ;
#46787 = CYLINDRICAL_SURFACE ( 'NONE', #47530, 15.00000000000000000 ) ;
#46788 = ORIENTED_EDGE ( 'NONE', *, *, #19086, .F. ) ;
#46789 = DIRECTION ( 'NONE',  ( -0.000000000000000000, 0.000000000000000000, -1.000000000000000000 ) ) ;
#46790 = CARTESIAN_POINT ( 'NONE',  ( -92.78132261338706144, -175.3837268820161057, -116.8859077982276631 ) ) ;
#46791 = ORIENTED_EDGE ( 'NONE', *, *, #39121, .F. ) ;
#46792 = CARTESIAN_POINT ( 'NONE',  ( -339.1964088526558498, -90.39567187580880159, -48.84008046109142498 ) ) ;
#46793 = CARTESIAN_POINT ( 'NONE',  ( -48.47912675150885065, -175.3837268820161057, 6.938893903907228378E-15 ) ) ;
#46794 = CARTESIAN_POINT ( 'NONE',  ( 45.36094686508022988, -193.5000000000000000, -82.57748230379237953 ) ) ;
#46795 = PLANE ( 'NONE',  #6681 ) ;
#46796 = PLANE ( 'NONE',  #29911 ) ;
#46797 = VERTEX_POINT ( 'NONE', #51885 ) ;
#46798 = EDGE_CURVE ( 'NONE', #16397, #23451, #7722, .T. ) ;
#46799 = LINE ( 'NONE', #10788, #2785 ) ;
#46800 = DIRECTION ( 'NONE',  ( 0.000000000000000000, -1.000000000000000000, 0.000000000000000000 ) ) ;
#46801 = ADVANCED_FACE ( 'NONE', ( #47928 ), #11907, .T. ) ;
#46802 = CARTESIAN_POINT ( 'NONE',  ( 27.23560471289045992, -175.3837268820161057, 99.45993886622845537 ) ) ;
#46803 = ORIENTED_EDGE ( 'NONE', *, *, #7688, .F. ) ;
#46804 = CIRCLE ( 'NONE', #21627, 60.00000000000000000 ) ;
#46805 = CIRCLE ( 'NONE', #51014, 4.000000000000003553 ) ;
#46806 = ADVANCED_FACE ( 'NONE', ( #37121 ), #14003, .T. ) ;
#46807 = CARTESIAN_POINT ( 'NONE',  ( -172.4465090799742484, -189.7472609257535510, -2.844930291600662908 ) ) ;
#46808 = DIRECTION ( 'NONE',  ( 0.000000000000000000, -1.000000000000000000, 0.000000000000000000 ) ) ;
#46810 = AXIS2_PLACEMENT_3D ( 'NONE', #8535, #20367, #32196 ) ;
#46809 = DIRECTION ( 'NONE',  ( -0.000000000000000000, 0.6631226582407937498, -0.7485107481711024136 ) ) ;
#46811 = EDGE_CURVE ( 'NONE', #121, #40458, #41855, .T. ) ;
#46812 = CARTESIAN_POINT ( 'NONE',  ( -121.5885020763900997, -193.5000000000000000, -101.3904297239420913 ) ) ;
#46813 = CARTESIAN_POINT ( 'NONE',  ( -332.3517673607765914, -175.8491356171901145, 29.31839013542587224 ) ) ;
#46814 = ORIENTED_EDGE ( 'NONE', *, *, #10472, .F. ) ;
#46815 = AXIS2_PLACEMENT_3D ( 'NONE', #13527, #17217, #9077 ) ;
#46816 = DIRECTION ( 'NONE',  ( -0.2635871660690783380, 0.000000000000000000, 0.9646355819083558547 ) ) ;
#46817 = CIRCLE ( 'NONE', #6530, 60.00000000000000000 ) ;
#46818 = DIRECTION ( 'NONE',  ( -0.000000000000000000, 1.000000000000000000, -0.000000000000000000 ) ) ;
#46819 = CARTESIAN_POINT ( 'NONE',  ( 74.68865188374466868, -177.1207230881787780, 14.34663989163627740 ) ) ;
#46820 = DIRECTION ( 'NONE',  ( 1.000000000000000000, -0.000000000000000000, -0.000000000000000000 ) ) ;
#46821 = ORIENTED_EDGE ( 'NONE', *, *, #1872, .T. ) ;
#46822 = CARTESIAN_POINT ( 'NONE',  ( -332.3517673607765914, -66.60506506233235768, -15.70448169564047092 ) ) ;
#46823 = AXIS2_PLACEMENT_3D ( 'NONE', #9216, #49676, #12618 ) ;
#46824 = CARTESIAN_POINT ( 'NONE',  ( 40.71578595748725604, -183.6283474603465606, 86.14171647324928927 ) ) ;
#46825 = ORIENTED_EDGE ( 'NONE', *, *, #21789, .T. ) ;
#46826 = ORIENTED_EDGE ( 'NONE', *, *, #7986, .F. ) ;
#46827 = ORIENTED_EDGE ( 'NONE', *, *, #50822, .F. ) ;
#46828 = CARTESIAN_POINT ( 'NONE',  ( -305.0000000000000568, -165.2193480479701293, -43.12187378178659714 ) ) ;
#46829 = DIRECTION ( 'NONE',  ( 0.9266896074318291543, 0.000000000000000000, 0.3758275821142488260 ) ) ;
#46830 = CARTESIAN_POINT ( 'NONE',  ( -339.1964088526558498, -131.1080185721133660, -58.50955523165751515 ) ) ;
#46831 = VERTEX_POINT ( 'NONE', #5871 ) ;
#46832 = ADVANCED_FACE ( 'NONE', ( #12941 ), #13738, .T. ) ;
#46833 = FACE_OUTER_BOUND ( 'NONE', #35416, .T. ) ;
#46834 = CARTESIAN_POINT ( 'NONE',  ( 75.78974234412359579, -183.6283474603465606, 13.49993235881449394 ) ) ;
#46835 = VECTOR ( 'NONE', #3006, 1000.000000000000114 ) ;
#46838 = ORIENTED_EDGE ( 'NONE', *, *, #11773, .F. ) ;
#46837 = DIRECTION ( 'NONE',  ( 0.08879589532292483933, 0.000000000000000000, 0.9960498426152178952 ) ) ;
#46836 = LINE ( 'NONE', #3200, #20775 ) ;
#46839 = AXIS2_PLACEMENT_3D ( 'NONE', #35647, #51697, #15702 ) ;
#46840 = CARTESIAN_POINT ( 'NONE',  ( 5.015379008610418410, -193.5000000000000000, -112.9749434763326690 ) ) ;
#46841 = ORIENTED_EDGE ( 'NONE', *, *, #39617, .F. ) ;
#46842 = CARTESIAN_POINT ( 'NONE',  ( -49.21696003055058810, -193.5000000000000000, 0.6749830015182108900 ) ) ;
#46843 = VECTOR ( 'NONE', #44226, 1000.000000000000000 ) ;
#46844 = ORIENTED_EDGE ( 'NONE', *, *, #42744, .F. ) ;
#46845 = ADVANCED_FACE ( 'NONE', ( #37655 ), #33704, .F. ) ;
#46846 = EDGE_CURVE ( 'NONE', #20850, #4823, #7071, .T. ) ;
#46847 = ADVANCED_FACE ( 'NONE', ( #28968 ), #21097, .T. ) ;
#46848 = DIRECTION ( 'NONE',  ( -0.000000000000000000, -0.9350162426854121689, 0.3546048870425426158 ) ) ;
#46849 = FACE_OUTER_BOUND ( 'NONE', #38712, .T. ) ;
#46850 = FACE_OUTER_BOUND ( 'NONE', #33144, .T. ) ;
#46851 = ORIENTED_EDGE ( 'NONE', *, *, #29945, .T. ) ;
#46852 = EDGE_CURVE ( 'NONE', #23160, #3747, #9798, .T. ) ;
#46853 = VECTOR ( 'NONE', #7191, 1000.000000000000000 ) ;
#46854 = EDGE_LOOP ( 'NONE', ( #21560, #10830, #26206, #405 ) ) ;
#46855 = DIRECTION ( 'NONE',  ( -1.000000000000000000, -0.000000000000000000, -0.000000000000000000 ) ) ;
#46856 = FACE_OUTER_BOUND ( 'NONE', #4133, .T. ) ;
#46857 = EDGE_LOOP ( 'NONE', ( #43855, #41444, #48571, #13418 ) ) ;
#46858 = EDGE_CURVE ( 'NONE', #12980, #10123, #19658, .T. ) ;
#46859 = CARTESIAN_POINT ( 'NONE',  ( -18.31235070009513777, -189.7472609257535510, 121.3052580173829824 ) ) ;
#46860 = FACE_OUTER_BOUND ( 'NONE', #40885, .T. ) ;
#46861 = ORIENTED_EDGE ( 'NONE', *, *, #14759, .F. ) ;
#46862 = FACE_BOUND ( 'NONE', #26373, .T. ) ;
#46863 = EDGE_CURVE ( 'NONE', #4854, #11814, #45034, .T. ) ;
#46864 = LINE ( 'NONE', #10848, #33165 ) ;
#46865 = EDGE_CURVE ( 'NONE', #13250, #8786, #25059, .T. ) ;
#46866 = AXIS2_PLACEMENT_3D ( 'NONE', #30226, #46269, #26267 ) ;
#46867 = EDGE_LOOP ( 'NONE', ( #19599, #25899, #51478, #25343 ) ) ;
#46868 = CARTESIAN_POINT ( 'NONE',  ( -147.8383830610225971, -177.1207230881787780, -74.18852968774183410 ) ) ;
#46869 = ORIENTED_EDGE ( 'NONE', *, *, #27610, .T. ) ;
#46870 = EDGE_CURVE ( 'NONE', #42377, #23944, #9537, .T. ) ;
#46871 = CARTESIAN_POINT ( 'NONE',  ( -52.47502265695602119, -177.1207230881787780, -124.9361149384469485 ) ) ;
#46872 = CARTESIAN_POINT ( 'NONE',  ( -151.9915035862630646, -183.6283474603465606, 70.07273251429430161 ) ) ;
#46873 = ORIENTED_EDGE ( 'NONE', *, *, #17371, .T. ) ;
#46874 = EDGE_CURVE ( 'NONE', #12363, #27774, #45546, .T. ) ;
#46875 = DIRECTION ( 'NONE',  ( 0.000000000000000000, -0.000000000000000000, 1.000000000000000000 ) ) ;
#46876 = DIRECTION ( 'NONE',  ( -0.000000000000000000, 0.000000000000000000, 1.000000000000000000 ) ) ;
#46877 = LINE ( 'NONE', #27129, #45044 ) ;
#46878 = EDGE_CURVE ( 'NONE', #19748, #33685, #41320, .T. ) ;
#46879 = ORIENTED_EDGE ( 'NONE', *, *, #4844, .T. ) ;
#46880 = DIRECTION ( 'NONE',  ( -0.000000000000000000, -0.6631226582407989678, -0.7485107481710977506 ) ) ;
#46881 = AXIS2_PLACEMENT_3D ( 'NONE', #3989, #28138, #48133 ) ;
#46882 = VECTOR ( 'NONE', #15898, 1000.000000000000000 ) ;
#46883 = VECTOR ( 'NONE', #49673, 1000.000000000000000 ) ;
#46884 = LINE ( 'NONE', #46359, #10190 ) ;
#46885 = CARTESIAN_POINT ( 'NONE',  ( 36.84288420123322538, -177.1207230881787780, 91.35181687837501840 ) ) ;
#46887 = EDGE_LOOP ( 'NONE', ( #20008, #29761, #43878, #44113 ) ) ;
#46886 = CARTESIAN_POINT ( 'NONE',  ( -47.53180039765465636, -177.1207230881787780, -0.3202698538628280800 ) ) ;
#46888 = AXIS2_PLACEMENT_3D ( 'NONE', #41246, #5535, #8946 ) ;
#46889 = EDGE_LOOP ( 'NONE', ( #22069, #301, #38889, #17464 ) ) ;
#46890 = CARTESIAN_POINT ( 'NONE',  ( 72.71365293123227502, -177.1207230881787780, -30.61552143554913030 ) ) ;
#46891 = ADVANCED_FACE ( 'NONE', ( #9281 ), #17443, .F. ) ;
#46892 = CARTESIAN_POINT ( 'NONE',  ( 43.86477233319988756, -175.3837268820161057, -84.24728067915975771 ) ) ;
#46893 = VECTOR ( 'NONE', #9919, 1000.000000000000000 ) ;
#46894 = VERTEX_POINT ( 'NONE', #29490 ) ;
#46895 = FACE_OUTER_BOUND ( 'NONE', #42469, .T. ) ;
#46896 = ORIENTED_EDGE ( 'NONE', *, *, #28500, .F. ) ;
#46897 = PLANE ( 'NONE',  #6528 ) ;
#46898 = DIRECTION ( 'NONE',  ( 0.000000000000000000, -1.000000000000000000, 0.000000000000000000 ) ) ;
#46899 = CARTESIAN_POINT ( 'NONE',  ( -118.4380981977755880, -189.7472609257535510, -102.3804074221059892 ) ) ;
#46900 = DIRECTION ( 'NONE',  ( 0.9982437317643210184, 0.000000000000000000, 0.05924062789372143423 ) ) ;
#46901 = ORIENTED_EDGE ( 'NONE', *, *, #17028, .F. ) ;
#46902 = ORIENTED_EDGE ( 'NONE', *, *, #30836, .T. ) ;
#46903 = ORIENTED_EDGE ( 'NONE', *, *, #17172, .T. ) ;
#46904 = AXIS2_PLACEMENT_3D ( 'NONE', #49310, #45371, #9359 ) ;
#46905 = LINE ( 'NONE', #10885, #5671 ) ;
#46906 = DIRECTION ( 'NONE',  ( -1.000000000000000000, 0.000000000000000000, 0.000000000000000000 ) ) ;
#46907 = LINE ( 'NONE', #10887, #30824 ) ;
#46908 = DIRECTION ( 'NONE',  ( 1.000000000000000000, -0.000000000000000000, 0.000000000000000000 ) ) ;
#46909 = FACE_OUTER_BOUND ( 'NONE', #35595, .T. ) ;
#46910 = ORIENTED_EDGE ( 'NONE', *, *, #25745, .F. ) ;
#46911 = EDGE_CURVE ( 'NONE', #4103, #18062, #8743, .T. ) ;
#46912 = PRODUCT_DEFINITION_CONTEXT ( 'detailed design', #46486, 'design' ) ;
#46913 = EDGE_CURVE ( 'NONE', #31214, #41614, #49230, .T. ) ;
#46914 = CARTESIAN_POINT ( 'NONE',  ( -336.3521761649654422, -166.5797264208035244, 40.34602258462248159 ) ) ;
#46915 = LINE ( 'NONE', #35069, #9759 ) ;
#46916 = ADVANCED_FACE ( 'NONE', ( #29246 ), #45299, .T. ) ;
#46917 = EDGE_CURVE ( 'NONE', #50927, #13015, #2934, .T. ) ;
#46918 = VERTEX_POINT ( 'NONE', #34230 ) ;
#46919 = VERTEX_POINT ( 'NONE', #18974 ) ;
#46920 = AXIS2_PLACEMENT_3D ( 'NONE', #35995, #11282, #47830 ) ;
#46921 = CIRCLE ( 'NONE', #51129, 125.0000000000000000 ) ;
#46922 = CARTESIAN_POINT ( 'NONE',  ( -332.3517673607765914, -81.08339623743702873, -41.09453333279329712 ) ) ;
#46923 = DIRECTION ( 'NONE',  ( -0.1182731709213660498, 0.000000000000000000, 0.9929810960135169173 ) ) ;
#46924 = LINE ( 'NONE', #23255, #22497 ) ;
#46925 = CARTESIAN_POINT ( 'NONE',  ( -139.0630283577175987, -183.6283474603465606, -86.13684908212449898 ) ) ;
#46926 = AXIS2_PLACEMENT_3D ( 'NONE', #40651, #9400, #29098 ) ;
#46927 = DIRECTION ( 'NONE',  ( 0.000000000000000000, 0.3546048870425300148, -0.9350162426854169428 ) ) ;
#46928 = CARTESIAN_POINT ( 'NONE',  ( -339.1964088526558498, -123.9999999999993747, 59.00000000000002132 ) ) ;
#46929 = VERTEX_POINT ( 'NONE', #10829 ) ;
#46930 = CARTESIAN_POINT ( 'NONE',  ( -25.55153130240594450, -189.7472609257535510, 122.8793122007210599 ) ) ;
#46931 = VERTEX_POINT ( 'NONE', #38673 ) ;
#46932 = FACE_OUTER_BOUND ( 'NONE', #6509, .T. ) ;
#46933 = EDGE_CURVE ( 'NONE', #48929, #18230, #30280, .T. ) ;
#46934 = CARTESIAN_POINT ( 'NONE',  ( -168.1386673294336163, -175.3837268820161057, 32.52067927015838222 ) ) ;
#46935 = ORIENTED_EDGE ( 'NONE', *, *, #49093, .T. ) ;
#46936 = CARTESIAN_POINT ( 'NONE',  ( -133.0671220150036334, -177.1207230881787780, -92.03190238880748097 ) ) ;
#46937 = LINE ( 'NONE', #27185, #31409 ) ;
#46938 = FACE_OUTER_BOUND ( 'NONE', #46854, .T. ) ;
#46939 = CARTESIAN_POINT ( 'NONE',  ( -104.8182102393454045, -175.3837268820161057, 111.5836353223472912 ) ) ;
#46940 = EDGE_CURVE ( 'NONE', #5804, #8278, #7140, .T. ) ;
#46941 = CIRCLE ( 'NONE', #15873, 60.00000000000000000 ) ;
#46942 = CARTESIAN_POINT ( 'NONE',  ( -48.47912675150885065, -183.6283474603465606, 6.938893903907228378E-15 ) ) ;
#46943 = ORIENTED_EDGE ( 'NONE', *, *, #22870, .T. ) ;
#46944 = LINE ( 'NONE', #6732, #21441 ) ;
#46946 = ORIENTED_EDGE ( 'NONE', *, *, #13677, .F. ) ;
#46945 = CARTESIAN_POINT ( 'NONE',  ( -47.78257572244585560, -193.5000000000000000, -0.7175072570443230546 ) ) ;
#46947 = ORIENTED_EDGE ( 'NONE', *, *, #34658, .T. ) ;
#46948 = LINE ( 'NONE', #34327, #33841 ) ;
#46949 = ORIENTED_EDGE ( 'NONE', *, *, #40407, .T. ) ;
#46950 = DIRECTION ( 'NONE',  ( -0.000000000000000000, 1.000000000000000000, -0.000000000000000000 ) ) ;
#46951 = ORIENTED_EDGE ( 'NONE', *, *, #38198, .T. ) ;
#46952 = VECTOR ( 'NONE', #49141, 1000.000000000000114 ) ;
#46953 = DIRECTION ( 'NONE',  ( 0.000000000000000000, 1.000000000000000000, 0.000000000000000000 ) ) ;
#46954 = DIRECTION ( 'NONE',  ( 0.000000000000000000, 0.000000000000000000, 1.000000000000000000 ) ) ;
#46955 = ORIENTED_EDGE ( 'NONE', *, *, #36497, .T. ) ;
#46956 = DIRECTION ( 'NONE',  ( 0.000000000000000000, -0.000000000000000000, -1.000000000000000000 ) ) ;
#46957 =( GEOMETRIC_REPRESENTATION_CONTEXT ( 3 ) GLOBAL_UNCERTAINTY_ASSIGNED_CONTEXT ( ( #5409 ) ) GLOBAL_UNIT_ASSIGNED_CONTEXT ( ( #30388, #50908, #5730 ) ) REPRESENTATION_CONTEXT ( 'NONE', 'WORKASPACE' ) );
#46958 = EDGE_CURVE ( 'NONE', #49907, #34582, #6246, .T. ) ;
#46959 = DIRECTION ( 'NONE',  ( 1.000000000000000000, -0.000000000000000000, -0.000000000000000000 ) ) ;
#46960 = LINE ( 'NONE', #10683, #24038 ) ;
#46961 = ORIENTED_EDGE ( 'NONE', *, *, #45210, .F. ) ;
#46962 = ORIENTED_EDGE ( 'NONE', *, *, #11033, .F. ) ;
#46963 = ORIENTED_EDGE ( 'NONE', *, *, #2010, .T. ) ;
#46964 = LINE ( 'NONE', #26183, #19200 ) ;
#46965 = CARTESIAN_POINT ( 'NONE',  ( 0.000000000000000000, -43.50000000000000000, 0.000000000000000000 ) ) ;
#46966 = DIRECTION ( 'NONE',  ( 1.000000000000000000, -0.000000000000000000, -0.000000000000000000 ) ) ;
#46967 = CARTESIAN_POINT ( 'NONE',  ( -75.48985759771373694, -177.1207230881787780, -122.0467960216648748 ) ) ;
#46968 = FACE_OUTER_BOUND ( 'NONE', #51232, .T. ) ;
#46969 = VERTEX_POINT ( 'NONE', #30797 ) ;
#46970 = ADVANCED_FACE ( 'NONE', ( #34477 ), #2435, .F. ) ;
#46971 = EDGE_CURVE ( 'NONE', #31192, #28668, #42359, .T. ) ;
#46972 = VECTOR ( 'NONE', #15122, 1000.000000000000114 ) ;
#46973 = DIRECTION ( 'NONE',  ( 0.000000000000000000, 6.938893903907222461E-16, 1.000000000000000000 ) ) ;
#46974 = EDGE_LOOP ( 'NONE', ( #29507, #23346, #50573, #39603 ) ) ;
#46976 = EDGE_LOOP ( 'NONE', ( #33325, #34567, #8853, #32015 ) ) ;
#46975 = LINE ( 'NONE', #30928, #46628 ) ;
#46977 = ORIENTED_EDGE ( 'NONE', *, *, #45312, .T. ) ;
#46978 = LINE ( 'NONE', #26980, #19073 ) ;
#46979 = DIRECTION ( 'NONE',  ( 0.000000000000000000, -0.6631226582408016323, -0.7485107481710953081 ) ) ;
#46980 = LINE ( 'NONE', #11732, #33871 ) ;
#46981 = FACE_OUTER_BOUND ( 'NONE', #40270, .T. ) ;
#46982 = ORIENTED_EDGE ( 'NONE', *, *, #47073, .F. ) ;
#46983 = CARTESIAN_POINT ( 'NONE',  ( 4.109287492203097081, -177.1207230881787780, -113.3995532942337121 ) ) ;
#46984 = EDGE_LOOP ( 'NONE', ( #21677, #27195, #16112, #21440 ) ) ;
#46985 = EDGE_LOOP ( 'NONE', ( #29068, #45861 ) ) ;
#46986 = DIRECTION ( 'NONE',  ( 0.000000000000000000, 0.000000000000000000, 1.000000000000000000 ) ) ;
#46987 = CARTESIAN_POINT ( 'NONE',  ( 42.10477485469927927, -177.1207230881787780, 86.13684908212515268 ) ) ;
#46988 = ADVANCED_FACE ( 'NONE', ( #18715 ), #42628, .T. ) ;
#46989 = CARTESIAN_POINT ( 'NONE',  ( 68.59638248015004081, -177.1207230881787780, -43.79868877201405297 ) ) ;
#46990 = DIRECTION ( 'NONE',  ( 0.000000000000000000, 0.000000000000000000, 1.000000000000000000 ) ) ;
#46991 = ORIENTED_EDGE ( 'NONE', *, *, #31993, .T. ) ;
#46992 = CARTESIAN_POINT ( 'NONE',  ( 76.37123734610607073, -183.6283474603465606, 6.114457023561876703 ) ) ;
#46993 = LINE ( 'NONE', #22806, #37340 ) ;
#46994 = LINE ( 'NONE', #42250, #5361 ) ;
#46995 = FACE_OUTER_BOUND ( 'NONE', #47927, .T. ) ;
#46996 = ORIENTED_EDGE ( 'NONE', *, *, #44336, .F. ) ;
#46997 = DIRECTION ( 'NONE',  ( -0.000000000000000000, 1.000000000000000000, -0.000000000000000000 ) ) ;
#46998 = CARTESIAN_POINT ( 'NONE',  ( -159.5526844214375615, -193.5000000000000000, 57.33816169485226055 ) ) ;
#46999 = ADVANCED_FACE ( 'NONE', ( #19238 ), #34729, .T. ) ;
#47000 = DIRECTION ( 'NONE',  ( -0.000000000000000000, 1.000000000000000000, -0.000000000000000000 ) ) ;
#47001 = EDGE_LOOP ( 'NONE', ( #43719, #5722, #27484, #3721 ) ) ;
#47002 = CARTESIAN_POINT ( 'NONE',  ( 55.91309001144629320, -183.6283474603465606, 68.75510947788671956 ) ) ;
#47003 = CYLINDRICAL_SURFACE ( 'NONE', #45432, 124.9999999999999858 ) ;
#47004 = ORIENTED_EDGE ( 'NONE', *, *, #28871, .F. ) ;
#47005 = CYLINDRICAL_SURFACE ( 'NONE', #47256, 125.0000000000000000 ) ;
#47006 = EDGE_CURVE ( 'NONE', #19975, #37889, #15044, .T. ) ;
#47007 = ORIENTED_EDGE ( 'NONE', *, *, #49191, .F. ) ;
#47008 = VECTOR ( 'NONE', #2018, 1000.000000000000114 ) ;
#47009 = AXIS2_PLACEMENT_3D ( 'NONE', #48748, #12718, #7506 ) ;
#47010 = FACE_OUTER_BOUND ( 'NONE', #49694, .T. ) ;
#47011 = FACE_BOUND ( 'NONE', #26061, .T. ) ;
#47012 = LINE ( 'NONE', #6556, #13697 ) ;
#47013 = CARTESIAN_POINT ( 'NONE',  ( -330.4913330509368166, -181.8741440471346493, 13.87297036558422825 ) ) ;
#47014 = VERTEX_POINT ( 'NONE', #6642 ) ;
#47015 = EDGE_CURVE ( 'NONE', #39351, #8427, #17206, .T. ) ;
#47016 = EDGE_LOOP ( 'NONE', ( #22180, #2268, #11304, #14567 ) ) ;
#47017 = LINE ( 'NONE', #46760, #7426 ) ;
#47018 = CIRCLE ( 'NONE', #9250, 60.00000000000000000 ) ;
#47019 = VERTEX_POINT ( 'NONE', #2161 ) ;
#47020 = PLANE ( 'NONE',  #15857 ) ;
#47021 = EDGE_CURVE ( 'NONE', #18124, #47386, #2068, .T. ) ;
#47022 = ADVANCED_FACE ( 'NONE', ( #31047 ), #14784, .F. ) ;
#47023 = CARTESIAN_POINT ( 'NONE',  ( -48.64924157374594671, -193.5000000000000000, 124.9998842437354227 ) ) ;
#47024 = CARTESIAN_POINT ( 'NONE',  ( -332.3517673607765914, -154.8494888031386836, 50.05135858667791382 ) ) ;
#47025 = ORIENTED_EDGE ( 'NONE', *, *, #10528, .F. ) ;
#47028 = VERTEX_POINT ( 'NONE', #38150 ) ;
#47027 = CARTESIAN_POINT ( 'NONE',  ( -50.89116676070551648, -177.1207230881787780, 124.9767260852757147 ) ) ;
#47026 = CARTESIAN_POINT ( 'NONE',  ( -2.727113817024051201, 51.29627183467966489, -20.73351566952182878 ) ) ;
#47029 = EDGE_CURVE ( 'NONE', #35813, #23503, #14522, .T. ) ;
#47030 = CARTESIAN_POINT ( 'NONE',  ( -144.6608085595393902, -193.5000000000000000, -78.26291788638665992 ) ) ;
#47031 = EDGE_LOOP ( 'NONE', ( #2022, #44505, #19533, #12749 ) ) ;
#47032 = LINE ( 'NONE', #14461, #23047 ) ;
#47033 = EDGE_LOOP ( 'NONE', ( #51171, #34456, #40940, #7078 ) ) ;
#47034 = EDGE_CURVE ( 'NONE', #1525, #23565, #27097, .T. ) ;
#47035 = CARTESIAN_POINT ( 'NONE',  ( -330.4913330509368166, -175.9742670995611036, 26.97593913775620678 ) ) ;
#47036 = EDGE_LOOP ( 'NONE', ( #17810, #370, #16946, #41118 ) ) ;
#47039 = VERTEX_POINT ( 'NONE', #23180 ) ;
#47038 = DIRECTION ( 'NONE',  ( -0.000000000000000000, 1.000000000000000000, -0.000000000000000000 ) ) ;
#47037 = CARTESIAN_POINT ( 'NONE',  ( -339.1964088526558498, -181.6348283828470755, 14.84391218301028026 ) ) ;
#47040 = VERTEX_POINT ( 'NONE', #18206 ) ;
#47041 = AXIS2_PLACEMENT_3D ( 'NONE', #28188, #40013, #51605 ) ;
#47042 = VECTOR ( 'NONE', #18743, 1000.000000000000341 ) ;
#47043 = DIRECTION ( 'NONE',  ( -0.000000000000000000, 1.000000000000000000, -0.000000000000000000 ) ) ;
#47044 = VERTEX_POINT ( 'NONE', #39197 ) ;
#47045 = LINE ( 'NONE', #39136, #33744 ) ;
#47046 = LINE ( 'NONE', #10260, #10593 ) ;
#47047 = ORIENTED_EDGE ( 'NONE', *, *, #29349, .F. ) ;
#47048 = EDGE_CURVE ( 'NONE', #28063, #12334, #35763, .T. ) ;
#47049 = CARTESIAN_POINT ( 'NONE',  ( 28.62116745695381326, -193.5000000000000000, -97.11716833071837129 ) ) ;
#47050 = CARTESIAN_POINT ( 'NONE',  ( -130.0559183202350084, -193.5000000000000000, -93.38753978496592367 ) ) ;
#47051 = DIRECTION ( 'NONE',  ( 1.000000000000000000, -0.000000000000000000, -0.000000000000000000 ) ) ;
#47052 = DIRECTION ( 'NONE',  ( 0.000000000000000000, -0.000000000000000000, 1.000000000000000000 ) ) ;
#47053 = ORIENTED_EDGE ( 'NONE', *, *, #681, .T. ) ;
#47054 = DIRECTION ( 'NONE',  ( 0.000000000000000000, 0.000000000000000000, 1.000000000000000000 ) ) ;
#47055 = DIRECTION ( 'NONE',  ( 0.2348860457809842095, 0.000000000000000000, -0.9720229140804107493 ) ) ;
#47056 = FACE_OUTER_BOUND ( 'NONE', #11572, .T. ) ;
#47057 = DIRECTION ( 'NONE',  ( 0.000000000000000000, -0.000000000000000000, 1.000000000000000000 ) ) ;
#47058 = VERTEX_POINT ( 'NONE', #36279 ) ;
#47059 = VECTOR ( 'NONE', #12017, 1000.000000000000000 ) ;
#47060 = CARTESIAN_POINT ( 'NONE',  ( 26.52087324849106054, -198.5000000000000000, -60.00000000000003553 ) ) ;
#47061 = LINE ( 'NONE', #15253, #47929 ) ;
#47062 = CARTESIAN_POINT ( 'NONE',  ( -332.3517673607765914, -123.5000000000000284, 0.000000000000000000 ) ) ;
#47063 = LINE ( 'NONE', #51021, #31944 ) ;
#47064 = CARTESIAN_POINT ( 'NONE',  ( -340.0000000000000568, -168.5000000000000284, -5.000000000000001776 ) ) ;
#47065 = ORIENTED_EDGE ( 'NONE', *, *, #16233, .T. ) ;
#47066 = CARTESIAN_POINT ( 'NONE',  ( -170.0000000000000284, 0.000000000000000000, 0.000000000000000000 ) ) ;
#47067 = FACE_OUTER_BOUND ( 'NONE', #20672, .T. ) ;
#47068 = DIRECTION ( 'NONE',  ( 0.000000000000000000, 0.000000000000000000, -1.000000000000000000 ) ) ;
#47069 = FACE_OUTER_BOUND ( 'NONE', #1076, .T. ) ;
#47070 = CYLINDRICAL_SURFACE ( 'NONE', #46377, 4.000000000000003553 ) ;
#47071 = AXIS2_PLACEMENT_3D ( 'NONE', #45573, #17972, #26623 ) ;
#47072 = ORIENTED_EDGE ( 'NONE', *, *, #49697, .T. ) ;
#47073 = EDGE_CURVE ( 'NONE', #346, #10684, #47871, .T. ) ;
#47074 = EDGE_CURVE ( 'NONE', #35097, #30216, #32328, .T. ) ;
#47075 = CARTESIAN_POINT ( 'NONE',  ( 3.549863570076594588, 51.93797953136993328, -20.18436947879331456 ) ) ;
#47076 = AXIS2_PLACEMENT_3D ( 'NONE', #47838, #11808, #27837 ) ;
#47077 = DIRECTION ( 'NONE',  ( -1.000000000000000000, 0.000000000000000000, 0.000000000000000000 ) ) ;
#47078 = ORIENTED_EDGE ( 'NONE', *, *, #39408, .F. ) ;
#47079 = VERTEX_POINT ( 'NONE', #23936 ) ;
#47080 = VERTEX_POINT ( 'NONE', #11324 ) ;
#47081 = CARTESIAN_POINT ( 'NONE',  ( -98.71382891444399377, -175.3837268820161057, -114.4616734920523555 ) ) ;
#47082 = ADVANCED_FACE ( 'NONE', ( #32080 ), #7416, .T. ) ;
#47083 = DIRECTION ( 'NONE',  ( -0.9995608365087942371, 0.000000000000000000, -0.02963332782256331357 ) ) ;
#47084 = ORIENTED_EDGE ( 'NONE', *, *, #1576, .F. ) ;
#47085 = ADVANCED_FACE ( 'NONE', ( #39688 ), #16595, .F. ) ;
#47086 = DIRECTION ( 'NONE',  ( 0.000000000000000000, 0.000000000000000000, -1.000000000000000000 ) ) ;
#47087 = DIRECTION ( 'NONE',  ( -0.8294056854502090959, 0.000000000000000000, 0.5586467658036415873 ) ) ;
#47090 = ORIENTED_EDGE ( 'NONE', *, *, #45012, .F. ) ;
#47089 = CARTESIAN_POINT ( 'NONE',  ( -305.0000000000000568, -162.0508476703726330, 45.97643030831914501 ) ) ;
#47088 = LINE ( 'NONE', #11064, #4015 ) ;
#47091 = EDGE_CURVE ( 'NONE', #8761, #26482, #279, .T. ) ;
#47092 = VECTOR ( 'NONE', #23799, 1000.000000000000000 ) ;
#47093 = LINE ( 'NONE', #35760, #39026 ) ;
#47094 = VERTEX_POINT ( 'NONE', #3977 ) ;
#47095 = CARTESIAN_POINT ( 'NONE',  ( -332.3517673607765914, -180.1556192733800117, 16.67542351306693149 ) ) ;
#47096 = ORIENTED_EDGE ( 'NONE', *, *, #12967, .F. ) ;
#47097 = DIRECTION ( 'NONE',  ( -0.1182731709213523247, 0.000000000000000000, -0.9929810960135185827 ) ) ;
#47098 = DIRECTION ( 'NONE',  ( 0.000000000000000000, 1.000000000000000000, 0.000000000000000000 ) ) ;
#47100 = CARTESIAN_POINT ( 'NONE',  ( -1.230335819511596540, -177.1207230881787780, 115.7261930397108358 ) ) ;
#47099 = DIRECTION ( 'NONE',  ( -1.000000000000000000, 0.000000000000000000, -0.000000000000000000 ) ) ;
#47101 = ORIENTED_EDGE ( 'NONE', *, *, #43259, .T. ) ;
#47102 = PLANE ( 'NONE',  #32354 ) ;
#47103 = ORIENTED_EDGE ( 'NONE', *, *, #5676, .F. ) ;
#47104 = DIRECTION ( 'NONE',  ( 0.000000000000000000, 0.000000000000000000, 1.000000000000000000 ) ) ;
#47105 = CARTESIAN_POINT ( 'NONE',  ( -45.06671089634843952, -193.5000000000000000, -124.9534129907280402 ) ) ;
#47106 = VERTEX_POINT ( 'NONE', #20001 ) ;
#47107 = DIRECTION ( 'NONE',  ( -0.000000000000000000, 0.3546048870425463906, 0.9350162426854107256 ) ) ;
#47108 = AXIS2_PLACEMENT_3D ( 'NONE', #28417, #32106, #48151 ) ;
#47109 = DIRECTION ( 'NONE',  ( 1.000000000000000000, 0.000000000000000000, 0.000000000000000000 ) ) ;
#47110 = ORIENTED_EDGE ( 'NONE', *, *, #8208, .T. ) ;
#47111 = FACE_OUTER_BOUND ( 'NONE', #44438, .T. ) ;
#47112 = CARTESIAN_POINT ( 'NONE',  ( 64.29733702426840125, -175.3837268820161057, 53.91167979418565892 ) ) ;
#47113 = CIRCLE ( 'NONE', #41240, 125.0000000000000000 ) ;
#47114 = VERTEX_POINT ( 'NONE', #20256 ) ;
#47115 = DIRECTION ( 'NONE',  ( -1.000000000000000000, 0.000000000000000000, 0.000000000000000000 ) ) ;
#47116 = ORIENTED_EDGE ( 'NONE', *, *, #23067, .T. ) ;
#47117 = VECTOR ( 'NONE', #49005, 1000.000000000000000 ) ;
#47118 = DIRECTION ( 'NONE',  ( -0.000000000000000000, 0.000000000000000000, 1.000000000000000000 ) ) ;
#47119 = DIRECTION ( 'NONE',  ( 0.9960498426152165630, 0.000000000000000000, 0.08879589532293852283 ) ) ;
#47120 = VERTEX_POINT ( 'NONE', #40474 ) ;
#47121 = CARTESIAN_POINT ( 'NONE',  ( -135.4258661347518853, -175.3837268820161057, -89.80681772907007598 ) ) ;
#47122 = FACE_OUTER_BOUND ( 'NONE', #43267, .T. ) ;
#47123 = CARTESIAN_POINT ( 'NONE',  ( -19.28375372365792728, -193.5000000000000000, 121.5427093402341541 ) ) ;
#47124 = DIRECTION ( 'NONE',  ( -1.000000000000000000, 0.000000000000000000, -0.000000000000000000 ) ) ;
#47125 = CIRCLE ( 'NONE', #21949, 125.0000000000000000 ) ;
#47126 = DIRECTION ( 'NONE',  ( 0.000000000000000000, 0.000000000000000000, -1.000000000000000000 ) ) ;
#47127 = CARTESIAN_POINT ( 'NONE',  ( -332.3517673607765914, -87.81784868886214213, 47.06073758877343494 ) ) ;
#47129 = EDGE_LOOP ( 'NONE', ( #17430, #40575, #347, #21159 ) ) ;
#47128 = DIRECTION ( 'NONE',  ( 0.000000000000000000, -1.000000000000000000, 0.000000000000000000 ) ) ;
#47130 = EDGE_CURVE ( 'NONE', #31203, #36752, #20511, .T. ) ;
#47131 = ORIENTED_EDGE ( 'NONE', *, *, #4123, .T. ) ;
#47132 = EDGE_CURVE ( 'NONE', #9298, #50508, #39443, .T. ) ;
#47133 = ADVANCED_FACE ( 'NONE', ( #51548 ), #12367, .F. ) ;
#47134 = CARTESIAN_POINT ( 'NONE',  ( 76.31829002442924548, -177.1207230881787780, 7.113702696402420145 ) ) ;
#47135 = EDGE_CURVE ( 'NONE', #14246, #44579, #11601, .T. ) ;
#47136 = CARTESIAN_POINT ( 'NONE',  ( -48.47912675150885065, -183.6283474603465606, 6.938893903907228378E-15 ) ) ;
#47137 = EDGE_LOOP ( 'NONE', ( #4586, #24536, #32145, #38851 ) ) ;
#47138 = EDGE_LOOP ( 'NONE', ( #1646, #20718, #17643, #44323 ) ) ;
#47139 = DIRECTION ( 'NONE',  ( 0.9995608365087946812, 0.000000000000000000, -0.02963332782254913048 ) ) ;
#47140 = EDGE_CURVE ( 'NONE', #14358, #49982, #27628, .T. ) ;
#47141 = EDGE_LOOP ( 'NONE', ( #42291, #11477, #4112, #6526 ) ) ;
#47142 = DIRECTION ( 'NONE',  ( -0.000000000000000000, 1.000000000000000000, -0.000000000000000000 ) ) ;
#47143 = CARTESIAN_POINT ( 'NONE',  ( -49.13194886969938580, -177.1207230881787780, 0.7575112421616214675 ) ) ;
#47144 = ADVANCED_FACE ( 'NONE', ( #3444 ), #7653, .T. ) ;
#47145 = VECTOR ( 'NONE', #26936, 1000.000000000000000 ) ;
#47146 = ADVANCED_FACE ( 'NONE', ( #4496 ), #23439, .F. ) ;
#47147 = DIRECTION ( 'NONE',  ( 0.000000000000000000, 0.000000000000000000, 1.000000000000000000 ) ) ;
#47148 = DIRECTION ( 'NONE',  ( 0.000000000000000000, 0.6631226582408039638, 0.7485107481710934207 ) ) ;
#47149 = CIRCLE ( 'NONE', #35386, 60.00000000000000000 ) ;
#47150 = ORIENTED_EDGE ( 'NONE', *, *, #2093, .F. ) ;
#47151 = ORIENTED_EDGE ( 'NONE', *, *, #16722, .F. ) ;
#47152 = ADVANCED_FACE ( 'NONE', ( #23672 ), #43410, .T. ) ;
#47154 = ORIENTED_EDGE ( 'NONE', *, *, #49004, .F. ) ;
#47153 = VECTOR ( 'NONE', #13972, 1000.000000000000114 ) ;
#47155 = EDGE_CURVE ( 'NONE', #14073, #21253, #19730, .T. ) ;
#47156 = CARTESIAN_POINT ( 'NONE',  ( -330.4913330509368166, -123.0000000000002700, -59.00000000000002132 ) ) ;
#47157 = LINE ( 'NONE', #51120, #18490 ) ;
#47158 = FACE_OUTER_BOUND ( 'NONE', #592, .T. ) ;
#47159 = EDGE_CURVE ( 'NONE', #49057, #49769, #13163, .T. ) ;
#47160 = CARTESIAN_POINT ( 'NONE',  ( 23.54917025746144432, -193.5000000000000000, -100.9358816284410381 ) ) ;
#47161 = FACE_BOUND ( 'NONE', #36278, .T. ) ;
#47162 = EDGE_LOOP ( 'NONE', ( #2914, #36088, #24765, #20736 ) ) ;
#47163 = EDGE_CURVE ( 'NONE', #16495, #16650, #9734, .T. ) ;
#47164 = DIRECTION ( 'NONE',  ( 1.043714542225393381E-14, -0.7485107481710977506, 0.6631226582407989678 ) ) ;
#47165 = DIRECTION ( 'NONE',  ( -0.000000000000000000, 1.000000000000000000, -0.000000000000000000 ) ) ;
#47166 = AXIS2_PLACEMENT_3D ( 'NONE', #38710, #11363, #34763 ) ;
#47167 = VERTEX_POINT ( 'NONE', #5818 ) ;
#47168 = VERTEX_POINT ( 'NONE', #5286 ) ;
#47169 = AXIS2_PLACEMENT_3D ( 'NONE', #28577, #40390, #51537 ) ;
#47170 = CARTESIAN_POINT ( 'NONE',  ( -168.4003408533108086, -177.1207230881787780, -35.26900067126612726 ) ) ;
#47171 = CARTESIAN_POINT ( 'NONE',  ( -91.22542124915045747, -189.7472609257535510, 117.4638425504669783 ) ) ;
#47172 = FACE_OUTER_BOUND ( 'NONE', #45588, .T. ) ;
#47173 = CARTESIAN_POINT ( 'NONE',  ( 46.00000000000000711, 35.00000000000000000, -46.00000000000000000 ) ) ;
#47174 = CARTESIAN_POINT ( 'NONE',  ( -48.47912675150885065, -117.5479369270332057, 15.00000000000000711 ) ) ;
#47175 = VERTEX_POINT ( 'NONE', #17636 ) ;
#47176 = DIRECTION ( 'NONE',  ( -0.9890401873221633666, 0.000000000000000000, -0.1476465640024850756 ) ) ;
#47177 = EDGE_CURVE ( 'NONE', #14469, #51370, #44697, .T. ) ;
#47178 = ORIENTED_EDGE ( 'NONE', *, *, #904, .F. ) ;
#47179 = CARTESIAN_POINT ( 'NONE',  ( -173.2765435274470178, -193.5000000000000000, -7.113702696401505321 ) ) ;
#47180 = DIRECTION ( 'NONE',  ( -1.000000000000000000, 0.000000000000000000, 0.000000000000000000 ) ) ;
#47181 = ORIENTED_EDGE ( 'NONE', *, *, #34784, .T. ) ;
#47182 = AXIS2_PLACEMENT_3D ( 'NONE', #42827, #30481, #26536 ) ;
#47183 = FACE_OUTER_BOUND ( 'NONE', #25676, .T. ) ;
#47184 = FACE_BOUND ( 'NONE', #40720, .T. ) ;
#47185 = CARTESIAN_POINT ( 'NONE',  ( -111.3295483157475729, -189.7472609257535510, 108.0501018472332362 ) ) ;
#47186 = CIRCLE ( 'NONE', #25347, 125.0000000000000000 ) ;
#47187 = CARTESIAN_POINT ( 'NONE',  ( 8.750818922897911634, -175.3837268820161057, -111.1293539894138576 ) ) ;
#47188 = AXIS2_PLACEMENT_3D ( 'NONE', #48631, #12603, #28623 ) ;
#47189 = DIRECTION ( 'NONE',  ( -0.2348860457809911206, 0.000000000000000000, 0.9720229140804089729 ) ) ;
#47190 = EDGE_CURVE ( 'NONE', #32138, #48781, #45237, .T. ) ;
#47191 = ORIENTED_EDGE ( 'NONE', *, *, #50706, .F. ) ;
#47192 = CARTESIAN_POINT ( 'NONE',  ( -339.1964088526558498, -115.7716958700755470, -59.50019592636139265 ) ) ;
#47194 = ORIENTED_EDGE ( 'NONE', *, *, #1926, .T. ) ;
#47193 = PLANE ( 'NONE',  #6132 ) ;
#47195 = EDGE_CURVE ( 'NONE', #29294, #27708, #25553, .T. ) ;
#47196 = EDGE_CURVE ( 'NONE', #43465, #3202, #49682, .T. ) ;
#47197 = VERTEX_POINT ( 'NONE', #1839 ) ;
#47198 = EDGE_CURVE ( 'NONE', #43364, #32964, #810, .T. ) ;
#47199 = DIRECTION ( 'NONE',  ( 5.399917434947259359E-17, 1.000000000000000000, -0.000000000000000000 ) ) ;
#47200 = ADVANCED_FACE ( 'NONE', ( #24723 ), #29432, .T. ) ;
#47201 = ORIENTED_EDGE ( 'NONE', *, *, #23417, .T. ) ;
#47202 = AXIS2_PLACEMENT_3D ( 'NONE', #11047, #23157, #3181 ) ;
#47203 = VECTOR ( 'NONE', #42233, 1000.000000000000000 ) ;
#47204 = EDGE_CURVE ( 'NONE', #49045, #14293, #377, .T. ) ;
#47205 = CARTESIAN_POINT ( 'NONE',  ( -305.0000000000000568, -151.8251501453684682, -52.89315522109013301 ) ) ;
#47206 = VECTOR ( 'NONE', #25285, 1000.000000000000000 ) ;
#47207 = ORIENTED_EDGE ( 'NONE', *, *, #26836, .T. ) ;
#47208 = CARTESIAN_POINT ( 'NONE',  ( 0.000000000000000000, 20.00000000000000000, 0.000000000000000000 ) ) ;
#47209 = EDGE_CURVE ( 'NONE', #47963, #27143, #33643, .T. ) ;
#47210 = CARTESIAN_POINT ( 'NONE',  ( -330.4913330509368166, -178.4886558749180949, 21.38919645685269444 ) ) ;
#47211 = ORIENTED_EDGE ( 'NONE', *, *, #19492, .F. ) ;
#47212 = PLANE ( 'NONE',  #32509 ) ;
#47213 = EDGE_CURVE ( 'NONE', #23398, #42501, #36815, .T. ) ;
#47214 = DIRECTION ( 'NONE',  ( -0.000000000000000000, -0.2393156642875482742, 0.9709418174260544543 ) ) ;
#47215 = FACE_OUTER_BOUND ( 'NONE', #10385, .T. ) ;
#47216 = ORIENTED_EDGE ( 'NONE', *, *, #5473, .T. ) ;
#47217 = ORIENTED_EDGE ( 'NONE', *, *, #15342, .T. ) ;
#47218 = EDGE_CURVE ( 'NONE', #2378, #32936, #37062, .T. ) ;
#47219 = VERTEX_POINT ( 'NONE', #21573 ) ;
#47220 = CARTESIAN_POINT ( 'NONE',  ( -336.3521761649654422, -123.5000000000000284, 0.000000000000000000 ) ) ;
#47221 = PLANE ( 'NONE',  #27669 ) ;
#47222 = ADVANCED_FACE ( 'NONE', ( #49168 ), #12623, .F. ) ;
#47223 = DIRECTION ( 'NONE',  ( 0.000000000000000000, 0.8854560256532093554, -0.4647231720437695057 ) ) ;
#47224 = DIRECTION ( 'NONE',  ( -0.2635871660690648488, 0.000000000000000000, -0.9646355819083595184 ) ) ;
#47225 = CARTESIAN_POINT ( 'NONE',  ( -330.4913330509368166, -66.09477493971917283, -13.63415328425296202 ) ) ;
#47226 = VECTOR ( 'NONE', #17064, 1000.000000000000000 ) ;
#47227 = ORIENTED_EDGE ( 'NONE', *, *, #3849, .T. ) ;
#47228 = EDGE_CURVE ( 'NONE', #28733, #48345, #45717, .T. ) ;
#47229 = EDGE_CURVE ( 'NONE', #41296, #37599, #8784, .T. ) ;
#47230 = AXIS2_PLACEMENT_3D ( 'NONE', #6350, #26051, #2130 ) ;
#47231 = DIRECTION ( 'NONE',  ( 0.000000000000000000, -0.000000000000000000, -1.000000000000000000 ) ) ;
#47232 = ORIENTED_EDGE ( 'NONE', *, *, #42625, .T. ) ;
#47234 = ORIENTED_EDGE ( 'NONE', *, *, #2224, .T. ) ;
#47233 = CARTESIAN_POINT ( 'NONE',  ( 61.38599058177058510, -175.3837268820161057, 59.62093586438192716 ) ) ;
#47235 = ORIENTED_EDGE ( 'NONE', *, *, #18255, .T. ) ;
#47236 = DIRECTION ( 'NONE',  ( -0.000000000000000000, 1.000000000000000000, -0.000000000000000000 ) ) ;
#47237 = DIRECTION ( 'NONE',  ( -0.4300652022765183435, 0.000000000000000000, -0.9027978299657446470 ) ) ;
#47238 = CARTESIAN_POINT ( 'NONE',  ( -1.771278280434267272, -193.5000000000000000, -115.9455772817710226 ) ) ;
#47239 = CARTESIAN_POINT ( 'NONE',  ( 24.15597040328004752, -193.5000000000000000, -101.7307360698543874 ) ) ;
#47240 = VERTEX_POINT ( 'NONE', #1057 ) ;
#47241 = LINE ( 'NONE', #27511, #25860 ) ;
#47242 = ORIENTED_EDGE ( 'NONE', *, *, #49043, .F. ) ;
#47243 = VECTOR ( 'NONE', #17025, 1000.000000000000114 ) ;
#47244 = VECTOR ( 'NONE', #26678, 1000.000000000000227 ) ;
#47245 = EDGE_CURVE ( 'NONE', #3854, #9931, #25500, .T. ) ;
#47246 = ORIENTED_EDGE ( 'NONE', *, *, #51636, .F. ) ;
#47247 = DIRECTION ( 'NONE',  ( 0.000000000000000000, -1.000000000000000000, 0.000000000000000000 ) ) ;
#47248 = AXIS2_PLACEMENT_3D ( 'NONE', #25913, #34316, #25398 ) ;
#47250 = VECTOR ( 'NONE', #33739, 999.9999999999998863 ) ;
#47249 = CARTESIAN_POINT ( 'NONE',  ( -339.1964088526558498, -109.8658467157473666, -57.40522506028092664 ) ) ;
#47251 = VERTEX_POINT ( 'NONE', #37324 ) ;
#47252 = LINE ( 'NONE', #46992, #29905 ) ;
#47253 = CARTESIAN_POINT ( 'NONE',  ( -172.1767935149754294, -177.1207230881787780, 8.665274887906315726 ) ) ;
#47254 = LINE ( 'NONE', #6265, #12044 ) ;
#47255 = CARTESIAN_POINT ( 'NONE',  ( 55.91309001144629320, -193.5000000000000000, 68.75510947788671956 ) ) ;
#47256 = AXIS2_PLACEMENT_3D ( 'NONE', #38327, #2343, #34637 ) ;
#47257 = ORIENTED_EDGE ( 'NONE', *, *, #12121, .T. ) ;
#47258 = CARTESIAN_POINT ( 'NONE',  ( 48.47907891923915003, -175.3837268820161057, 78.89300572996906169 ) ) ;
#47259 = CARTESIAN_POINT ( 'NONE',  ( -330.4913330509368166, -144.8891964568525452, -54.98865587491815177 ) ) ;
#47260 = DIRECTION ( 'NONE',  ( -0.000000000000000000, -0.3546048870425363986, -0.9350162426854146114 ) ) ;
#47261 = VERTEX_POINT ( 'NONE', #1323 ) ;
#47262 = CARTESIAN_POINT ( 'NONE',  ( 38.46761263173350187, -189.7472609257535510, 89.80681772907071547 ) ) ;
#47263 = AXIS2_PLACEMENT_3D ( 'NONE', #35652, #35390, #43285 ) ;
#47264 = FACE_OUTER_BOUND ( 'NONE', #24125, .T. ) ;
#47265 = ADVANCED_FACE ( 'NONE', ( #37598 ), #28647, .F. ) ;
#47266 = EDGE_LOOP ( 'NONE', ( #47720, #6904, #46663, #21424 ) ) ;
#47267 = EDGE_CURVE ( 'NONE', #38315, #46519, #47032, .T. ) ;
#47268 = DIRECTION ( 'NONE',  ( -0.000000000000000000, 1.000000000000000000, -0.000000000000000000 ) ) ;
#47269 = EDGE_LOOP ( 'NONE', ( #26975, #37341, #9691, #36334 ) ) ;
#47270 = AXIS2_PLACEMENT_3D ( 'NONE', #1953, #3252, #15333 ) ;
#47271 = DIRECTION ( 'NONE',  ( 1.000000000000000000, 0.000000000000000000, 0.000000000000000000 ) ) ;
#47272 = FACE_BOUND ( 'NONE', #44763, .T. ) ;
#47274 = ORIENTED_EDGE ( 'NONE', *, *, #45643, .T. ) ;
#47273 = LINE ( 'NONE', #11244, #31273 ) ;
#47276 = VECTOR ( 'NONE', #8398, 1000.000000000000114 ) ;
#47275 = LINE ( 'NONE', #23357, #49577 ) ;
#47277 = AXIS2_PLACEMENT_3D ( 'NONE', #50625, #23019, #46954 ) ;
#47278 = ORIENTED_EDGE ( 'NONE', *, *, #4364, .T. ) ;
#47279 = VERTEX_POINT ( 'NONE', #22328 ) ;
#47280 = DIRECTION ( 'NONE',  ( 1.000000000000000000, -0.000000000000000000, -0.000000000000000000 ) ) ;
#47281 = AXIS2_PLACEMENT_3D ( 'NONE', #14235, #41550, #13707 ) ;
#47282 = ORIENTED_EDGE ( 'NONE', *, *, #30773, .F. ) ;
#47283 = PRODUCT_DEFINITION ( 'UNKNOWN', '', #30954, #11138 ) ;
#47284 = DIRECTION ( 'NONE',  ( 0.000000000000000000, 1.000000000000000000, -0.000000000000000000 ) ) ;
#47285 = VECTOR ( 'NONE', #3305, 1000.000000000000114 ) ;
#47286 = EDGE_CURVE ( 'NONE', #28978, #3704, #18029, .T. ) ;
#47287 = FACE_OUTER_BOUND ( 'NONE', #46455, .T. ) ;
#47288 = ORIENTED_EDGE ( 'NONE', *, *, #36863, .F. ) ;
#47291 = ORIENTED_EDGE ( 'NONE', *, *, #35933, .F. ) ;
#47290 = CARTESIAN_POINT ( 'NONE',  ( -49.32472275501067571, -193.5000000000000000, -0.5338233779647935107 ) ) ;
#47289 = PLANE ( 'NONE',  #36763 ) ;
#47292 = CARTESIAN_POINT ( 'NONE',  ( -339.1964088526558498, -115.8919814278871598, -58.50955523165758621 ) ) ;
#47293 = ORIENTED_EDGE ( 'NONE', *, *, #47495, .T. ) ;
#47294 = LINE ( 'NONE', #24158, #48260 ) ;
#47295 = CIRCLE ( 'NONE', #27126, 60.00000000000000000 ) ;
#47296 = VERTEX_POINT ( 'NONE', #18139 ) ;
#47297 = DIRECTION ( 'NONE',  ( -0.000000000000000000, 1.000000000000000000, -0.000000000000000000 ) ) ;
#47298 = EDGE_LOOP ( 'NONE', ( #18465, #21013, #15685, #10371 ) ) ;
#47300 = DIRECTION ( 'NONE',  ( 0.000000000000000000, -0.3546048870425300148, 0.9350162426854169428 ) ) ;
#47299 = DIRECTION ( 'NONE',  ( -0.8124868780056783146, 0.000000000000000000, -0.5829794791144762289 ) ) ;
#47301 = ORIENTED_EDGE ( 'NONE', *, *, #48027, .T. ) ;
#47302 = VECTOR ( 'NONE', #18953, 1000.000000000000000 ) ;
#47303 = LINE ( 'NONE', #47562, #41625 ) ;
#47304 = VERTEX_POINT ( 'NONE', #30987 ) ;
#47305 = DIRECTION ( 'NONE',  ( 1.000000000000000000, -0.000000000000000000, -0.000000000000000000 ) ) ;
#47306 = DIRECTION ( 'NONE',  ( -0.000000000000000000, 1.000000000000000000, -0.000000000000000000 ) ) ;
#47307 = EDGE_LOOP ( 'NONE', ( #51943, #36823, #27590, #47116 ) ) ;
#47308 = DIRECTION ( 'NONE',  ( -1.000000000000000000, -0.000000000000000000, 0.000000000000000000 ) ) ;
#47309 = CARTESIAN_POINT ( 'NONE',  ( -336.3521761649654422, -123.5000000000000284, 0.000000000000000000 ) ) ;
#47310 = LINE ( 'NONE', #34181, #31596 ) ;
#47311 = PLANE ( 'NONE',  #25714 ) ;
#47312 = EDGE_LOOP ( 'NONE', ( #27598, #40610, #9016, #35677 ) ) ;
#47313 = DIRECTION ( 'NONE',  ( 1.000000000000000000, 0.000000000000000000, 0.000000000000000000 ) ) ;
#47314 = VECTOR ( 'NONE', #6646, 1000.000000000000000 ) ;
#47315 = DIRECTION ( 'NONE',  ( 0.000000000000000000, -1.000000000000000000, 0.000000000000000000 ) ) ;
#47316 = CARTESIAN_POINT ( 'NONE',  ( -48.47912675150885065, -177.1207230881787780, 6.938893903907228378E-15 ) ) ;
#47317 = LINE ( 'NONE', #3668, #2766 ) ;
#47318 = ORIENTED_EDGE ( 'NONE', *, *, #27276, .F. ) ;
#47319 = VECTOR ( 'NONE', #39334, 1000.000000000000000 ) ;
#47320 = CARTESIAN_POINT ( 'NONE',  ( -48.47912675150885065, -175.3837268820161057, 6.938893903907228378E-15 ) ) ;
#47321 = CARTESIAN_POINT ( 'NONE',  ( -339.1964088526558498, -74.65991953890826949, 33.10432812419072945 ) ) ;
#47322 = FACE_OUTER_BOUND ( 'NONE', #36122, .T. ) ;
#47324 = ORIENTED_EDGE ( 'NONE', *, *, #27305, .T. ) ;
#47323 = LINE ( 'NONE', #19205, #22413 ) ;
#47325 = EDGE_CURVE ( 'NONE', #5817, #1492, #7081, .T. ) ;
#47326 = CARTESIAN_POINT ( 'NONE',  ( 46.00000000000000711, 20.00000000000000000, 46.00000000000000000 ) ) ;
#47327 = CARTESIAN_POINT ( 'NONE',  ( -157.5429198988176438, -189.7472609257535510, 61.07445476073478829 ) ) ;
#47328 = CARTESIAN_POINT ( 'NONE',  ( -48.47912675150885065, -189.7472609257535510, 125.0000000000000000 ) ) ;
#47329 = DIRECTION ( 'NONE',  ( 0.000000000000000000, 0.000000000000000000, 1.000000000000000000 ) ) ;
#47330 = FACE_OUTER_BOUND ( 'NONE', #32420, .T. ) ;
#47331 = CIRCLE ( 'NONE', #38908, 125.0000000000000000 ) ;
#47332 = ORIENTED_EDGE ( 'NONE', *, *, #35536, .F. ) ;
#47333 = CARTESIAN_POINT ( 'NONE',  ( -305.0000000000000568, -138.3439121830097633, -58.13482838284718923 ) ) ;
#47334 = AXIS2_PLACEMENT_3D ( 'NONE', #15712, #28542, #20152 ) ;
#47335 = ORIENTED_EDGE ( 'NONE', *, *, #45131, .F. ) ;
#47336 = VERTEX_POINT ( 'NONE', #38360 ) ;
#47337 = EDGE_LOOP ( 'NONE', ( #19613, #17833, #47533, #48433 ) ) ;
#47338 = EDGE_CURVE ( 'NONE', #16187, #1636, #38614, .T. ) ;
#47339 = DIRECTION ( 'NONE',  ( 1.000000000000000000, 0.000000000000000000, 0.000000000000000000 ) ) ;
#47340 = CARTESIAN_POINT ( 'NONE',  ( -66.46933728415694986, -183.6283474603465606, 122.6885491605231380 ) ) ;
#47342 = EDGE_LOOP ( 'NONE', ( #21449, #4670, #50851, #6230 ) ) ;
#47341 = VECTOR ( 'NONE', #48583, 1000.000000000000114 ) ;
#47343 = DIRECTION ( 'NONE',  ( -8.718379230999705894E-17, -0.9350162426854107256, 0.3546048870425463906 ) ) ;
#47344 = CARTESIAN_POINT ( 'NONE',  ( -332.3517673607765914, -146.2946350401741711, -55.50139289590186564 ) ) ;
#47347 = ORIENTED_EDGE ( 'NONE', *, *, #5444, .F. ) ;
#47346 = CARTESIAN_POINT ( 'NONE',  ( -48.47912675150885065, -177.1207230881787780, 6.938893903907228378E-15 ) ) ;
#47345 = DIRECTION ( 'NONE',  ( 0.000000000000000000, -1.000000000000000000, 0.000000000000000000 ) ) ;
#47348 = CARTESIAN_POINT ( 'NONE',  ( -48.47912675150885065, -189.7472609257535510, 6.938893903907228378E-15 ) ) ;
#47349 = ORIENTED_EDGE ( 'NONE', *, *, #14510, .T. ) ;
#47350 = CARTESIAN_POINT ( 'NONE',  ( 50.70030191143631271, -193.5000000000000000, -76.08180419845318454 ) ) ;
#47351 = EDGE_LOOP ( 'NONE', ( #16620, #20551 ) ) ;
#47352 = DIRECTION ( 'NONE',  ( 0.000000000000000000, 0.000000000000000000, -1.000000000000000000 ) ) ;
#47353 = LINE ( 'NONE', #51300, #15428 ) ;
#47355 = CARTESIAN_POINT ( 'NONE',  ( 9.518239912201957864, -213.5000000000000000, -110.7307791902283043 ) ) ;
#47354 = FACE_OUTER_BOUND ( 'NONE', #35638, .T. ) ;
#47356 = ORIENTED_EDGE ( 'NONE', *, *, #23553, .T. ) ;
#47357 = PLANE ( 'NONE',  #20622 ) ;
#47358 = VERTEX_POINT ( 'NONE', #42560 ) ;
#47359 = DIRECTION ( 'NONE',  ( -0.9564009842765264224, 0.000000000000000000, 0.2920567706369628924 ) ) ;
#47360 = ORIENTED_EDGE ( 'NONE', *, *, #32929, .F. ) ;
#47361 = PLANE ( 'NONE',  #19864 ) ;
#47362 = AXIS2_PLACEMENT_3D ( 'NONE', #25824, #1116, #5609 ) ;
#47363 = CARTESIAN_POINT ( 'NONE',  ( -339.1964088526558498, -137.1341532842523065, 57.40522506028101901 ) ) ;
#47364 = VECTOR ( 'NONE', #8127, 1000.000000000000000 ) ;
#47365 = EDGE_CURVE ( 'NONE', #13363, #18053, #30469, .T. ) ;
#47366 = VERTEX_POINT ( 'NONE', #14205 ) ;
#47367 = CARTESIAN_POINT ( 'NONE',  ( -330.4913330509368166, -123.9999999999993747, 59.00000000000002132 ) ) ;
#47369 = AXIS2_PLACEMENT_3D ( 'NONE', #44003, #4074, #20092 ) ;
#47368 = FACE_OUTER_BOUND ( 'NONE', #23728, .T. ) ;
#47370 = EDGE_CURVE ( 'NONE', #8060, #4209, #34668, .T. ) ;
#47371 = PLANE ( 'NONE',  #44215 ) ;
#47372 = ORIENTED_EDGE ( 'NONE', *, *, #47987, .F. ) ;
#47373 = CARTESIAN_POINT ( 'NONE',  ( -339.1964088526558498, -123.5000000000000284, 0.000000000000000000 ) ) ;
#47374 = CARTESIAN_POINT ( 'NONE',  ( -339.1964088526558498, -130.1153096980144426, 58.63009191191295599 ) ) ;
#47375 = DIRECTION ( 'NONE',  ( 0.000000000000000000, 0.000000000000000000, -1.000000000000000000 ) ) ;
#47376 = CARTESIAN_POINT ( 'NONE',  ( -154.6193097927903182, -175.3837268820161057, -66.02470404298122730 ) ) ;
#47377 = FACE_OUTER_BOUND ( 'NONE', #32707, .T. ) ;
#47378 = EDGE_CURVE ( 'NONE', #13340, #48355, #4590, .T. ) ;
#47379 = VECTOR ( 'NONE', #9344, 1000.000000000000000 ) ;
#47380 = EDGE_CURVE ( 'NONE', #26396, #18665, #30222, .T. ) ;
#47381 = DIRECTION ( 'NONE',  ( 0.000000000000000000, -1.000000000000000000, 0.000000000000000000 ) ) ;
#47382 = ADVANCED_FACE ( 'NONE', ( #6308 ), #42042, .F. ) ;
#47383 = DIRECTION ( 'NONE',  ( -0.8757349421956345248, 0.000000000000000000, -0.4827922027307490205 ) ) ;
#47384 = DIRECTION ( 'NONE',  ( 0.000000000000000000, -1.000000000000000000, 0.000000000000000000 ) ) ;
#47386 = VERTEX_POINT ( 'NONE', #22072 ) ;
#47385 = LINE ( 'NONE', #43447, #35401 ) ;
#47387 = EDGE_LOOP ( 'NONE', ( #41407, #28887, #9218, #29566 ) ) ;
#47388 = CARTESIAN_POINT ( 'NONE',  ( -48.47912675150885065, -183.6283474603465606, 6.938893903907228378E-15 ) ) ;
#47389 = CARTESIAN_POINT ( 'NONE',  ( -172.0839188101925004, -175.3837268820161057, -18.62405380494756812 ) ) ;
#47390 = ORIENTED_EDGE ( 'NONE', *, *, #7681, .F. ) ;
#47391 = EDGE_LOOP ( 'NONE', ( #18412, #30996, #15274, #5517 ) ) ;
#47392 = LINE ( 'NONE', #11120, #12207 ) ;
#47393 = ORIENTED_EDGE ( 'NONE', *, *, #51670, .T. ) ;
#47394 = EDGE_CURVE ( 'NONE', #12850, #21974, #34419, .T. ) ;
#47395 = CARTESIAN_POINT ( 'NONE',  ( -332.3517673607765914, -88.64083255475578937, 47.62880233550460218 ) ) ;
#47396 = CARTESIAN_POINT ( 'NONE',  ( -1.079983486989452192E-15, 45.00000000000000000, 0.000000000000000000 ) ) ;
#47397 = AXIS2_PLACEMENT_3D ( 'NONE', #1598, #45740, #10003 ) ;
#47398 = CIRCLE ( 'NONE', #2069, 125.0000000000000000 ) ;
#47399 = PLANE ( 'NONE',  #33654 ) ;
#47400 = CARTESIAN_POINT ( 'NONE',  ( 7.991501969728822985, -175.3837268820161057, 110.3950557015152754 ) ) ;
#47401 = EDGE_LOOP ( 'NONE', ( #3361, #50535, #10404, #35071 ) ) ;
#47402 = ORIENTED_EDGE ( 'NONE', *, *, #10225, .T. ) ;
#47403 = AXIS2_PLACEMENT_3D ( 'NONE', #22687, #10338, #50552 ) ;
#47404 = VERTEX_POINT ( 'NONE', #26264 ) ;
#47405 = FACE_OUTER_BOUND ( 'NONE', #21181, .T. ) ;
#47406 = DIRECTION ( 'NONE',  ( 0.000000000000000000, -1.000000000000000000, 0.000000000000000000 ) ) ;
#47407 = CARTESIAN_POINT ( 'NONE',  ( -330.4913330509368166, -75.22798428563987727, -33.92731199008506593 ) ) ;
#47408 = PLANE ( 'NONE',  #12997 ) ;
#47409 = ORIENTED_EDGE ( 'NONE', *, *, #50203, .F. ) ;
#47410 = UNCERTAINTY_MEASURE_WITH_UNIT (LENGTH_MEASURE( 1.000000000000000082E-05 ), #36292, 'distance_accuracy_value', 'NONE');
#47411 = AXIS2_PLACEMENT_3D ( 'NONE', #21095, #37119, #25302 ) ;
#47412 = DIRECTION ( 'NONE',  ( 1.000000000000000000, -0.000000000000000000, 0.000000000000000000 ) ) ;
#47413 = PLANE ( 'NONE',  #34092 ) ;
#47414 = VERTEX_POINT ( 'NONE', #10763 ) ;
#47415 = ORIENTED_EDGE ( 'NONE', *, *, #29856, .F. ) ;
#47416 = CARTESIAN_POINT ( 'NONE',  ( -62.43888699632653783, -193.5000000000000000, 124.2180546213279371 ) ) ;
#47417 = LINE ( 'NONE', #38229, #30846 ) ;
#47418 = ORIENTED_EDGE ( 'NONE', *, *, #20678, .F. ) ;
#47419 = DIRECTION ( 'NONE',  ( 0.000000000000000000, 0.000000000000000000, 1.000000000000000000 ) ) ;
#47420 = DIRECTION ( 'NONE',  ( 0.000000000000000000, -1.000000000000000000, 0.000000000000000000 ) ) ;
#47421 = EDGE_CURVE ( 'NONE', #34513, #1466, #35642, .T. ) ;
#47422 = EDGE_CURVE ( 'NONE', #50178, #43983, #37300, .T. ) ;
#47423 = DIRECTION ( 'NONE',  ( -0.000000000000000000, -0.8854560256532062468, 0.4647231720437755564 ) ) ;
#47424 = ORIENTED_EDGE ( 'NONE', *, *, #24215, .T. ) ;
#47425 = DIRECTION ( 'NONE',  ( -0.000000000000000000, 1.000000000000000000, -0.000000000000000000 ) ) ;
#47426 = ORIENTED_EDGE ( 'NONE', *, *, #33191, .F. ) ;
#47427 = LINE ( 'NONE', #31385, #32980 ) ;
#47428 = FACE_BOUND ( 'NONE', #25448, .T. ) ;
#47429 = VECTOR ( 'NONE', #22159, 1000.000000000000000 ) ;
#47430 = LINE ( 'NONE', #31911, #13491 ) ;
#47431 = ORIENTED_EDGE ( 'NONE', *, *, #17913, .T. ) ;
#47432 = AXIS2_PLACEMENT_3D ( 'NONE', #45952, #35073, #31123 ) ;
#47433 = AXIS2_PLACEMENT_3D ( 'NONE', #13763, #12526, #10333 ) ;
#47434 = PLANE ( 'NONE',  #39097 ) ;
#47435 = CARTESIAN_POINT ( 'NONE',  ( 46.00000000000000711, 20.00000000000000000, -46.00000000000000000 ) ) ;
#47436 = DIRECTION ( 'NONE',  ( 0.7378332790417239107, 0.000000000000000000, 0.6749830015182142207 ) ) ;
#47437 = EDGE_CURVE ( 'NONE', #19237, #47120, #26524, .T. ) ;
#47438 = CARTESIAN_POINT ( 'NONE',  ( 25.43954814678888710, -193.5000000000000000, 100.8019320314832754 ) ) ;
#47439 = VECTOR ( 'NONE', #19335, 1000.000000000000114 ) ;
#47440 = EDGE_CURVE ( 'NONE', #40906, #39314, #38867, .T. ) ;
#47441 = PLANE ( 'NONE',  #30323 ) ;
#47442 = ORIENTED_EDGE ( 'NONE', *, *, #8551, .T. ) ;
#47443 = EDGE_LOOP ( 'NONE', ( #7591, #28027, #46438, #44921 ) ) ;
#47444 = EDGE_CURVE ( 'NONE', #18213, #36857, #7138, .T. ) ;
#47445 = AXIS2_PLACEMENT_3D ( 'NONE', #2303, #43536, #30652 ) ;
#47446 = LINE ( 'NONE', #50879, #28132 ) ;
#47448 = VERTEX_POINT ( 'NONE', #3136 ) ;
#47447 = FACE_OUTER_BOUND ( 'NONE', #50382, .T. ) ;
#47449 = CIRCLE ( 'NONE', #12994, 60.00000000000000000 ) ;
#47450 = EDGE_CURVE ( 'NONE', #35955, #44388, #16371, .T. ) ;
#47451 = ORIENTED_EDGE ( 'NONE', *, *, #46495, .F. ) ;
#47452 = CARTESIAN_POINT ( 'NONE',  ( -52.47502265695602119, -193.5000000000000000, -124.9361149384469485 ) ) ;
#47453 = AXIS2_PLACEMENT_3D ( 'NONE', #39441, #16067, #3442 ) ;
#47454 = AXIS2_PLACEMENT_3D ( 'NONE', #5537, #49933, #21562 ) ;
#47455 = LINE ( 'NONE', #50372, #39378 ) ;
#47456 = EDGE_LOOP ( 'NONE', ( #9840, #48213, #51156, #25823 ) ) ;
#47457 = DIRECTION ( 'NONE',  ( -0.000000000000000000, 1.000000000000000000, -0.000000000000000000 ) ) ;
#47458 = LINE ( 'NONE', #13208, #47206 ) ;
#47459 = ORIENTED_EDGE ( 'NONE', *, *, #18840, .F. ) ;
#47460 = CARTESIAN_POINT ( 'NONE',  ( -47.47956591500005885, -193.5000000000000000, 0.02963332782257025594 ) ) ;
#47461 = CARTESIAN_POINT ( 'NONE',  ( -330.4913330509368166, -175.9742670995615015, -26.97593913775547136 ) ) ;
#47462 = LINE ( 'NONE', #4346, #31607 ) ;
#47463 = ORIENTED_EDGE ( 'NONE', *, *, #4774, .F. ) ;
#47464 = ORIENTED_EDGE ( 'NONE', *, *, #15115, .T. ) ;
#47465 = ORIENTED_EDGE ( 'NONE', *, *, #9538, .T. ) ;
#47466 = CARTESIAN_POINT ( 'NONE',  ( -46.00000000000000711, 20.00000000000000000, 8.673617379884035472E-15 ) ) ;
#47467 = CARTESIAN_POINT ( 'NONE',  ( -54.99637373343401237, -189.7472609257535510, 123.8286356280830773 ) ) ;
#47468 = VECTOR ( 'NONE', #16340, 1000.000000000000000 ) ;
#47469 = PLANE ( 'NONE',  #51168 ) ;
#47470 = AXIS2_PLACEMENT_3D ( 'NONE', #51307, #23450, #51065 ) ;
#47471 = FACE_OUTER_BOUND ( 'NONE', #44117, .T. ) ;
#47472 = FACE_OUTER_BOUND ( 'NONE', #45673, .T. ) ;
#47473 = VERTEX_POINT ( 'NONE', #33894 ) ;
#47474 = AXIS2_PLACEMENT_3D ( 'NONE', #43373, #27061, #30497 ) ;
#47475 = CARTESIAN_POINT ( 'NONE',  ( -12.42681898335384894, -193.5000000000000000, 118.6432945265039365 ) ) ;
#47476 = ADVANCED_FACE ( 'NONE', ( #13938 ), #46015, .T. ) ;
#47477 = VERTEX_POINT ( 'NONE', #35972 ) ;
#47478 =( REPRESENTATION_RELATIONSHIP ('NONE','NONE', #4578, #33116 ) REPRESENTATION_RELATIONSHIP_WITH_TRANSFORMATION ( #49388 )SHAPE_REPRESENTATION_RELATIONSHIP( ) );
#47480 = ORIENTED_EDGE ( 'NONE', *, *, #44635, .T. ) ;
#47479 = DIRECTION ( 'NONE',  ( 0.000000000000000000, 1.000000000000000000, 0.000000000000000000 ) ) ;
#47481 = ORIENTED_EDGE ( 'NONE', *, *, #13450, .F. ) ;
#47482 = LINE ( 'NONE', #50653, #10699 ) ;
#47483 = VECTOR ( 'NONE', #42566, 1000.000000000000000 ) ;
#47484 = PLANE ( 'NONE',  #35025 ) ;
#47485 = VECTOR ( 'NONE', #49580, 1000.000000000000000 ) ;
#47486 = ADVANCED_FACE ( 'NONE', ( #43340 ), #31774, .T. ) ;
#47487 = CARTESIAN_POINT ( 'NONE',  ( 1.734723475976807094E-15, 20.00000000000000000, 41.00000000000000711 ) ) ;
#47488 = ADVANCED_FACE ( 'NONE', ( #7351 ), #3918, .F. ) ;
#47489 = EDGE_CURVE ( 'NONE', #9353, #23327, #1284, .T. ) ;
#47490 = DIRECTION ( 'NONE',  ( 0.1768902751225733261, 0.000000000000000000, -0.9842305779475966077 ) ) ;
#47491 = ORIENTED_EDGE ( 'NONE', *, *, #43319, .F. ) ;
#47492 = DIRECTION ( 'NONE',  ( 0.000000000000000000, -1.000000000000000000, 0.000000000000000000 ) ) ;
#47493 = AXIS2_PLACEMENT_3D ( 'NONE', #15487, #31497, #11534 ) ;
#47494 = ORIENTED_EDGE ( 'NONE', *, *, #50203, .T. ) ;
#47495 = EDGE_CURVE ( 'NONE', #6148, #2027, #19672, .T. ) ;
#47496 = CIRCLE ( 'NONE', #43282, 125.0000000000000000 ) ;
#47497 = ORIENTED_EDGE ( 'NONE', *, *, #32004, .T. ) ;
#47498 = LINE ( 'NONE', #28286, #40512 ) ;
#47499 = LINE ( 'NONE', #40553, #9651 ) ;
#47500 = ADVANCED_FACE ( 'NONE', ( #39381 ), #23612, .T. ) ;
#47501 = FACE_OUTER_BOUND ( 'NONE', #39649, .T. ) ;
#47502 = PLANE ( 'NONE',  #1285 ) ;
#47503 = LINE ( 'NONE', #22563, #14588 ) ;
#47504 = LINE ( 'NONE', #26998, #45556 ) ;
#47505 = EDGE_CURVE ( 'NONE', #39776, #20552, #47294, .T. ) ;
#47506 = VERTEX_POINT ( 'NONE', #23375 ) ;
#47507 = CARTESIAN_POINT ( 'NONE',  ( 59.29945538372742675, -183.6283474603465606, 63.31490529818493940 ) ) ;
#47508 = LINE ( 'NONE', #43559, #27382 ) ;
#47509 = EDGE_CURVE ( 'NONE', #36297, #47114, #19170, .T. ) ;
#47510 = DIRECTION ( 'NONE',  ( 0.000000000000000000, -0.4647231720437573488, 0.8854560256532157947 ) ) ;
#47511 = ORIENTED_EDGE ( 'NONE', *, *, #25402, .T. ) ;
#47512 = CIRCLE ( 'NONE', #4701, 125.0000000000000000 ) ;
#47513 = ADVANCED_FACE ( 'NONE', ( #19415 ), #40166, .F. ) ;
#47514 = DIRECTION ( 'NONE',  ( 0.000000000000000000, 0.000000000000000000, -1.000000000000000000 ) ) ;
#47515 = VECTOR ( 'NONE', #45497, 999.9999999999998863 ) ;
#47516 = VECTOR ( 'NONE', #32296, 999.9999999999998863 ) ;
#47517 = CARTESIAN_POINT ( 'NONE',  ( -336.3521761649654422, -160.6539403396202772, 45.90766452162722544 ) ) ;
#47518 = EDGE_CURVE ( 'NONE', #24853, #33118, #19943, .T. ) ;
#47519 = ORIENTED_EDGE ( 'NONE', *, *, #127, .T. ) ;
#47520 = DIRECTION ( 'NONE',  ( -0.000000000000000000, 1.000000000000000000, -0.000000000000000000 ) ) ;
#47521 = VERTEX_POINT ( 'NONE', #216 ) ;
#47522 = EDGE_CURVE ( 'NONE', #32234, #32749, #48321, .T. ) ;
#47523 = DIRECTION ( 'NONE',  ( 0.000000000000000000, 0.000000000000000000, 1.000000000000000000 ) ) ;
#47524 = FACE_BOUND ( 'NONE', #35194, .T. ) ;
#47525 = VECTOR ( 'NONE', #25594, 1000.000000000000000 ) ;
#47527 = ORIENTED_EDGE ( 'NONE', *, *, #24142, .F. ) ;
#47526 = DIRECTION ( 'NONE',  ( -0.000000000000000000, 1.000000000000000000, -0.000000000000000000 ) ) ;
#47528 = VECTOR ( 'NONE', #30304, 1000.000000000000000 ) ;
#47529 = CIRCLE ( 'NONE', #31685, 125.0000000000000568 ) ;
#47530 = AXIS2_PLACEMENT_3D ( 'NONE', #30233, #10773, #17646 ) ;
#47531 = DIRECTION ( 'NONE',  ( -0.9982437317643214625, 0.000000000000000000, -0.05924062789371441901 ) ) ;
#47532 = EDGE_CURVE ( 'NONE', #23663, #28688, #51489, .T. ) ;
#47533 = ORIENTED_EDGE ( 'NONE', *, *, #48210, .F. ) ;
#47534 = EDGE_CURVE ( 'NONE', #10132, #32136, #13021, .T. ) ;
#47535 = ORIENTED_EDGE ( 'NONE', *, *, #13800, .T. ) ;
#47536 = AXIS2_PLACEMENT_3D ( 'NONE', #870, #48715, #44249 ) ;
#47537 = DIRECTION ( 'NONE',  ( 0.5085311186492094127, 0.000000000000000000, 0.8610436117673619938 ) ) ;
#47538 = VERTEX_POINT ( 'NONE', #51754 ) ;
#47539 = FACE_OUTER_BOUND ( 'NONE', #43545, .T. ) ;
#47540 = CARTESIAN_POINT ( 'NONE',  ( 0.000000000000000000, -172.0560480877254861, 33.51582005713859758 ) ) ;
#47541 = DIRECTION ( 'NONE',  ( 0.8757349421956345248, 0.000000000000000000, 0.4827922027307490205 ) ) ;
#47542 = ORIENTED_EDGE ( 'NONE', *, *, #51029, .T. ) ;
#47545 = EDGE_LOOP ( 'NONE', ( #40557, #28533, #8236, #37848 ) ) ;
#47544 = CARTESIAN_POINT ( 'NONE',  ( -339.1964088526558498, -178.4886558749184076, -21.38919645685194837 ) ) ;
#47543 = DIRECTION ( 'NONE',  ( -0.000000000000000000, 1.000000000000000000, -0.000000000000000000 ) ) ;
#47546 = VECTOR ( 'NONE', #8841, 1000.000000000000000 ) ;
#47547 = CIRCLE ( 'NONE', #28204, 125.0000000000000000 ) ;
#47548 = DIRECTION ( 'NONE',  ( 0.000000000000000000, 0.000000000000000000, 1.000000000000000000 ) ) ;
#47549 = ORIENTED_EDGE ( 'NONE', *, *, #861, .F. ) ;
#47550 = DIRECTION ( 'NONE',  ( -0.2920567706369628924, 0.000000000000000000, -0.9564009842765264224 ) ) ;
#47551 = ORIENTED_EDGE ( 'NONE', *, *, #2231, .T. ) ;
#47552 = VECTOR ( 'NONE', #8443, 1000.000000000000000 ) ;
#47553 = ADVANCED_FACE ( 'NONE', ( #51238 ), #47812, .T. ) ;
#47554 = EDGE_CURVE ( 'NONE', #2758, #45184, #43221, .T. ) ;
#47555 = CARTESIAN_POINT ( 'NONE',  ( 42.10477485469927927, -183.6283474603465606, 86.13684908212515268 ) ) ;
#47556 = VERTEX_POINT ( 'NONE', #40410 ) ;
#47558 = CARTESIAN_POINT ( 'NONE',  ( -336.3521761649654422, -182.5000000000000568, 2.632288850093980503 ) ) ;
#47557 = DIRECTION ( 'NONE',  ( -0.000000000000000000, 1.000000000000000000, -0.000000000000000000 ) ) ;
#47559 = ORIENTED_EDGE ( 'NONE', *, *, #22482, .F. ) ;
#47560 = ADVANCED_FACE ( 'NONE', ( #31499 ), #15228, .F. ) ;
#47561 = EDGE_CURVE ( 'NONE', #26366, #4036, #12571, .T. ) ;
#47562 = CARTESIAN_POINT ( 'NONE',  ( -140.5933766095837427, -175.3837268820161057, -84.49831343337065448 ) ) ;
#47563 = ORIENTED_EDGE ( 'NONE', *, *, #3741, .T. ) ;
#47564 = FACE_OUTER_BOUND ( 'NONE', #9480, .T. ) ;
#47565 = CIRCLE ( 'NONE', #2242, 125.0000000000000000 ) ;
#47566 = DIRECTION ( 'NONE',  ( 0.000000000000000000, 1.000000000000000000, 0.000000000000000000 ) ) ;
#47567 = AXIS2_PLACEMENT_3D ( 'NONE', #39143, #46530, #3153 ) ;
#47568 = DIRECTION ( 'NONE',  ( 0.000000000000000000, 0.000000000000000000, 1.000000000000000000 ) ) ;
#47569 = CARTESIAN_POINT ( 'NONE',  ( -47.51449116960048968, -189.7472609257535510, -0.2635871660690578544 ) ) ;
#47570 = DIRECTION ( 'NONE',  ( 0.000000000000000000, 1.000000000000000000, -0.000000000000000000 ) ) ;
#47571 = VECTOR ( 'NONE', #7305, 1000.000000000000000 ) ;
#47572 = AXIS2_PLACEMENT_3D ( 'NONE', #34114, #41990, #17585 ) ;
#47573 = CARTESIAN_POINT ( 'NONE',  ( -98.71382891444399377, -193.5000000000000000, -114.4616734920523555 ) ) ;
#47574 = VERTEX_POINT ( 'NONE', #17311 ) ;
#47575 = VECTOR ( 'NONE', #15604, 1000.000000000000000 ) ;
#47576 = LINE ( 'NONE', #43866, #17136 ) ;
#47577 = DIRECTION ( 'NONE',  ( -0.000000000000000000, 1.000000000000000000, -0.000000000000000000 ) ) ;
#47578 = CIRCLE ( 'NONE', #32444, 125.0000000000000000 ) ;
#47579 = LINE ( 'NONE', #11562, #41366 ) ;
#47580 = VERTEX_POINT ( 'NONE', #1254 ) ;
#47581 = DIRECTION ( 'NONE',  ( -0.000000000000000000, 0.5680647467311656929, 0.8229838658936495799 ) ) ;
#47582 = ADVANCED_FACE ( 'NONE', ( #29631 ), #48595, .T. ) ;
#47583 = PLANE ( 'NONE',  #18554 ) ;
#47584 = LINE ( 'NONE', #3946, #9304 ) ;
#47586 = EDGE_LOOP ( 'NONE', ( #42954, #38196, #20785, #20933 ) ) ;
#47585 = CARTESIAN_POINT ( 'NONE',  ( -158.3442440847887269, -189.7472609257535510, -59.62093586438114556 ) ) ;
#47587 = VERTEX_POINT ( 'NONE', #13608 ) ;
#47588 = ORIENTED_EDGE ( 'NONE', *, *, #26340, .T. ) ;
#47589 = ADVANCED_FACE ( 'NONE', ( #4966 ), #33331, .T. ) ;
#47590 = VECTOR ( 'NONE', #15135, 1000.000000000000000 ) ;
#47591 = DIRECTION ( 'NONE',  ( 0.000000000000000000, -1.000000000000000000, -0.000000000000000000 ) ) ;
#47592 = VECTOR ( 'NONE', #51087, 1000.000000000000000 ) ;
#47593 = LINE ( 'NONE', #32053, #40447 ) ;
#47594 = LINE ( 'NONE', #44146, #29578 ) ;
#47595 = LINE ( 'NONE', #18439, #21196 ) ;
#47596 = VECTOR ( 'NONE', #2471, 1000.000000000000114 ) ;
#47597 = ORIENTED_EDGE ( 'NONE', *, *, #8864, .T. ) ;
#47598 = PLANE ( 'NONE',  #29370 ) ;
#47599 = EDGE_LOOP ( 'NONE', ( #39118, #30962, #42205, #49037 ) ) ;
#47600 = AXIS2_PLACEMENT_3D ( 'NONE', #21160, #37186, #45611 ) ;
#47601 = ORIENTED_EDGE ( 'NONE', *, *, #40903, .T. ) ;
#47602 = VECTOR ( 'NONE', #8233, 1000.000000000000000 ) ;
#47603 = ORIENTED_EDGE ( 'NONE', *, *, #18656, .T. ) ;
#47604 = FACE_OUTER_BOUND ( 'NONE', #31137, .T. ) ;
#47605 = VECTOR ( 'NONE', #48123, 1000.000000000000114 ) ;
#47606 = CIRCLE ( 'NONE', #15726, 125.0000000000000000 ) ;
#47608 = CIRCLE ( 'NONE', #9004, 125.0000000000000000 ) ;
#47607 = PLANE ( 'NONE',  #21986 ) ;
#47609 = ORIENTED_EDGE ( 'NONE', *, *, #35944, .T. ) ;
#47610 = AXIS2_PLACEMENT_3D ( 'NONE', #1842, #37327, #17885 ) ;
#47611 = DIRECTION ( 'NONE',  ( -1.000000000000000000, 0.000000000000000000, -0.000000000000000000 ) ) ;
#47612 = DIRECTION ( 'NONE',  ( 0.000000000000000000, -0.8229838658936596829, -0.5680647467311510379 ) ) ;
#47615 = ORIENTED_EDGE ( 'NONE', *, *, #51649, .F. ) ;
#47614 = DIRECTION ( 'NONE',  ( 1.000000000000000000, -8.151826190875865775E-17, 3.091579882402733311E-17 ) ) ;
#47613 = DIRECTION ( 'NONE',  ( -0.000000000000000000, 1.000000000000000000, 0.000000000000000000 ) ) ;
#47616 = LINE ( 'NONE', #12089, #18891 ) ;
#47617 = ORIENTED_EDGE ( 'NONE', *, *, #35796, .T. ) ;
#47618 = CARTESIAN_POINT ( 'NONE',  ( -339.1964088526558498, -150.4759391377552618, 52.47426709956155122 ) ) ;
#47619 = ORIENTED_EDGE ( 'NONE', *, *, #51858, .T. ) ;
#47620 = EDGE_CURVE ( 'NONE', #21250, #1126, #11322, .T. ) ;
#47621 = CARTESIAN_POINT ( 'NONE',  ( 63.31225588004632243, -183.6283474603465606, 55.92572546981597981 ) ) ;
#47622 = PLANE ( 'NONE',  #17119 ) ;
#47624 = CARTESIAN_POINT ( 'NONE',  ( -330.4913330509368166, -167.9936954712156023, -38.74998146212117689 ) ) ;
#47623 = PLANE ( 'NONE',  #10652 ) ;
#47625 = ORIENTED_EDGE ( 'NONE', *, *, #38496, .F. ) ;
#47626 = LINE ( 'NONE', #11610, #14787 ) ;
#47627 = DIRECTION ( 'NONE',  ( -0.000000000000000000, 0.4647231720437789981, 0.8854560256532044704 ) ) ;
#47628 = AXIS2_PLACEMENT_3D ( 'NONE', #25794, #42073, #21603 ) ;
#47629 = ORIENTED_EDGE ( 'NONE', *, *, #18815, .T. ) ;
#47630 = CARTESIAN_POINT ( 'NONE',  ( 18.49541618049842384, -183.6283474603465606, 105.5434062319798016 ) ) ;
#47631 = VECTOR ( 'NONE', #24763, 1000.000000000000227 ) ;
#47632 = DIRECTION ( 'NONE',  ( 0.000000000000000000, 0.000000000000000000, -1.000000000000000000 ) ) ;
#47633 = EDGE_LOOP ( 'NONE', ( #51506, #18217, #26164, #46391 ) ) ;
#47634 = CARTESIAN_POINT ( 'NONE',  ( -36.09284319799462537, -193.5000000000000000, 124.3848060646152618 ) ) ;
#47635 = PLANE ( 'NONE',  #35674 ) ;
#47636 = FACE_OUTER_BOUND ( 'NONE', #47298, .T. ) ;
#47637 = PRODUCT_RELATED_PRODUCT_CATEGORY ( 'part', '', ( #13844 ) ) ;
#47638 = ORIENTED_EDGE ( 'NONE', *, *, #20431, .F. ) ;
#47639 = LINE ( 'NONE', #20024, #9001 ) ;
#47640 = VERTEX_POINT ( 'NONE', #24655 ) ;
#47641 = VECTOR ( 'NONE', #48445, 1000.000000000000000 ) ;
#47642 = DIRECTION ( 'NONE',  ( 0.000000000000000000, -0.000000000000000000, 1.000000000000000000 ) ) ;
#47643 = AXIS2_PLACEMENT_3D ( 'NONE', #47346, #15541, #19470 ) ;
#47644 = CARTESIAN_POINT ( 'NONE',  ( 51.65665342072241373, -183.6283474603465606, 74.81861753132420745 ) ) ;
#47645 = ADVANCED_FACE ( 'NONE', ( #5484 ), #5225, .T. ) ;
#47646 = AXIS2_PLACEMENT_3D ( 'NONE', #15437, #47237, #19367 ) ;
#47647 = DIRECTION ( 'NONE',  ( 0.000000000000000000, -0.8660254037844354880, -0.5000000000000054401 ) ) ;
#47648 = CYLINDRICAL_SURFACE ( 'NONE', #2073, 125.0000000000000000 ) ;
#47649 = CARTESIAN_POINT ( 'NONE',  ( -332.3517673607765914, -132.3499116637027271, -59.34373651485605450 ) ) ;
#47650 = AXIS2_PLACEMENT_3D ( 'NONE', #47569, #31255, #34684 ) ;
#47652 = CIRCLE ( 'NONE', #3969, 60.00000000000000000 ) ;
#47651 = DIRECTION ( 'NONE',  ( 0.000000000000000000, -1.000000000000000000, 0.000000000000000000 ) ) ;
#47653 = CARTESIAN_POINT ( 'NONE',  ( -332.3517673607765914, -119.0014323656137947, -58.88711093124865670 ) ) ;
#47654 = CARTESIAN_POINT ( 'NONE',  ( -330.4913330509368166, -167.3305728129743102, 39.49849221029282376 ) ) ;
#47656 = ORIENTED_EDGE ( 'NONE', *, *, #36433, .F. ) ;
#47655 = DIRECTION ( 'NONE',  ( 0.000000000000000000, 1.000000000000000000, 0.000000000000000000 ) ) ;
#47657 = EDGE_LOOP ( 'NONE', ( #40922, #27855, #9907, #35636 ) ) ;
#47658 = DIRECTION ( 'NONE',  ( -1.000000000000000000, 0.000000000000000000, -0.000000000000000000 ) ) ;
#47659 = EDGE_CURVE ( 'NONE', #1035, #6177, #21245, .T. ) ;
#47660 = CARTESIAN_POINT ( 'NONE',  ( 71.35177504360963496, -193.5000000000000000, 31.88354567335082734 ) ) ;
#47661 = ORIENTED_EDGE ( 'NONE', *, *, #12101, .T. ) ;
#47662 = CIRCLE ( 'NONE', #49395, 124.9999999999999858 ) ;
#47663 = VECTOR ( 'NONE', #47818, 1000.000000000000114 ) ;
#47664 = EDGE_LOOP ( 'NONE', ( #51960, #30594, #5667, #4699 ) ) ;
#47665 = DIRECTION ( 'NONE',  ( 0.000000000000000000, -1.000000000000000000, 0.000000000000000000 ) ) ;
#47666 = ORIENTED_EDGE ( 'NONE', *, *, #9012, .T. ) ;
#47667 = CARTESIAN_POINT ( 'NONE',  ( 37.77106160267051393, -189.7472609257535510, 89.08931047202638354 ) ) ;
#47668 = DIRECTION ( 'NONE',  ( -0.000000000000000000, 0.8229838658936634577, 0.5680647467311457088 ) ) ;
#47669 = CIRCLE ( 'NONE', #2350, 125.0000000000000000 ) ;
#47670 = DIRECTION ( 'NONE',  ( 0.000000000000000000, -0.000000000000000000, -1.000000000000000000 ) ) ;
#47671 = LINE ( 'NONE', #23732, #12356 ) ;
#47672 = ORIENTED_EDGE ( 'NONE', *, *, #18012, .F. ) ;
#47673 = ORIENTED_EDGE ( 'NONE', *, *, #23706, .T. ) ;
#47674 = EDGE_LOOP ( 'NONE', ( #9105, #33536, #25444, #38134 ) ) ;
#47675 = EDGE_CURVE ( 'NONE', #15950, #33788, #25591, .T. ) ;
#47676 = DIRECTION ( 'NONE',  ( 0.000000000000000000, 0.000000000000000000, -1.000000000000000000 ) ) ;
#47677 = CARTESIAN_POINT ( 'NONE',  ( 0.000000000000000000, -63.50000000000000000, -20.00000000000000000 ) ) ;
#47678 = LINE ( 'NONE', #23742, #12316 ) ;
#47679 = CARTESIAN_POINT ( 'NONE',  ( -140.8230258362169707, -175.3837268820161057, 84.24728067916045404 ) ) ;
#47680 = DIRECTION ( 'NONE',  ( -0.000000000000000000, 1.000000000000000000, 0.000000000000000000 ) ) ;
#47681 = VERTEX_POINT ( 'NONE', #20719 ) ;
#47682 = CARTESIAN_POINT ( 'NONE',  ( -47.74129347246713451, -193.5000000000000000, 0.6749830015182212151 ) ) ;
#47683 = EDGE_CURVE ( 'NONE', #21742, #23268, #39010, .T. ) ;
#47684 = CARTESIAN_POINT ( 'NONE',  ( -167.6453766917639427, -177.1207230881787780, 37.74128873232411507 ) ) ;
#47685 = DIRECTION ( 'NONE',  ( 0.000000000000000000, 0.000000000000000000, -1.000000000000000000 ) ) ;
#47686 = VECTOR ( 'NONE', #7342, 1000.000000000000000 ) ;
#47687 = ORIENTED_EDGE ( 'NONE', *, *, #25960, .T. ) ;
#47688 = ORIENTED_EDGE ( 'NONE', *, *, #32331, .F. ) ;
#47689 = EDGE_CURVE ( 'NONE', #2646, #27986, #37264, .T. ) ;
#47690 = EDGE_LOOP ( 'NONE', ( #42823, #50709, #51306, #39083 ) ) ;
#47691 = LINE ( 'NONE', #50855, #410 ) ;
#47692 = FACE_OUTER_BOUND ( 'NONE', #31062, .T. ) ;
#47693 = VERTEX_POINT ( 'NONE', #36753 ) ;
#47694 = LINE ( 'NONE', #19052, #37583 ) ;
#47695 = CARTESIAN_POINT ( 'NONE',  ( -336.3521761649654422, -164.5945333327934463, -42.41660376256285048 ) ) ;
#47696 = DIRECTION ( 'NONE',  ( 0.02963332782256331357, 0.000000000000000000, -0.9995608365087942371 ) ) ;
#47697 = ORIENTED_EDGE ( 'NONE', *, *, #48310, .F. ) ;
#47698 = LINE ( 'NONE', #32163, #19997 ) ;
#47699 = EDGE_LOOP ( 'NONE', ( #11940, #18395, #27282, #46327 ) ) ;
#47700 = CARTESIAN_POINT ( 'NONE',  ( -339.1964088526558498, -130.1153096980153236, -58.63009191191284941 ) ) ;
#47701 = AXIS2_PLACEMENT_3D ( 'NONE', #42236, #10188, #14399 ) ;
#47702 = CIRCLE ( 'NONE', #31859, 125.0000000000000000 ) ;
#47703 = DIRECTION ( 'NONE',  ( -0.000000000000000000, 1.000000000000000000, -0.000000000000000000 ) ) ;
#47704 = ADVANCED_FACE ( 'NONE', ( #32546 ), #48851, .F. ) ;
#47705 = VERTEX_POINT ( 'NONE', #21499 ) ;
#47706 = AXIS2_PLACEMENT_3D ( 'NONE', #16843, #36802, #28637 ) ;
#47707 = LINE ( 'NONE', #7745, #36595 ) ;
#47708 = PLANE ( 'NONE',  #51565 ) ;
#47709 = FACE_OUTER_BOUND ( 'NONE', #17146, .T. ) ;
#47710 = CARTESIAN_POINT ( 'NONE',  ( -79.88691714431334390, -177.1207230881787780, 119.9572859573367367 ) ) ;
#47711 = EDGE_CURVE ( 'NONE', #40896, #6302, #470, .T. ) ;
#47712 = EDGE_LOOP ( 'NONE', ( #25314, #20068, #11684, #7826 ) ) ;
#47713 = CARTESIAN_POINT ( 'NONE',  ( 43.33156026654913262, 30.00000000000000355, -51.04247435516399634 ) ) ;
#47714 = ORIENTED_EDGE ( 'NONE', *, *, #40547, .T. ) ;
#47715 = ORIENTED_EDGE ( 'NONE', *, *, #51384, .T. ) ;
#47716 = CIRCLE ( 'NONE', #40115, 125.0000000000000000 ) ;
#47717 = DIRECTION ( 'NONE',  ( -0.000000000000000000, 1.000000000000000000, -0.000000000000000000 ) ) ;
#47719 = ORIENTED_EDGE ( 'NONE', *, *, #33060, .F. ) ;
#47718 = DIRECTION ( 'NONE',  ( 0.000000000000000000, -0.000000000000000000, 1.000000000000000000 ) ) ;
#47720 = ORIENTED_EDGE ( 'NONE', *, *, #24744, .T. ) ;
#47721 = DIRECTION ( 'NONE',  ( -1.000000000000000000, 0.000000000000000000, -1.043714542225393381E-14 ) ) ;
#47722 = CIRCLE ( 'NONE', #20022, 125.0000000000000000 ) ;
#47723 = DIRECTION ( 'NONE',  ( 0.000000000000000000, 1.000000000000000000, 0.000000000000000000 ) ) ;
#47724 = ORIENTED_EDGE ( 'NONE', *, *, #42332, .F. ) ;
#47725 = FACE_OUTER_BOUND ( 'NONE', #35345, .T. ) ;
#47726 = CARTESIAN_POINT ( 'NONE',  ( -330.4913330509368166, -95.63860483659122735, -52.00954392751761191 ) ) ;
#47727 = VERTEX_POINT ( 'NONE', #28846 ) ;
#47728 = DIRECTION ( 'NONE',  ( 0.1768902751225666370, 0.000000000000000000, 0.9842305779475979399 ) ) ;
#47729 = PLANE ( 'NONE',  #8192 ) ;
#47730 = ADVANCED_FACE ( 'NONE', ( #24927 ), #17573, .F. ) ;
#47731 = EDGE_CURVE ( 'NONE', #13383, #40543, #33056, .T. ) ;
#47732 = CARTESIAN_POINT ( 'NONE',  ( 41.00573479224733120, -193.5000000000000000, -87.27805883780175122 ) ) ;
#47733 = CARTESIAN_POINT ( 'NONE',  ( 59.29945538372744096, -183.6283474603465606, 63.31490529818492519 ) ) ;
#47734 = ORIENTED_EDGE ( 'NONE', *, *, #14484, .T. ) ;
#47735 = ORIENTED_EDGE ( 'NONE', *, *, #36557, .T. ) ;
#47736 = VERTEX_POINT ( 'NONE', #4432 ) ;
#47737 = CARTESIAN_POINT ( 'NONE',  ( 37.99238433767461487, -189.7472609257535510, -90.26448786734027863 ) ) ;
#47738 = CARTESIAN_POINT ( 'NONE',  ( -47.63353074800702558, -193.5000000000000000, -0.5338233779647817423 ) ) ;
#47739 = AXIS2_PLACEMENT_3D ( 'NONE', #46930, #31131, #35079 ) ;
#47740 = CARTESIAN_POINT ( 'NONE',  ( -339.1964088526558498, -123.5000000000000284, 0.000000000000000000 ) ) ;
#47741 = DIRECTION ( 'NONE',  ( 0.000000000000000000, 0.6631226582408039638, 0.7485107481710934207 ) ) ;
#47742 = CARTESIAN_POINT ( 'NONE',  ( -173.0003472773501585, -175.3837268820161057, 10.93003379476953363 ) ) ;
#47743 = VERTEX_POINT ( 'NONE', #13091 ) ;
#47744 = AXIS2_PLACEMENT_3D ( 'NONE', #19403, #24143, #27794 ) ;
#47745 = ADVANCED_FACE ( 'NONE', ( #20450 ), #36470, .F. ) ;
#47746 = EDGE_CURVE ( 'NONE', #48787, #4433, #28091, .T. ) ;
#47747 = DIRECTION ( 'NONE',  ( -0.000000000000000000, 1.000000000000000000, -0.000000000000000000 ) ) ;
#47748 = ORIENTED_EDGE ( 'NONE', *, *, #14943, .F. ) ;
#47750 = VERTEX_POINT ( 'NONE', #3005 ) ;
#47749 = DIRECTION ( 'NONE',  ( 0.5085311186492154079, 0.000000000000000000, 0.8610436117673585521 ) ) ;
#47751 = VECTOR ( 'NONE', #31754, 1000.000000000000000 ) ;
#47752 = ORIENTED_EDGE ( 'NONE', *, *, #36497, .F. ) ;
#47753 = ADVANCED_FACE ( 'NONE', ( #29894 ), #15118, .F. ) ;
#47754 = DIRECTION ( 'NONE',  ( -0.000000000000000000, -1.000000000000000000, -0.000000000000000000 ) ) ;
#47755 = PLANE ( 'NONE',  #10719 ) ;
#47756 = ADVANCED_FACE ( 'NONE', ( #22729 ), #19049, .T. ) ;
#47757 = DIRECTION ( 'NONE',  ( -0.000000000000000000, 1.000000000000000000, -0.000000000000000000 ) ) ;
#47758 = PLANE ( 'NONE',  #37660 ) ;
#47759 = VERTEX_POINT ( 'NONE', #25955 ) ;
#47760 = LINE ( 'NONE', #3862, #21668 ) ;
#47761 = VERTEX_POINT ( 'NONE', #19553 ) ;
#47762 = VECTOR ( 'NONE', #33587, 1000.000000000000000 ) ;
#47763 = ORIENTED_EDGE ( 'NONE', *, *, #49747, .T. ) ;
#47764 = LINE ( 'NONE', #27761, #48944 ) ;
#47765 = FACE_OUTER_BOUND ( 'NONE', #2291, .T. ) ;
#47766 = PLANE ( 'NONE',  #16372 ) ;
#47767 = DIRECTION ( 'NONE',  ( -0.000000000000000000, 1.000000000000000000, -0.000000000000000000 ) ) ;
#47768 = DIRECTION ( 'NONE',  ( 0.8124868780056783146, 0.000000000000000000, 0.5829794791144762289 ) ) ;
#47769 = ORIENTED_EDGE ( 'NONE', *, *, #35151, .T. ) ;
#47770 = DIRECTION ( 'NONE',  ( 0.000000000000000000, 0.000000000000000000, -1.000000000000000000 ) ) ;
#47771 = CARTESIAN_POINT ( 'NONE',  ( -4.794493649713349015, -193.5000000000000000, -117.1181148702518726 ) ) ;
#47772 = FACE_BOUND ( 'NONE', #50439, .T. ) ;
#47773 = EDGE_LOOP ( 'NONE', ( #32181, #9423, #34067, #14506 ) ) ;
#47774 = AXIS2_PLACEMENT_3D ( 'NONE', #38332, #10987, #26497 ) ;
#47775 = CARTESIAN_POINT ( 'NONE',  ( 67.04262753014327814, -189.7472609257535510, -47.74645837849745078 ) ) ;
#47776 = CIRCLE ( 'NONE', #4069, 125.0000000000000000 ) ;
#47777 = DIRECTION ( 'NONE',  ( 0.000000000000000000, 0.000000000000000000, 1.000000000000000000 ) ) ;
#47778 = VERTEX_POINT ( 'NONE', #47170 ) ;
#47779 = LINE ( 'NONE', #24127, #18733 ) ;
#47780 = ORIENTED_EDGE ( 'NONE', *, *, #36067, .F. ) ;
#47781 = CIRCLE ( 'NONE', #28436, 125.0000000000000000 ) ;
#47782 = CARTESIAN_POINT ( 'NONE',  ( -339.1964088526558498, -68.15673923803930734, -20.45418021416698551 ) ) ;
#47783 = FACE_BOUND ( 'NONE', #23746, .T. ) ;
#47785 = VERTEX_POINT ( 'NONE', #6956 ) ;
#47784 = DIRECTION ( 'NONE',  ( 0.5586467658036594619, 0.000000000000000000, -0.8294056854501971054 ) ) ;
#47786 = EDGE_CURVE ( 'NONE', #31544, #47106, #11144, .T. ) ;
#47787 = EDGE_CURVE ( 'NONE', #9277, #25409, #27169, .T. ) ;
#47788 = EDGE_CURVE ( 'NONE', #4302, #48486, #13875, .T. ) ;
#47789 = PLANE ( 'NONE',  #16830 ) ;
#47790 = ORIENTED_EDGE ( 'NONE', *, *, #6, .T. ) ;
#47791 = EDGE_CURVE ( 'NONE', #37366, #37251, #15366, .T. ) ;
#47792 = AXIS2_PLACEMENT_3D ( 'NONE', #25263, #11922, #20078 ) ;
#47793 = ORIENTED_EDGE ( 'NONE', *, *, #51826, .F. ) ;
#47794 = CARTESIAN_POINT ( 'NONE',  ( -48.47912675150885065, -177.1207230881787780, 6.938893903907228378E-15 ) ) ;
#47795 = ORIENTED_EDGE ( 'NONE', *, *, #21076, .F. ) ;
#47796 = EDGE_CURVE ( 'NONE', #35424, #34486, #47691, .T. ) ;
#47797 = FACE_OUTER_BOUND ( 'NONE', #40647, .T. ) ;
#47798 = ADVANCED_FACE ( 'NONE', ( #23254 ), #19310, .T. ) ;
#47799 = LINE ( 'NONE', #4169, #41437 ) ;
#47800 = EDGE_CURVE ( 'NONE', #716, #25977, #9936, .T. ) ;
#47801 = EDGE_CURVE ( 'NONE', #7649, #26442, #31375, .T. ) ;
#47802 = DIRECTION ( 'NONE',  ( -0.4677363560876381388, 0.000000000000000000, -0.8838680338115288970 ) ) ;
#47803 = DIRECTION ( 'NONE',  ( -0.1476465640024918202, 0.000000000000000000, 0.9890401873221624784 ) ) ;
#47804 = ORIENTED_EDGE ( 'NONE', *, *, #33949, .T. ) ;
#47806 = ORIENTED_EDGE ( 'NONE', *, *, #41047, .F. ) ;
#47805 = CARTESIAN_POINT ( 'NONE',  ( 46.00000000000000711, 0.000000000000000000, 51.00000000000000000 ) ) ;
#47807 = ORIENTED_EDGE ( 'NONE', *, *, #9274, .F. ) ;
#47808 = EDGE_CURVE ( 'NONE', #19701, #30167, #42949, .T. ) ;
#47809 = VECTOR ( 'NONE', #18315, 1000.000000000000000 ) ;
#47810 = CARTESIAN_POINT ( 'NONE',  ( -336.3521761649654422, -65.12692710742291524, -8.732051761643681687 ) ) ;
#47811 = ORIENTED_EDGE ( 'NONE', *, *, #29945, .F. ) ;
#47812 = PLANE ( 'NONE',  #4625 ) ;
#47813 = ORIENTED_EDGE ( 'NONE', *, *, #11696, .T. ) ;
#47814 = EDGE_CURVE ( 'NONE', #35764, #12660, #15545, .T. ) ;
#47815 = CARTESIAN_POINT ( 'NONE',  ( -48.88225018079683082, -193.5000000000000000, 0.9151456172430223468 ) ) ;
#47816 = ORIENTED_EDGE ( 'NONE', *, *, #10541, .T. ) ;
#47818 = DIRECTION ( 'NONE',  ( -0.05924062789372142729, 0.000000000000000000, 0.9982437317643209074 ) ) ;
#47817 = DIRECTION ( 'NONE',  ( 0.5085311186492216251, 0.000000000000000000, -0.8610436117673548884 ) ) ;
#47819 = ORIENTED_EDGE ( 'NONE', *, *, #15703, .F. ) ;
#47820 = EDGE_CURVE ( 'NONE', #16360, #46692, #35573, .T. ) ;
#47821 = FACE_OUTER_BOUND ( 'NONE', #46102, .T. ) ;
#47822 = VERTEX_POINT ( 'NONE', #33837 ) ;
#47823 = LINE ( 'NONE', #32281, #42170 ) ;
#47824 = CARTESIAN_POINT ( 'NONE',  ( 71.73509643893275722, -183.6283474603465606, -30.40954281680804172 ) ) ;
#47825 = LINE ( 'NONE', #32028, #46504 ) ;
#47826 = FACE_OUTER_BOUND ( 'NONE', #36248, .T. ) ;
#47827 = PLANE ( 'NONE',  #50121 ) ;
#47828 = CARTESIAN_POINT ( 'NONE',  ( 2.449293598294706119E-15, 20.00000000000000355, -20.00000000000000000 ) ) ;
#47829 = ORIENTED_EDGE ( 'NONE', *, *, #26595, .F. ) ;
#47830 = DIRECTION ( 'NONE',  ( 1.000000000000000000, 0.000000000000000000, 0.000000000000000000 ) ) ;
#47831 = CARTESIAN_POINT ( 'NONE',  ( -124.1938582159088327, -189.7472609257535510, -99.45993886622791536 ) ) ;
#47832 = EDGE_CURVE ( 'NONE', #1331, #47304, #20561, .T. ) ;
#47833 = DIRECTION ( 'NONE',  ( -0.1768902751225592818, 0.000000000000000000, -0.9842305779475992722 ) ) ;
#47834 = VECTOR ( 'NONE', #37764, 1000.000000000000000 ) ;
#47835 = DIRECTION ( 'NONE',  ( -0.2348860457809707758, 0.000000000000000000, -0.9720229140804138579 ) ) ;
#47836 = ORIENTED_EDGE ( 'NONE', *, *, #21832, .F. ) ;
#47837 = DIRECTION ( 'NONE',  ( 0.000000000000000000, 0.000000000000000000, 1.000000000000000000 ) ) ;
#47838 = CARTESIAN_POINT ( 'NONE',  ( -336.3521761649654422, -123.5000000000000284, 0.000000000000000000 ) ) ;
#47840 = VERTEX_POINT ( 'NONE', #34794 ) ;
#47839 = CARTESIAN_POINT ( 'NONE',  ( 7.403327498934737960, -189.7472609257535510, -110.6939782313521192 ) ) ;
#47841 = ORIENTED_EDGE ( 'NONE', *, *, #34001, .F. ) ;
#47842 = ORIENTED_EDGE ( 'NONE', *, *, #26832, .T. ) ;
#47843 = ORIENTED_EDGE ( 'NONE', *, *, #8050, .F. ) ;
#47844 = EDGE_CURVE ( 'NONE', #117, #44736, #6327, .T. ) ;
#47845 = CARTESIAN_POINT ( 'NONE',  ( -180.0000000000000568, -123.5000000000000284, 6.938893903907228378E-15 ) ) ;
#47846 = VECTOR ( 'NONE', #41239, 1000.000000000000000 ) ;
#47847 = CARTESIAN_POINT ( 'NONE',  ( -339.1964088526558498, -123.5000000000000284, 0.000000000000000000 ) ) ;
#47848 = CARTESIAN_POINT ( 'NONE',  ( -336.3521761649654422, -128.1121410293017391, 59.82247199109905011 ) ) ;
#47849 = DIRECTION ( 'NONE',  ( 1.000000000000000000, -0.000000000000000000, -0.000000000000000000 ) ) ;
#47850 = ORIENTED_EDGE ( 'NONE', *, *, #33572, .T. ) ;
#47851 = ADVANCED_FACE ( 'NONE', ( #8755 ), #36885, .F. ) ;
#47852 = EDGE_CURVE ( 'NONE', #26723, #16129, #24530, .T. ) ;
#47853 = EDGE_CURVE ( 'NONE', #16896, #2635, #28203, .T. ) ;
#47854 = CARTESIAN_POINT ( 'NONE',  ( 4.462259530680975139, 54.37685667866154660, -18.37340906701131615 ) ) ;
#47855 = ADVANCED_FACE ( 'NONE', ( #51895 ), #20071, .T. ) ;
#47856 = VERTEX_POINT ( 'NONE', #32412 ) ;
#47857 = ORIENTED_EDGE ( 'NONE', *, *, #26288, .F. ) ;
#47858 = ORIENTED_EDGE ( 'NONE', *, *, #37819, .T. ) ;
#47859 = DIRECTION ( 'NONE',  ( -0.000000000000000000, -0.2393156642875482742, 0.9709418174260544543 ) ) ;
#47860 = ORIENTED_EDGE ( 'NONE', *, *, #29861, .F. ) ;
#47861 = VECTOR ( 'NONE', #43715, 999.9999999999998863 ) ;
#47862 = CIRCLE ( 'NONE', #31079, 125.0000000000000000 ) ;
#47863 = CARTESIAN_POINT ( 'NONE',  ( -140.5285791076019279, -175.3837268820161057, -83.08371579725672973 ) ) ;
#47864 = PLANE ( 'NONE',  #28560 ) ;
#47867 = EDGE_LOOP ( 'NONE', ( #12352, #27416, #16641, #504 ) ) ;
#47866 = DIRECTION ( 'NONE',  ( 0.000000000000000000, -0.6631226582407989678, -0.7485107481710977506 ) ) ;
#47865 = CARTESIAN_POINT ( 'NONE',  ( 40.29886924377099433, 30.00000000000000355, -46.21030057994576623 ) ) ;
#47868 = EDGE_CURVE ( 'NONE', #11130, #29227, #19804, .T. ) ;
#47869 = DIRECTION ( 'NONE',  ( -1.000000000000000000, -0.000000000000000000, 0.000000000000000000 ) ) ;
#47870 = VERTEX_POINT ( 'NONE', #44254 ) ;
#47871 = LINE ( 'NONE', #27870, #9621 ) ;
#47872 = ORIENTED_EDGE ( 'NONE', *, *, #46499, .T. ) ;
#47873 = EDGE_CURVE ( 'NONE', #28133, #19912, #19769, .T. ) ;
#47874 = DIRECTION ( 'NONE',  ( 0.000000000000000000, -0.9350162426854194964, -0.3546048870425235200 ) ) ;
#47875 = CARTESIAN_POINT ( 'NONE',  ( 73.79319191488886531, -177.1207230881787780, 20.63201007055493008 ) ) ;
#47877 = LINE ( 'NONE', #11849, #23176 ) ;
#47876 = LINE ( 'NONE', #48125, #26553 ) ;
#47878 = ORIENTED_EDGE ( 'NONE', *, *, #10403, .F. ) ;
#47879 = EDGE_CURVE ( 'NONE', #43316, #5824, #12690, .T. ) ;
#47880 = CARTESIAN_POINT ( 'NONE',  ( -339.1964088526558498, -90.39567187580880159, -48.84008046109142498 ) ) ;
#47881 = CARTESIAN_POINT ( 'NONE',  ( -131.9398708394020332, -177.1207230881787780, 91.70840728318374602 ) ) ;
#47882 = VECTOR ( 'NONE', #23088, 1000.000000000000000 ) ;
#47883 = ORIENTED_EDGE ( 'NONE', *, *, #8354, .F. ) ;
#47884 = CARTESIAN_POINT ( 'NONE',  ( 76.51419089073347379, -177.1207230881787780, -1.292495564988661139 ) ) ;
#47885 = CARTESIAN_POINT ( 'NONE',  ( -172.2289551866394106, -189.7472609257535510, -17.63462396184707970 ) ) ;
#47886 = CARTESIAN_POINT ( 'NONE',  ( 68.24201764719070695, -177.1207230881787780, -44.73448837594910543 ) ) ;
#47887 = ORIENTED_EDGE ( 'NONE', *, *, #13552, .T. ) ;
#47888 = FACE_OUTER_BOUND ( 'NONE', #35344, .T. ) ;
#47889 = CARTESIAN_POINT ( 'NONE',  ( -339.1964088526558498, -64.86990808808704401, 6.615309698014191220 ) ) ;
#47890 = ORIENTED_EDGE ( 'NONE', *, *, #27888, .F. ) ;
#47891 = CARTESIAN_POINT ( 'NONE',  ( 60.00000000000001421, -63.50000000000000000, 60.00000000000000711 ) ) ;
#47892 = ORIENTED_EDGE ( 'NONE', *, *, #12717, .F. ) ;
#47893 = CARTESIAN_POINT ( 'NONE',  ( -48.47912675150885065, -175.3837268820161057, 6.938893903907228378E-15 ) ) ;
#47894 = PLANE ( 'NONE',  #27016 ) ;
#47895 = LINE ( 'NONE', #11100, #48727 ) ;
#47896 = LINE ( 'NONE', #39473, #36506 ) ;
#47897 = LINE ( 'NONE', #16351, #39976 ) ;
#47898 = VECTOR ( 'NONE', #38143, 1000.000000000000000 ) ;
#47899 = VECTOR ( 'NONE', #8142, 1000.000000000000000 ) ;
#47900 = PLANE ( 'NONE',  #42227 ) ;
#47901 = CARTESIAN_POINT ( 'NONE',  ( -330.4913330509368166, -123.5000000000000284, 0.000000000000000000 ) ) ;
#47902 = DIRECTION ( 'NONE',  ( 0.1182731709213660498, 0.000000000000000000, -0.9929810960135169173 ) ) ;
#47904 = ORIENTED_EDGE ( 'NONE', *, *, #52009, .F. ) ;
#47903 = CARTESIAN_POINT ( 'NONE',  ( -173.4787860028527007, -183.6283474603465606, 0.2918682030023308505 ) ) ;
#47905 = ORIENTED_EDGE ( 'NONE', *, *, #2595, .F. ) ;
#47906 = ADVANCED_FACE ( 'NONE', ( #873 ), #12441, .F. ) ;
#47907 = EDGE_CURVE ( 'NONE', #28151, #11654, #8858, .T. ) ;
#47908 = CARTESIAN_POINT ( 'NONE',  ( -48.98765787015805984, -193.5000000000000000, -0.8610436117673551104 ) ) ;
#47909 = DIRECTION ( 'NONE',  ( 0.000000000000000000, 0.000000000000000000, 1.000000000000000000 ) ) ;
#47910 = VERTEX_POINT ( 'NONE', #35840 ) ;
#47911 = EDGE_LOOP ( 'NONE', ( #8736, #35384, #11761, #19938 ) ) ;
#47912 = AXIS2_PLACEMENT_3D ( 'NONE', #38780, #35108, #2786 ) ;
#47913 = ORIENTED_EDGE ( 'NONE', *, *, #47015, .T. ) ;
#47914 = DIRECTION ( 'NONE',  ( 0.000000000000000000, 0.000000000000000000, 1.000000000000000000 ) ) ;
#47915 = DIRECTION ( 'NONE',  ( -1.000000000000000000, 0.000000000000000000, 0.000000000000000000 ) ) ;
#47916 = LINE ( 'NONE', #7954, #39528 ) ;
#47917 = LINE ( 'NONE', #7196, #47575 ) ;
#47918 = VERTEX_POINT ( 'NONE', #93 ) ;
#47919 = EDGE_LOOP ( 'NONE', ( #32522, #49828, #21772, #23902 ) ) ;
#47920 = ORIENTED_EDGE ( 'NONE', *, *, #41098, .F. ) ;
#47921 = CARTESIAN_POINT ( 'NONE',  ( -48.47912675150885065, -183.6283474603465606, 6.938893903907228378E-15 ) ) ;
#47922 = PLANE ( 'NONE',  #28519 ) ;
#47923 = LINE ( 'NONE', #23494, #45921 ) ;
#47924 = ADVANCED_FACE ( 'NONE', ( #48718 ), #16399, .T. ) ;
#47925 = CARTESIAN_POINT ( 'NONE',  ( -260.0000000000000000, -113.5000000000000000, 39.99999999999998579 ) ) ;
#47926 = DIRECTION ( 'NONE',  ( 0.000000000000000000, -0.000000000000000000, 1.000000000000000000 ) ) ;
#47927 = EDGE_LOOP ( 'NONE', ( #31815, #26828, #22439, #3280 ) ) ;
#47928 = FACE_OUTER_BOUND ( 'NONE', #38444, .T. ) ;
#47929 = VECTOR ( 'NONE', #31268, 1000.000000000000000 ) ;
#47930 = CARTESIAN_POINT ( 'NONE',  ( 23.33927677392130917, -183.6283474603465606, -102.3089288139528747 ) ) ;
#47931 = CARTESIAN_POINT ( 'NONE',  ( 0.000000000000000000, -63.50000000000000000, -60.00000000000000711 ) ) ;
#47932 = LINE ( 'NONE', #20857, #18165 ) ;
#47933 = EDGE_CURVE ( 'NONE', #47705, #7370, #28993, .T. ) ;
#47934 = AXIS2_PLACEMENT_3D ( 'NONE', #48287, #28303, #31982 ) ;
#47935 = ORIENTED_EDGE ( 'NONE', *, *, #49755, .T. ) ;
#47936 = EDGE_LOOP ( 'NONE', ( #23960, #20086, #50181, #25673 ) ) ;
#47937 = ORIENTED_EDGE ( 'NONE', *, *, #5735, .T. ) ;
#47938 = CARTESIAN_POINT ( 'NONE',  ( -49.44376233341720450, -175.3837268820161057, -0.2635871660690713436 ) ) ;
#47939 = FACE_OUTER_BOUND ( 'NONE', #8313, .T. ) ;
#47940 = ORIENTED_EDGE ( 'NONE', *, *, #14835, .T. ) ;
#47941 = FACE_OUTER_BOUND ( 'NONE', #893, .T. ) ;
#47942 = CARTESIAN_POINT ( 'NONE',  ( -339.1964088526558498, -167.3305728129742249, 39.49849221029288060 ) ) ;
#47943 = CARTESIAN_POINT ( 'NONE',  ( -336.3521761649654422, -94.63601285149479736, 51.48334306143172512 ) ) ;
#47944 = VERTEX_POINT ( 'NONE', #24278 ) ;
#47945 = DIRECTION ( 'NONE',  ( 0.000000000000000000, 0.000000000000000000, -1.000000000000000000 ) ) ;
#47946 = ORIENTED_EDGE ( 'NONE', *, *, #5318, .T. ) ;
#47947 = CARTESIAN_POINT ( 'NONE',  ( -142.9772358822569629, -183.6283474603465606, 81.82363577055970438 ) ) ;
#47948 = PLANE ( 'NONE',  #7813 ) ;
#47949 = CIRCLE ( 'NONE', #48782, 125.0000000000000000 ) ;
#47950 = CARTESIAN_POINT ( 'NONE',  ( -27.18512803868276251, -189.7472609257535510, -123.1729094355498404 ) ) ;
#47951 = ORIENTED_EDGE ( 'NONE', *, *, #10937, .T. ) ;
#47952 = DIRECTION ( 'NONE',  ( -1.000000000000000000, -0.000000000000000000, 0.000000000000000000 ) ) ;
#47953 = DIRECTION ( 'NONE',  ( 0.000000000000000000, 0.000000000000000000, 1.000000000000000000 ) ) ;
#47954 = DIRECTION ( 'NONE',  ( 0.000000000000000000, 0.000000000000000000, -1.000000000000000000 ) ) ;
#47955 = PLANE ( 'NONE',  #19888 ) ;
#47956 = ADVANCED_FACE ( 'NONE', ( #8494 ), #32924, .T. ) ;
#47957 = ORIENTED_EDGE ( 'NONE', *, *, #13820, .F. ) ;
#47958 = CARTESIAN_POINT ( 'NONE',  ( -27.18512803868275540, -175.3837268820161057, -123.1729094355498262 ) ) ;
#47959 = ORIENTED_EDGE ( 'NONE', *, *, #10270, .T. ) ;
#47960 = ORIENTED_EDGE ( 'NONE', *, *, #11988, .F. ) ;
#47961 = DIRECTION ( 'NONE',  ( -0.6528221181905280446, 0.000000000000000000, 0.7575112421616145841 ) ) ;
#47963 = VERTEX_POINT ( 'NONE', #4303 ) ;
#47962 = DIRECTION ( 'NONE',  ( 0.000000000000000000, 1.000000000000000000, -0.000000000000000000 ) ) ;
#47964 = AXIS2_PLACEMENT_3D ( 'NONE', #49060, #13317, #16759 ) ;
#47965 = ORIENTED_EDGE ( 'NONE', *, *, #43123, .T. ) ;
#47966 = DIRECTION ( 'NONE',  ( -0.000000000000000000, 1.000000000000000000, -0.000000000000000000 ) ) ;
#47967 = EDGE_CURVE ( 'NONE', #4130, #14785, #36534, .T. ) ;
#47968 = AXIS2_PLACEMENT_3D ( 'NONE', #35654, #7551, #8327 ) ;
#47969 = AXIS2_PLACEMENT_3D ( 'NONE', #18497, #19009, #51095 ) ;
#47970 = PLANE ( 'NONE',  #26819 ) ;
#47971 = EDGE_CURVE ( 'NONE', #41557, #50211, #44084, .T. ) ;
#47972 = ORIENTED_EDGE ( 'NONE', *, *, #15202, .T. ) ;
#47973 = PLANE ( 'NONE',  #13034 ) ;
#47974 = PLANE ( 'NONE',  #178 ) ;
#47975 = ORIENTED_EDGE ( 'NONE', *, *, #12422, .F. ) ;
#47976 = CARTESIAN_POINT ( 'NONE',  ( -340.0000000000000568, -78.50000000000002842, 0.000000000000000000 ) ) ;
#47977 = FACE_OUTER_BOUND ( 'NONE', #16685, .T. ) ;
#47978 = CARTESIAN_POINT ( 'NONE',  ( 5.015379008610445943, -183.6283474603465606, -112.9749434763326690 ) ) ;
#47979 = CARTESIAN_POINT ( 'NONE',  ( -137.2261550162227479, -183.6283474603465606, 86.60307583628416239 ) ) ;
#47980 = VERTEX_POINT ( 'NONE', #36619 ) ;
#47981 = VECTOR ( 'NONE', #18802, 1000.000000000000000 ) ;
#47982 = EDGE_LOOP ( 'NONE', ( #45300, #37769, #19138, #7401 ) ) ;
#47983 = ORIENTED_EDGE ( 'NONE', *, *, #559, .F. ) ;
#47984 = DIRECTION ( 'NONE',  ( -0.000000000000000000, 0.2393156642875547968, -0.9709418174260527890 ) ) ;
#47985 = DIRECTION ( 'NONE',  ( 0.000000000000000000, -0.4647231720437725033, -0.8854560256532079121 ) ) ;
#47986 = CIRCLE ( 'NONE', #27820, 5.000000000000001776 ) ;
#47987 = EDGE_CURVE ( 'NONE', #4203, #38934, #49166, .T. ) ;
#47988 = DIRECTION ( 'NONE',  ( 0.5315839928299667116, 0.000000000000000000, -0.8470055835512242393 ) ) ;
#47989 = CARTESIAN_POINT ( 'NONE',  ( -160.0000000000000284, -123.5000000000000284, -37.63467731922663972 ) ) ;
#47990 = LINE ( 'NONE', #44317, #356 ) ;
#47991 = EDGE_LOOP ( 'NONE', ( #41621, #49164, #37890, #18288 ) ) ;
#47992 = CARTESIAN_POINT ( 'NONE',  ( -146.8460685364478877, -183.6283474603465606, 75.49882471933933914 ) ) ;
#47993 = EDGE_LOOP ( 'NONE', ( #33713, #26138 ) ) ;
#47995 = VERTEX_POINT ( 'NONE', #23758 ) ;
#47994 = DIRECTION ( 'NONE',  ( 0.000000000000000000, -0.7485107481710934207, 0.6631226582408039638 ) ) ;
#47996 = VERTEX_POINT ( 'NONE', #39763 ) ;
#47997 = CARTESIAN_POINT ( 'NONE',  ( -48.36085358058748085, -183.6283474603465606, -0.9929810960135100339 ) ) ;
#47998 = DIRECTION ( 'NONE',  ( 0.000000000000000000, -0.3546048870425396182, -0.9350162426854132791 ) ) ;
#47999 = VECTOR ( 'NONE', #37070, 1000.000000000000000 ) ;
#48000 = CARTESIAN_POINT ( 'NONE',  ( -165.1736796818183564, -177.1207230881787780, -41.93543928473609839 ) ) ;
#48001 = FACE_OUTER_BOUND ( 'NONE', #43826, .T. ) ;
#48002 = ORIENTED_EDGE ( 'NONE', *, *, #51229, .T. ) ;
#48003 = CARTESIAN_POINT ( 'NONE',  ( -48.47912675150885065, -183.6283474603465606, 6.938893903907228378E-15 ) ) ;
#48004 = VECTOR ( 'NONE', #27707, 1000.000000000000114 ) ;
#48005 = ORIENTED_EDGE ( 'NONE', *, *, #44570, .T. ) ;
#48006 = VECTOR ( 'NONE', #23715, 1000.000000000000000 ) ;
#48007 = ORIENTED_EDGE ( 'NONE', *, *, #11964, .T. ) ;
#48008 = DIRECTION ( 'NONE',  ( 0.5586467658036535777, 0.000000000000000000, -0.8294056854502011022 ) ) ;
#48009 = CARTESIAN_POINT ( 'NONE',  ( 4.109287492203100634, -193.5000000000000000, -113.3995532942336979 ) ) ;
#48010 = CARTESIAN_POINT ( 'NONE',  ( 60.00000000000001421, -113.5000000000000142, 39.99999999999998579 ) ) ;
#48011 = ADVANCED_FACE ( 'NONE', ( #22150 ), #33714, .T. ) ;
#48012 = DIRECTION ( 'NONE',  ( 0.000000000000000000, 1.000000000000000000, 0.000000000000000000 ) ) ;
#48013 = DIRECTION ( 'NONE',  ( -0.9027978299657387629, 0.000000000000000000, -0.4300652022765304450 ) ) ;
#48014 = EDGE_LOOP ( 'NONE', ( #44151, #15803, #5189, #9337 ) ) ;
#48015 = DIRECTION ( 'NONE',  ( -0.000000000000000000, 1.000000000000000000, -0.000000000000000000 ) ) ;
#48016 = DIRECTION ( 'NONE',  ( -0.000000000000000000, 0.000000000000000000, -1.000000000000000000 ) ) ;
#48017 = VECTOR ( 'NONE', #25342, 1000.000000000000114 ) ;
#48018 = EDGE_CURVE ( 'NONE', #12556, #34369, #25067, .T. ) ;
#48019 = FACE_BOUND ( 'NONE', #26331, .T. ) ;
#48020 = VERTEX_POINT ( 'NONE', #49759 ) ;
#48021 = AXIS2_PLACEMENT_3D ( 'NONE', #6105, #10294, #6355 ) ;
#48022 = AXIS2_PLACEMENT_3D ( 'NONE', #18517, #2491, #11388 ) ;
#48023 = CARTESIAN_POINT ( 'NONE',  ( -137.2624501260119985, -183.6283474603465606, 87.99159897727967916 ) ) ;
#48024 = DIRECTION ( 'NONE',  ( 0.000000000000000000, 1.000000000000000000, 0.000000000000000000 ) ) ;
#48025 = ORIENTED_EDGE ( 'NONE', *, *, #47177, .T. ) ;
#48026 = DIRECTION ( 'NONE',  ( 1.000000000000000000, 4.051632851310703470E-17, 7.719741424018482920E-17 ) ) ;
#48027 = EDGE_CURVE ( 'NONE', #51992, #47640, #22295, .T. ) ;
#48028 = ORIENTED_EDGE ( 'NONE', *, *, #38464, .T. ) ;
#48029 = EDGE_CURVE ( 'NONE', #2635, #186, #13487, .T. ) ;
#48030 = EDGE_CURVE ( 'NONE', #27697, #13519, #33966, .T. ) ;
#48031 = DIRECTION ( 'NONE',  ( -0.000000000000000000, 1.000000000000000000, 0.000000000000000000 ) ) ;
#48032 = EDGE_CURVE ( 'NONE', #51044, #11395, #41077, .T. ) ;
#48033 = FACE_BOUND ( 'NONE', #28754, .T. ) ;
#48035 = ORIENTED_EDGE ( 'NONE', *, *, #37704, .T. ) ;
#48034 = PLANE ( 'NONE',  #40493 ) ;
#48036 = AXIS2_PLACEMENT_3D ( 'NONE', #19682, #23385, #12580 ) ;
#48037 = DIRECTION ( 'NONE',  ( -0.000000000000000000, 1.000000000000000000, 0.000000000000000000 ) ) ;
#48038 = ORIENTED_EDGE ( 'NONE', *, *, #10832, .F. ) ;
#48039 = AXIS2_PLACEMENT_3D ( 'NONE', #12920, #32890, #48941 ) ;
#48040 = ORIENTED_EDGE ( 'NONE', *, *, #45542, .T. ) ;
#48041 = CARTESIAN_POINT ( 'NONE',  ( -163.0741914257288272, -175.3837268820161057, 47.37063079638398477 ) ) ;
#48042 = ORIENTED_EDGE ( 'NONE', *, *, #38224, .T. ) ;
#48043 = DIRECTION ( 'NONE',  ( 0.000000000000000000, 0.000000000000000000, -1.000000000000000000 ) ) ;
#48044 = CARTESIAN_POINT ( 'NONE',  ( -336.3521761649654422, -69.26746417191145611, -23.38292116578723068 ) ) ;
#48045 = VECTOR ( 'NONE', #19981, 1000.000000000000000 ) ;
#48046 = AXIS2_PLACEMENT_3D ( 'NONE', #36102, #12445, #25071 ) ;
#48047 = SURFACE_STYLE_FILL_AREA ( #16000 ) ;
#48048 = LINE ( 'NONE', #4683, #45773 ) ;
#48049 = ORIENTED_EDGE ( 'NONE', *, *, #20803, .F. ) ;
#48052 = VERTEX_POINT ( 'NONE', #17452 ) ;
#48051 = DIRECTION ( 'NONE',  ( -0.000000000000000000, 1.000000000000000000, 0.000000000000000000 ) ) ;
#48050 = FACE_OUTER_BOUND ( 'NONE', #45152, .T. ) ;
#48053 = VECTOR ( 'NONE', #16480, 1000.000000000000000 ) ;
#48054 = AXIS2_PLACEMENT_3D ( 'NONE', #9308, #45572, #25574 ) ;
#48055 = ORIENTED_EDGE ( 'NONE', *, *, #33380, .F. ) ;
#48056 = DIRECTION ( 'NONE',  ( 0.000000000000000000, -1.000000000000000000, -0.000000000000000000 ) ) ;
#48057 = VERTEX_POINT ( 'NONE', #49238 ) ;
#48058 = DIRECTION ( 'NONE',  ( 1.000000000000000000, -0.000000000000000000, -0.000000000000000000 ) ) ;
#48059 = VERTEX_POINT ( 'NONE', #37132 ) ;
#48060 = VECTOR ( 'NONE', #13388, 1000.000000000000000 ) ;
#48061 = DIRECTION ( 'NONE',  ( 0.8455960035018272869, 0.000000000000000000, -0.5338233779647886257 ) ) ;
#48062 = EDGE_LOOP ( 'NONE', ( #26148, #39524, #20874, #48426 ) ) ;
#48064 = CARTESIAN_POINT ( 'NONE',  ( 11.52087324849114580, -173.5000000000000284, -186.7953921478704729 ) ) ;
#48063 = DIRECTION ( 'NONE',  ( 0.000000000000000000, -0.4647231720437789981, -0.8854560256532044704 ) ) ;
#48065 = VERTEX_POINT ( 'NONE', #33473 ) ;
#48066 = ORIENTED_EDGE ( 'NONE', *, *, #10840, .F. ) ;
#48067 = CARTESIAN_POINT ( 'NONE',  ( -2.700932609314990351, -177.1207230881787780, -116.3157639405751667 ) ) ;
#48068 = LINE ( 'NONE', #44120, #31549 ) ;
#48069 = DIRECTION ( 'NONE',  ( 0.000000000000000000, 1.000000000000000000, -0.000000000000000000 ) ) ;
#48070 = CARTESIAN_POINT ( 'NONE',  ( 38.46761263173350898, -189.7472609257535510, 89.80681772907070126 ) ) ;
#48071 = DIRECTION ( 'NONE',  ( 0.000000000000000000, -0.000000000000000000, 1.000000000000000000 ) ) ;
#48072 = VECTOR ( 'NONE', #37983, 1000.000000000000114 ) ;
#48073 = LINE ( 'NONE', #20466, #38975 ) ;
#48074 = EDGE_CURVE ( 'NONE', #45175, #27697, #17175, .T. ) ;
#48075 = ADVANCED_FACE ( 'NONE', ( #45559 ), #21897, .F. ) ;
#48076 = ORIENTED_EDGE ( 'NONE', *, *, #13638, .T. ) ;
#48077 = EDGE_CURVE ( 'NONE', #40019, #6739, #21431, .T. ) ;
#48078 =( NAMED_UNIT ( * ) PLANE_ANGLE_UNIT ( ) SI_UNIT ( $, .RADIAN. ) );
#48079 = CARTESIAN_POINT ( 'NONE',  ( -169.9883746053192795, -189.7472609257535510, -24.72869175143020826 ) ) ;
#48080 = DIRECTION ( 'NONE',  ( 0.000000000000000000, 0.000000000000000000, -1.000000000000000000 ) ) ;
#48081 = AXIS2_PLACEMENT_3D ( 'NONE', #43384, #7390, #44422 ) ;
#48082 = DIRECTION ( 'NONE',  ( 0.000000000000000000, 0.000000000000000000, 1.000000000000000000 ) ) ;
#48083 = ORIENTED_EDGE ( 'NONE', *, *, #27561, .T. ) ;
#48084 = CARTESIAN_POINT ( 'NONE',  ( -46.06708674231130374, -183.6283474603465606, -124.9767260852756863 ) ) ;
#48085 = ADVANCED_FACE ( 'NONE', ( #45306 ), #25316, .F. ) ;
#48086 = DIRECTION ( 'NONE',  ( 0.9646355819083594074, 0.000000000000000000, -0.2635871660690647933 ) ) ;
#48087 = LINE ( 'NONE', #8402, #48450 ) ;
#48088 = ORIENTED_EDGE ( 'NONE', *, *, #12668, .T. ) ;
#48089 = ORIENTED_EDGE ( 'NONE', *, *, #34978, .T. ) ;
#48090 = EDGE_CURVE ( 'NONE', #26719, #15605, #5618, .T. ) ;
#48091 = VECTOR ( 'NONE', #16031, 1000.000000000000227 ) ;
#48092 = EDGE_LOOP ( 'NONE', ( #41737, #46142, #41057, #11383 ) ) ;
#48093 = VECTOR ( 'NONE', #2848, 1000.000000000000000 ) ;
#48094 = EDGE_CURVE ( 'NONE', #15388, #33963, #35717, .T. ) ;
#48095 = PLANE ( 'NONE',  #30920 ) ;
#48096 = VECTOR ( 'NONE', #1356, 1000.000000000000000 ) ;
#48097 = EDGE_CURVE ( 'NONE', #41262, #11883, #44125, .T. ) ;
#48098 = CARTESIAN_POINT ( 'NONE',  ( -167.6453766917639427, -193.5000000000000000, 37.74128873232411507 ) ) ;
#48099 = CARTESIAN_POINT ( 'NONE',  ( 73.09196206113300320, -183.6283474603465606, 29.07697310430964421 ) ) ;
#48100 = PLANE ( 'NONE',  #49716 ) ;
#48101 = ADVANCED_FACE ( 'NONE', ( #30035 ), #46085, .T. ) ;
#48102 = EDGE_LOOP ( 'NONE', ( #24773, #9501, #28082, #47890 ) ) ;
#48103 = VECTOR ( 'NONE', #17018, 1000.000000000000000 ) ;
#48104 = DIRECTION ( 'NONE',  ( 0.000000000000000000, -1.000000000000000000, 0.000000000000000000 ) ) ;
#48105 = VERTEX_POINT ( 'NONE', #1398 ) ;
#48106 = VERTEX_POINT ( 'NONE', #1666 ) ;
#48107 = ORIENTED_EDGE ( 'NONE', *, *, #47177, .F. ) ;
#48108 = ORIENTED_EDGE ( 'NONE', *, *, #29462, .F. ) ;
#48109 = DIRECTION ( 'NONE',  ( -0.6528221181905174975, 0.000000000000000000, -0.7575112421616236880 ) ) ;
#48110 = VECTOR ( 'NONE', #23394, 1000.000000000000000 ) ;
#48111 = ORIENTED_EDGE ( 'NONE', *, *, #17958, .T. ) ;
#48112 = EDGE_CURVE ( 'NONE', #37279, #26450, #7179, .T. ) ;
#48113 = AXIS2_PLACEMENT_3D ( 'NONE', #7184, #14305, #43451 ) ;
#48114 = LINE ( 'NONE', #39681, #30062 ) ;
#48115 = CARTESIAN_POINT ( 'NONE',  ( -336.3521761649654422, -85.59754891220836726, -45.24454186338619621 ) ) ;
#48118 = ORIENTED_EDGE ( 'NONE', *, *, #10172, .T. ) ;
#48117 = PLANE ( 'NONE',  #17416 ) ;
#48116 = CARTESIAN_POINT ( 'NONE',  ( -100.6109117578263152, -183.6283474603465606, 112.5098962032393359 ) ) ;
#48119 = CARTESIAN_POINT ( 'NONE',  ( 35.67816836544800196, -177.1207230881787780, -92.42591454022745268 ) ) ;
#48120 = ORIENTED_EDGE ( 'NONE', *, *, #32392, .F. ) ;
#48121 = DIRECTION ( 'NONE',  ( 0.000000000000000000, 0.000000000000000000, -1.000000000000000000 ) ) ;
#48122 = ORIENTED_EDGE ( 'NONE', *, *, #5327, .T. ) ;
#48123 = DIRECTION ( 'NONE',  ( -0.9995608365087940150, 0.000000000000000000, -0.02963332782257007206 ) ) ;
#48124 = LINE ( 'NONE', #35767, #28821 ) ;
#48126 = CARTESIAN_POINT ( 'NONE',  ( 68.24201764719070695, -183.6283474603465606, -44.73448837594909833 ) ) ;
#48125 = CARTESIAN_POINT ( 'NONE',  ( -101.9736325116273576, -177.1207230881787780, 112.9749434763330811 ) ) ;
#48127 = VECTOR ( 'NONE', #18450, 1000.000000000000000 ) ;
#48128 = VERTEX_POINT ( 'NONE', #34238 ) ;
#48129 = EDGE_CURVE ( 'NONE', #21574, #30158, #12952, .T. ) ;
#48130 = LINE ( 'NONE', #3985, #9712 ) ;
#48131 = VECTOR ( 'NONE', #15697, 1000.000000000000000 ) ;
#48132 = DIRECTION ( 'NONE',  ( -0.7765238627180482966, 0.000000000000000000, 0.6300878435817038881 ) ) ;
#48133 = DIRECTION ( 'NONE',  ( 0.000000000000000000, 0.000000000000000000, -1.000000000000000000 ) ) ;
#48134 = ORIENTED_EDGE ( 'NONE', *, *, #47074, .T. ) ;
#48135 = CARTESIAN_POINT ( 'NONE',  ( 47.70255505652111339, -189.7472609257535510, 78.26291788638732783 ) ) ;
#48136 = LINE ( 'NONE', #47885, #31558 ) ;
#48137 = LINE ( 'NONE', #8193, #17331 ) ;
#48138 = EDGE_CURVE ( 'NONE', #40953, #978, #19249, .T. ) ;
#48139 = EDGE_CURVE ( 'NONE', #9556, #30483, #51681, .T. ) ;
#48140 = EDGE_CURVE ( 'NONE', #1324, #51755, #38435, .T. ) ;
#48141 = ORIENTED_EDGE ( 'NONE', *, *, #22345, .T. ) ;
#48142 = EDGE_CURVE ( 'NONE', #2545, #4861, #31316, .T. ) ;
#48143 = CARTESIAN_POINT ( 'NONE',  ( 23.33927677392130917, -193.5000000000000000, -102.3089288139528747 ) ) ;
#48144 = LINE ( 'NONE', #12115, #10504 ) ;
#48145 = EDGE_CURVE ( 'NONE', #8800, #42139, #26491, .T. ) ;
#48146 = ORIENTED_EDGE ( 'NONE', *, *, #32332, .T. ) ;
#48147 = CARTESIAN_POINT ( 'NONE',  ( 70.20858612167234014, -183.6283474603465606, 35.90758392117750475 ) ) ;
#48148 = EDGE_LOOP ( 'NONE', ( #23408, #19014, #35093, #12942 ) ) ;
#48149 = DIRECTION ( 'NONE',  ( 0.000000000000000000, 1.000000000000000000, -0.000000000000000000 ) ) ;
#48150 = ADVANCED_FACE ( 'NONE', ( #42886 ), #15300, .T. ) ;
#48151 = DIRECTION ( 'NONE',  ( 0.000000000000000000, -0.000000000000000000, 1.000000000000000000 ) ) ;
#48152 = VECTOR ( 'NONE', #19134, 1000.000000000000000 ) ;
#48153 = PLANE ( 'NONE',  #42000 ) ;
#48154 = CARTESIAN_POINT ( 'NONE',  ( -180.0000000000000568, -123.5000000000000284, -45.63467731922664683 ) ) ;
#48155 = CARTESIAN_POINT ( 'NONE',  ( -133.8011377042516301, -177.1207230881787780, -91.35181687837437892 ) ) ;
#48156 = EDGE_CURVE ( 'NONE', #20663, #48860, #30686, .T. ) ;
#48157 = CIRCLE ( 'NONE', #40554, 125.0000000000000000 ) ;
#48158 = EDGE_CURVE ( 'NONE', #20663, #39795, #14270, .T. ) ;
#48159 = DIRECTION ( 'NONE',  ( 1.000000000000000000, -0.000000000000000000, -0.000000000000000000 ) ) ;
#48160 = EDGE_CURVE ( 'NONE', #47261, #16316, #50789, .T. ) ;
#48161 = DIRECTION ( 'NONE',  ( 0.000000000000000000, -1.346129392433909288E-16, 1.000000000000000000 ) ) ;
#48162 = DIRECTION ( 'NONE',  ( -0.000000000000000000, 1.000000000000000000, -0.000000000000000000 ) ) ;
#48164 = VERTEX_POINT ( 'NONE', #18466 ) ;
#48163 = CARTESIAN_POINT ( 'NONE',  ( -95.37971604807238180, -183.6283474603465606, -114.7887733785764226 ) ) ;
#48165 = EDGE_CURVE ( 'NONE', #23027, #25456, #8040, .T. ) ;
#48166 = ORIENTED_EDGE ( 'NONE', *, *, #34639, .T. ) ;
#48167 = CARTESIAN_POINT ( 'NONE',  ( -78.64590280292341617, -189.7472609257535510, -121.3052580173827408 ) ) ;
#48168 = VECTOR ( 'NONE', #20439, 1000.000000000000000 ) ;
#48169 = EDGE_CURVE ( 'NONE', #34175, #10145, #35258, .T. ) ;
#48170 = PLANE ( 'NONE',  #23767 ) ;
#48171 = ORIENTED_EDGE ( 'NONE', *, *, #33962, .T. ) ;
#48172 = ORIENTED_EDGE ( 'NONE', *, *, #15400, .F. ) ;
#48173 = ORIENTED_EDGE ( 'NONE', *, *, #7183, .F. ) ;
#48174 = CARTESIAN_POINT ( 'NONE',  ( -49.03777351731250889, -193.5000000000000000, 0.8294056854502042109 ) ) ;
#48175 = CARTESIAN_POINT ( 'NONE',  ( -330.4913330509368166, -150.4759391377553186, 52.47426709956150859 ) ) ;
#48176 = FACE_OUTER_BOUND ( 'NONE', #27154, .T. ) ;
#48177 = CARTESIAN_POINT ( 'NONE',  ( -88.49718702276017268, -193.5000000000000000, -117.3655938605927389 ) ) ;
#48178 = EDGE_LOOP ( 'NONE', ( #36267, #7598, #11900, #41919 ) ) ;
#48179 = ORIENTED_EDGE ( 'NONE', *, *, #7513, .F. ) ;
#48180 = ADVANCED_FACE ( 'NONE', ( #34484 ), #50533, .T. ) ;
#48181 = VERTEX_POINT ( 'NONE', #42638 ) ;
#48182 = ADVANCED_FACE ( 'NONE', ( #14532 ), #22669, .T. ) ;
#48183 = CARTESIAN_POINT ( 'NONE',  ( -5.732832253866452454, -175.3837268820161057, -117.4638425504666799 ) ) ;
#48184 = PLANE ( 'NONE',  #32736 ) ;
#48185 = CARTESIAN_POINT ( 'NONE',  ( -330.4913330509368166, -182.0095552316575152, 7.608018572113473432 ) ) ;
#48186 = LINE ( 'NONE', #12156, #14497 ) ;
#48187 = CARTESIAN_POINT ( 'NONE',  ( -170.7514454179067513, -183.6283474603465606, -20.63201007055403480 ) ) ;
#48188 = VECTOR ( 'NONE', #4555, 1000.000000000000114 ) ;
#48189 = ORIENTED_EDGE ( 'NONE', *, *, #41657, .T. ) ;
#48190 = FACE_OUTER_BOUND ( 'NONE', #38933, .T. ) ;
#48191 = VECTOR ( 'NONE', #49635, 1000.000000000000000 ) ;
#48192 = CARTESIAN_POINT ( 'NONE',  ( 11.10560377650619301, -183.6283474603465606, -108.7464374498168951 ) ) ;
#48193 = CARTESIAN_POINT ( 'NONE',  ( 56.46549106873199264, -189.7472609257535510, -66.05018866041272929 ) ) ;
#48194 = CARTESIAN_POINT ( 'NONE',  ( -339.1964088526558498, -123.5000000000000284, 0.000000000000000000 ) ) ;
#48195 = AXIS2_PLACEMENT_3D ( 'NONE', #6973, #7233, #38246 ) ;
#48196 = EDGE_LOOP ( 'NONE', ( #20965, #13853, #50661, #15266 ) ) ;
#48197 = EDGE_LOOP ( 'NONE', ( #7994, #17459, #26888, #2966 ) ) ;
#48198 = VERTEX_POINT ( 'NONE', #6893 ) ;
#48199 = CARTESIAN_POINT ( 'NONE',  ( -133.8011377042516301, -183.6283474603465606, -91.35181687837437892 ) ) ;
#48200 = CARTESIAN_POINT ( 'NONE',  ( 58.48829670243886625, -183.6283474603465606, -64.67588669375805921 ) ) ;
#48201 = EDGE_LOOP ( 'NONE', ( #44563, #50376, #16254, #36007 ) ) ;
#48202 = CARTESIAN_POINT ( 'NONE',  ( -180.0000000000000568, -123.5000000000000284, -15.24495751795538290 ) ) ;
#48203 = PLANE ( 'NONE',  #23699 ) ;
#48204 = EDGE_CURVE ( 'NONE', #38453, #19435, #46589, .T. ) ;
#48206 = EDGE_CURVE ( 'NONE', #37592, #13526, #10573, .T. ) ;
#48205 = CARTESIAN_POINT ( 'NONE',  ( -49.42645310536303782, -183.6283474603465606, -0.3202698538628417357 ) ) ;
#48207 = EDGE_LOOP ( 'NONE', ( #39203, #42257, #31166, #22265 ) ) ;
#48208 = CARTESIAN_POINT ( 'NONE',  ( -339.1964088526558498, -182.0095552316575152, 7.608018572113563138 ) ) ;
#48209 = AXIS2_PLACEMENT_3D ( 'NONE', #2492, #22976, #38987 ) ;
#48210 = EDGE_CURVE ( 'NONE', #12390, #32491, #11336, .T. ) ;
#48211 = ORIENTED_EDGE ( 'NONE', *, *, #28833, .F. ) ;
#48212 = CARTESIAN_POINT ( 'NONE',  ( -123.8574911141017765, -193.5000000000000000, 98.45863302693528851 ) ) ;
#48213 = ORIENTED_EDGE ( 'NONE', *, *, #14626, .F. ) ;
#48214 = DIRECTION ( 'NONE',  ( -0.000000000000000000, 1.000000000000000000, -0.000000000000000000 ) ) ;
#48215 = CARTESIAN_POINT ( 'NONE',  ( 56.46549106873199975, -175.3837268820161057, -66.05018866041274350 ) ) ;
#48216 = ORIENTED_EDGE ( 'NONE', *, *, #34108, .F. ) ;
#48217 = DIRECTION ( 'NONE',  ( 0.000000000000000000, 0.000000000000000000, -1.000000000000000000 ) ) ;
#48218 = CARTESIAN_POINT ( 'NONE',  ( -332.3517673607765914, -120.8677111499054320, 59.00000000000000000 ) ) ;
#48219 = CARTESIAN_POINT ( 'NONE',  ( 74.61260187273138911, -177.1207230881787780, -14.98512977653175149 ) ) ;
#48220 = DIRECTION ( 'NONE',  ( -1.000000000000000000, 0.000000000000000000, -0.000000000000000000 ) ) ;
#48221 = ORIENTED_EDGE ( 'NONE', *, *, #35267, .T. ) ;
#48222 = DIRECTION ( 'NONE',  ( 0.000000000000000000, 0.000000000000000000, 1.000000000000000000 ) ) ;
#48223 = VERTEX_POINT ( 'NONE', #18985 ) ;
#48224 = EDGE_LOOP ( 'NONE', ( #43351, #478, #24553, #8399 ) ) ;
#48225 = EDGE_CURVE ( 'NONE', #42327, #32964, #43420, .T. ) ;
#48226 = CARTESIAN_POINT ( 'NONE',  ( 26.70958190211000982, -175.3837268820161057, -99.85818990449013199 ) ) ;
#48228 = ORIENTED_EDGE ( 'NONE', *, *, #15823, .T. ) ;
#48227 = DIRECTION ( 'NONE',  ( 0.000000000000000000, -1.000000000000000000, 0.000000000000000000 ) ) ;
#48229 = AXIS2_PLACEMENT_3D ( 'NONE', #47618, #15820, #28124 ) ;
#48230 = AXIS2_PLACEMENT_3D ( 'NONE', #40959, #12842, #24945 ) ;
#48231 = ORIENTED_EDGE ( 'NONE', *, *, #31518, .T. ) ;
#48232 = CARTESIAN_POINT ( 'NONE',  ( -330.4913330509368166, -172.3400804610915031, -33.10432812419114157 ) ) ;
#48233 = CIRCLE ( 'NONE', #25560, 125.0000000000000000 ) ;
#48234 = EDGE_CURVE ( 'NONE', #653, #672, #19486, .T. ) ;
#48235 = DIRECTION ( 'NONE',  ( -0.000000000000000000, 1.000000000000000000, -0.000000000000000000 ) ) ;
#48236 = ORIENTED_EDGE ( 'NONE', *, *, #29562, .T. ) ;
#48237 = LINE ( 'NONE', #28246, #50794 ) ;
#48238 = CARTESIAN_POINT ( 'NONE',  ( -47.78257572244585560, -177.1207230881787780, -0.7175072570443230546 ) ) ;
#48239 = ORIENTED_EDGE ( 'NONE', *, *, #22029, .T. ) ;
#48240 = PLANE ( 'NONE',  #23332 ) ;
#48241 = LINE ( 'NONE', #48511, #31672 ) ;
#48242 = PLANE ( 'NONE',  #7619 ) ;
#48243 = CARTESIAN_POINT ( 'NONE',  ( -1.230335819511603423, -193.5000000000000000, 115.7261930397108216 ) ) ;
#48244 = ORIENTED_EDGE ( 'NONE', *, *, #10082, .T. ) ;
#48245 = ORIENTED_EDGE ( 'NONE', *, *, #33844, .F. ) ;
#48246 = ORIENTED_EDGE ( 'NONE', *, *, #23642, .F. ) ;
#48247 = CARTESIAN_POINT ( 'NONE',  ( -135.4258661347518853, -175.3837268820161057, -89.80681772907007598 ) ) ;
#48248 = FACE_OUTER_BOUND ( 'NONE', #41284, .T. ) ;
#48249 = DIRECTION ( 'NONE',  ( 0.000000000000000000, 0.000000000000000000, -1.000000000000000000 ) ) ;
#48250 = FACE_BOUND ( 'NONE', #1930, .T. ) ;
#48251 = DIRECTION ( 'NONE',  ( 0.000000000000000000, -1.000000000000000000, -0.000000000000000000 ) ) ;
#48252 = VERTEX_POINT ( 'NONE', #8702 ) ;
#48253 = VERTEX_POINT ( 'NONE', #25510 ) ;
#48255 = ORIENTED_EDGE ( 'NONE', *, *, #50726, .F. ) ;
#48254 = CARTESIAN_POINT ( 'NONE',  ( -115.4536696835168641, -177.1207230881787780, -105.5434062319793185 ) ) ;
#48256 = ORIENTED_EDGE ( 'NONE', *, *, #24629, .F. ) ;
#48257 = VECTOR ( 'NONE', #43026, 1000.000000000000114 ) ;
#48258 = DIRECTION ( 'NONE',  ( 0.000000000000000000, 0.000000000000000000, 1.000000000000000000 ) ) ;
#48259 = LINE ( 'NONE', #49307, #27478 ) ;
#48260 = VECTOR ( 'NONE', #16010, 1000.000000000000000 ) ;
#48261 = VECTOR ( 'NONE', #15965, 1000.000000000000000 ) ;
#48262 = DIRECTION ( 'NONE',  ( 0.000000000000000000, 1.000000000000000000, 0.000000000000000000 ) ) ;
#48263 = EDGE_CURVE ( 'NONE', #26317, #51929, #33416, .T. ) ;
#48264 = CARTESIAN_POINT ( 'NONE',  ( -1.578537454945990293, -193.5000000000000000, 114.7887733785766926 ) ) ;
#48265 = ORIENTED_EDGE ( 'NONE', *, *, #34012, .T. ) ;
#48266 = DIRECTION ( 'NONE',  ( -0.000000000000000000, 1.000000000000000000, 0.000000000000000000 ) ) ;
#48267 = ORIENTED_EDGE ( 'NONE', *, *, #43952, .T. ) ;
#48268 = AXIS2_PLACEMENT_3D ( 'NONE', #11496, #22820, #2839 ) ;
#48269 = ORIENTED_EDGE ( 'NONE', *, *, #30406, .T. ) ;
#48270 = CARTESIAN_POINT ( 'NONE',  ( -128.2395503755045638, -183.6283474603465606, -96.24590808611419845 ) ) ;
#48271 = AXIS2_PLACEMENT_3D ( 'NONE', #20445, #48051, #16522 ) ;
#48272 = LINE ( 'NONE', #43288, #16087 ) ;
#48273 = FACE_OUTER_BOUND ( 'NONE', #18990, .T. ) ;
#48274 = AXIS2_PLACEMENT_3D ( 'NONE', #41897, #6432, #9846 ) ;
#48275 = DIRECTION ( 'NONE',  ( 4.884776371667510679E-16, 0.000000000000000000, -1.000000000000000000 ) ) ;
#48276 = DIRECTION ( 'NONE',  ( 0.9266896074318291543, 0.000000000000000000, 0.3758275821142488260 ) ) ;
#48277 = DIRECTION ( 'NONE',  ( -0.8896570909947530970, 0.000000000000000000, 0.4566292373937018700 ) ) ;
#48278 = ORIENTED_EDGE ( 'NONE', *, *, #2173, .T. ) ;
#48279 = VECTOR ( 'NONE', #4232, 1000.000000000000000 ) ;
#48280 = CARTESIAN_POINT ( 'NONE',  ( -330.4913330509368166, -123.5000000000000142, 60.00000000000000000 ) ) ;
#48281 = CARTESIAN_POINT ( 'NONE',  ( -168.8371699641976420, -189.7472609257535510, 33.74820638215509661 ) ) ;
#48282 = VECTOR ( 'NONE', #34412, 1000.000000000000000 ) ;
#48283 = FACE_BOUND ( 'NONE', #35868, .T. ) ;
#48284 = EDGE_LOOP ( 'NONE', ( #47714, #18099, #13950, #3319 ) ) ;
#48285 = EDGE_CURVE ( 'NONE', #28119, #27646, #44159, .T. ) ;
#48286 = DIRECTION ( 'NONE',  ( -0.1182731709213660498, 0.000000000000000000, 0.9929810960135169173 ) ) ;
#48287 = CARTESIAN_POINT ( 'NONE',  ( 0.000000000000000000, -89.98417994286192823, -48.55604808772582004 ) ) ;
#48288 = VERTEX_POINT ( 'NONE', #44711 ) ;
#48289 = DIRECTION ( 'NONE',  ( 0.7765238627180393038, 0.000000000000000000, 0.6300878435817147682 ) ) ;
#48290 = ORIENTED_EDGE ( 'NONE', *, *, #47683, .F. ) ;
#48291 = CARTESIAN_POINT ( 'NONE',  ( -164.6246685127424882, -189.7472609257535510, -46.20836643930983456 ) ) ;
#48292 = AXIS2_PLACEMENT_3D ( 'NONE', #32355, #23698, #39464 ) ;
#48293 = FACE_BOUND ( 'NONE', #3218, .T. ) ;
#48294 = CARTESIAN_POINT ( 'NONE',  ( -140.5933766095837427, -175.3837268820161057, -84.49831343337065448 ) ) ;
#48295 = VECTOR ( 'NONE', #42368, 1000.000000000000000 ) ;
#48296 = CIRCLE ( 'NONE', #11366, 124.9999999999999858 ) ;
#48297 = EDGE_CURVE ( 'NONE', #51884, #17654, #33246, .T. ) ;
#48298 = CARTESIAN_POINT ( 'NONE',  ( -332.3517673607765914, -159.1821513111375452, -47.06073758877369073 ) ) ;
#48299 = ORIENTED_EDGE ( 'NONE', *, *, #8348, .T. ) ;
#48300 = AXIS2_PLACEMENT_3D ( 'NONE', #24367, #24121, #36437 ) ;
#48301 = VERTEX_POINT ( 'NONE', #49178 ) ;
#48302 = CARTESIAN_POINT ( 'NONE',  ( 56.77503207194101265, -175.3837268820161057, -67.42819922234311036 ) ) ;
#48303 = EDGE_CURVE ( 'NONE', #18993, #17406, #14810, .T. ) ;
#48304 = VERTEX_POINT ( 'NONE', #25006 ) ;
#48305 = VECTOR ( 'NONE', #35376, 999.9999999999998863 ) ;
#48306 = DIRECTION ( 'NONE',  ( 0.000000000000000000, 0.000000000000000000, -1.000000000000000000 ) ) ;
#48307 = VECTOR ( 'NONE', #516, 1000.000000000000000 ) ;
#48308 = DIRECTION ( 'NONE',  ( 0.9266896074318317078, 0.000000000000000000, 0.3758275821142421647 ) ) ;
#48309 = AXIS2_PLACEMENT_3D ( 'NONE', #28334, #28587, #44631 ) ;
#48310 = EDGE_CURVE ( 'NONE', #33612, #4373, #1335, .T. ) ;
#48311 = CIRCLE ( 'NONE', #19752, 60.00000000000000000 ) ;
#48312 = DIRECTION ( 'NONE',  ( 0.2920567706369764371, 0.000000000000000000, -0.9564009842765223146 ) ) ;
#48313 = LINE ( 'NONE', #12294, #39028 ) ;
#48314 = ORIENTED_EDGE ( 'NONE', *, *, #39268, .F. ) ;
#48317 = ORIENTED_EDGE ( 'NONE', *, *, #40944, .T. ) ;
#48316 = CARTESIAN_POINT ( 'NONE',  ( -332.3517673607765914, -106.8245764869328980, 56.65561927337994064 ) ) ;
#48315 = FACE_OUTER_BOUND ( 'NONE', #22527, .T. ) ;
#48318 = VERTEX_POINT ( 'NONE', #5828 ) ;
#48319 = LINE ( 'NONE', #16795, #7195 ) ;
#48320 = ORIENTED_EDGE ( 'NONE', *, *, #31759, .T. ) ;
#48321 = LINE ( 'NONE', #35702, #3797 ) ;
#48322 = ORIENTED_EDGE ( 'NONE', *, *, #49101, .F. ) ;
#48323 = EDGE_CURVE ( 'NONE', #21876, #37521, #13176, .T. ) ;
#48324 = PLANE ( 'NONE',  #35100 ) ;
#48325 = ORIENTED_EDGE ( 'NONE', *, *, #26501, .T. ) ;
#48327 = DIRECTION ( 'NONE',  ( 1.043714542225393223E-14, -0.9927088740980544168, -0.1205366802553199113 ) ) ;
#48326 = CARTESIAN_POINT ( 'NONE',  ( -154.6193097927903182, -193.5000000000000000, -66.02470404298122730 ) ) ;
#48328 = EDGE_LOOP ( 'NONE', ( #42931, #7344, #46371, #9512 ) ) ;
#48329 = EDGE_CURVE ( 'NONE', #49227, #17596, #37608, .T. ) ;
#48330 = ORIENTED_EDGE ( 'NONE', *, *, #38741, .F. ) ;
#48331 = CYLINDRICAL_SURFACE ( 'NONE', #13639, 125.0000000000000000 ) ;
#48332 = EDGE_CURVE ( 'NONE', #31941, #18024, #45249, .T. ) ;
#48333 = VECTOR ( 'NONE', #21786, 1000.000000000000000 ) ;
#48334 = DIRECTION ( 'NONE',  ( 0.000000000000000000, -1.000000000000000000, 0.000000000000000000 ) ) ;
#48335 = LINE ( 'NONE', #3931, #7884 ) ;
#48336 = CARTESIAN_POINT ( 'NONE',  ( -330.4913330509368166, -68.15673923803900891, 20.45418021416622878 ) ) ;
#48337 = CARTESIAN_POINT ( 'NONE',  ( -146.0653709326077490, -193.5000000000000000, -78.11481899503411341 ) ) ;
#48338 = VECTOR ( 'NONE', #40747, 999.9999999999998863 ) ;
#48339 = FACE_OUTER_BOUND ( 'NONE', #20729, .T. ) ;
#48340 = VECTOR ( 'NONE', #47581, 1000.000000000000114 ) ;
#48341 = ORIENTED_EDGE ( 'NONE', *, *, #48592, .F. ) ;
#48342 = CARTESIAN_POINT ( 'NONE',  ( 0.000000000000000000, -68.33404168156053515, -20.92168833550964990 ) ) ;
#48343 = DIRECTION ( 'NONE',  ( 0.000000000000000000, 0.000000000000000000, -1.000000000000000000 ) ) ;
#48344 = PLANE ( 'NONE',  #9496 ) ;
#48345 = VERTEX_POINT ( 'NONE', #36829 ) ;
#48346 = DIRECTION ( 'NONE',  ( 0.6965510290630033685, 0.000000000000000000, -0.7175072570443249420 ) ) ;
#48347 = AXIS2_PLACEMENT_3D ( 'NONE', #19243, #39960, #31309 ) ;
#48348 = EDGE_CURVE ( 'NONE', #44602, #38839, #16863, .T. ) ;
#48349 = AXIS2_PLACEMENT_3D ( 'NONE', #5949, #23518, #36116 ) ;
#48350 = CARTESIAN_POINT ( 'NONE',  ( 48.69345348225013481, -175.3837268820161057, -78.62880929222873760 ) ) ;
#48351 = DIRECTION ( 'NONE',  ( 1.000000000000000000, -0.000000000000000000, -0.000000000000000000 ) ) ;
#48352 = ORIENTED_EDGE ( 'NONE', *, *, #18447, .F. ) ;
#48353 = ORIENTED_EDGE ( 'NONE', *, *, #33375, .T. ) ;
#48354 = VECTOR ( 'NONE', #7362, 1000.000000000000000 ) ;
#48355 = VERTEX_POINT ( 'NONE', #41809 ) ;
#48356 = AXIS2_PLACEMENT_3D ( 'NONE', #18545, #34559, #1484 ) ;
#48357 = CARTESIAN_POINT ( 'NONE',  ( 76.37123734610607073, -193.5000000000000000, 6.114457023561876703 ) ) ;
#48358 = CARTESIAN_POINT ( 'NONE',  ( -46.00000000000000711, 20.00000000000000000, 8.673617379884035472E-15 ) ) ;
#48359 = DIRECTION ( 'NONE',  ( 0.8610436117673514467, 0.000000000000000000, 0.5085311186492273983 ) ) ;
#48360 = PLANE ( 'NONE',  #25400 ) ;
#48361 = ORIENTED_EDGE ( 'NONE', *, *, #1863, .T. ) ;
#48362 = CARTESIAN_POINT ( 'NONE',  ( 32.99469856375238663, -193.5000000000000000, 94.79987230212020677 ) ) ;
#48363 = ORIENTED_EDGE ( 'NONE', *, *, #51641, .T. ) ;
#48364 = ORIENTED_EDGE ( 'NONE', *, *, #36239, .F. ) ;
#48365 = CIRCLE ( 'NONE', #11432, 15.24495751795539000 ) ;
#48366 = AXIS2_PLACEMENT_3D ( 'NONE', #14411, #45969, #29646 ) ;
#48367 = ORIENTED_EDGE ( 'NONE', *, *, #26037, .T. ) ;
#48368 = CARTESIAN_POINT ( 'NONE',  ( -49.38192458147459973, -193.5000000000000000, 0.4300652022765185656 ) ) ;
#48369 = AXIS2_PLACEMENT_3D ( 'NONE', #18923, #50232, #10267 ) ;
#48370 = ADVANCED_FACE ( 'NONE', ( #41019 ), #4769, .F. ) ;
#48371 = EDGE_CURVE ( 'NONE', #13513, #45342, #49693, .T. ) ;
#48372 = CARTESIAN_POINT ( 'NONE',  ( -49.47868758801764955, -189.7472609257535510, 0.02963332782255607284 ) ) ;
#48373 = DIRECTION ( 'NONE',  ( -1.000000000000000000, 0.000000000000000000, 0.000000000000000000 ) ) ;
#48376 = VERTEX_POINT ( 'NONE', #37071 ) ;
#48375 = DIRECTION ( 'NONE',  ( 0.000000000000000000, 0.000000000000000000, -1.000000000000000000 ) ) ;
#48374 = PLANE ( 'NONE',  #48480 ) ;
#48377 = CIRCLE ( 'NONE', #9903, 60.00000000000000000 ) ;
#48378 = AXIS2_PLACEMENT_3D ( 'NONE', #21403, #45339, #37426 ) ;
#48379 = VECTOR ( 'NONE', #13835, 1000.000000000000000 ) ;
#48380 = FACE_OUTER_BOUND ( 'NONE', #16777, .T. ) ;
#48382 = ORIENTED_EDGE ( 'NONE', *, *, #29189, .T. ) ;
#48381 = AXIS2_PLACEMENT_3D ( 'NONE', #33074, #30176, #45966 ) ;
#48383 = CARTESIAN_POINT ( 'NONE',  ( 55.35935253854128035, -183.6283474603465606, 69.58857822035041352 ) ) ;
#48384 = EDGE_LOOP ( 'NONE', ( #51621, #35476, #1835, #30549 ) ) ;
#48385 = CARTESIAN_POINT ( 'NONE',  ( -16.77927958806651887, -193.5000000000000000, -120.9136869416130082 ) ) ;
#48386 = EDGE_CURVE ( 'NONE', #9307, #44982, #38266, .T. ) ;
#48387 = VECTOR ( 'NONE', #670, 1000.000000000000000 ) ;
#48388 = DIRECTION ( 'NONE',  ( -0.000000000000000000, -0.9709418174260502354, 0.2393156642875652051 ) ) ;
#48390 = DIRECTION ( 'NONE',  ( -0.000000000000000000, 1.000000000000000000, -0.000000000000000000 ) ) ;
#48389 = DIRECTION ( 'NONE',  ( -0.000000000000000000, 1.000000000000000000, -0.000000000000000000 ) ) ;
#48391 = ORIENTED_EDGE ( 'NONE', *, *, #14447, .T. ) ;
#48392 = EDGE_CURVE ( 'NONE', #38149, #3363, #21586, .T. ) ;
#48393 = VECTOR ( 'NONE', #47099, 1000.000000000000000 ) ;
#48394 = LINE ( 'NONE', #28403, #18161 ) ;
#48395 = DIRECTION ( 'NONE',  ( 0.4300652022765115712, 0.000000000000000000, 0.9027978299657477557 ) ) ;
#48396 = EDGE_CURVE ( 'NONE', #3624, #25977, #37444, .T. ) ;
#48397 = DIRECTION ( 'NONE',  ( 0.9785564922995060311, 0.000000000000000000, -0.2059786187410889424 ) ) ;
#48398 = ORIENTED_EDGE ( 'NONE', *, *, #20491, .T. ) ;
#48399 = AXIS2_PLACEMENT_3D ( 'NONE', #31492, #15220, #39373 ) ;
#48400 = FACE_OUTER_BOUND ( 'NONE', #5552, .T. ) ;
#48401 = DIRECTION ( 'NONE',  ( -0.6528221181905119463, 0.000000000000000000, -0.7575112421616284619 ) ) ;
#48402 = FACE_OUTER_BOUND ( 'NONE', #51818, .T. ) ;
#48403 = ADVANCED_FACE ( 'NONE', ( #8971 ), #29705, .T. ) ;
#48404 = VERTEX_POINT ( 'NONE', #33131 ) ;
#48405 = CARTESIAN_POINT ( 'NONE',  ( -160.2705093830644216, -183.6283474603465606, -55.92572546981520532 ) ) ;
#48406 = CARTESIAN_POINT ( 'NONE',  ( -332.3517673607765914, -163.8460225846223466, -43.07972642080364523 ) ) ;
#48407 = EDGE_LOOP ( 'NONE', ( #34770, #11851, #5713, #30821 ) ) ;
#48408 = CARTESIAN_POINT ( 'NONE',  ( -305.0000000000000568, -157.9941932480463436, 49.09328500076600221 ) ) ;
#48409 = ORIENTED_EDGE ( 'NONE', *, *, #45266, .F. ) ;
#48410 = AXIS2_PLACEMENT_3D ( 'NONE', #16938, #8268, #25091 ) ;
#48411 = AXIS2_PLACEMENT_3D ( 'NONE', #45578, #6412, #50036 ) ;
#48412 = DIRECTION ( 'NONE',  ( -0.000000000000000000, 1.000000000000000000, -0.000000000000000000 ) ) ;
#48413 = CARTESIAN_POINT ( 'NONE',  ( 75.48825557695654709, -193.5000000000000000, 2.844930291601490246 ) ) ;
#48414 = VECTOR ( 'NONE', #51957, 1000.000000000000000 ) ;
#48415 = CARTESIAN_POINT ( 'NONE',  ( -71.40672220061269115, -193.5000000000000000, -122.8793122007208751 ) ) ;
#48416 = CARTESIAN_POINT ( 'NONE',  ( -49.17567778057185990, -193.5000000000000000, 0.7175072570443320474 ) ) ;
#48417 = CARTESIAN_POINT ( 'NONE',  ( -336.3521761649654422, -180.1556192733800117, 16.67542351306693149 ) ) ;
#48418 = CARTESIAN_POINT ( 'NONE',  ( -48.47912675150885065, -175.3837268820161057, 6.938893903907228378E-15 ) ) ;
#48419 = VECTOR ( 'NONE', #12225, 1000.000000000000114 ) ;
#48420 = CIRCLE ( 'NONE', #11448, 60.00000000000000000 ) ;
#48421 = DIRECTION ( 'NONE',  ( -0.000000000000000000, 1.000000000000000000, -0.000000000000000000 ) ) ;
#48422 = FACE_OUTER_BOUND ( 'NONE', #15856, .T. ) ;
#48424 = ORIENTED_EDGE ( 'NONE', *, *, #34889, .T. ) ;
#48423 = LINE ( 'NONE', #20550, #23656 ) ;
#48425 = CIRCLE ( 'NONE', #50950, 125.0000000000000000 ) ;
#48426 = ORIENTED_EDGE ( 'NONE', *, *, #11812, .T. ) ;
#48427 = FACE_OUTER_BOUND ( 'NONE', #14370, .T. ) ;
#48428 = VECTOR ( 'NONE', #823, 1000.000000000000000 ) ;
#48429 = VECTOR ( 'NONE', #50469, 1000.000000000000000 ) ;
#48430 = EDGE_CURVE ( 'NONE', #40405, #22679, #48665, .T. ) ;
#48431 = FACE_OUTER_BOUND ( 'NONE', #19171, .T. ) ;
#48432 = ORIENTED_EDGE ( 'NONE', *, *, #46741, .F. ) ;
#48433 = ORIENTED_EDGE ( 'NONE', *, *, #6416, .T. ) ;
#48434 = ORIENTED_EDGE ( 'NONE', *, *, #10648, .F. ) ;
#48435 = PLANE ( 'NONE',  #21672 ) ;
#48436 = EDGE_CURVE ( 'NONE', #49012, #47168, #21518, .T. ) ;
#48437 = EDGE_CURVE ( 'NONE', #47028, #41848, #7220, .T. ) ;
#48438 = ADVANCED_FACE ( 'NONE', ( #43087 ), #2884, .T. ) ;
#48439 = DIRECTION ( 'NONE',  ( 0.9266896074318317078, 0.000000000000000000, 0.3758275821142421647 ) ) ;
#48440 = DIRECTION ( 'NONE',  ( 0.000000000000000000, 0.000000000000000000, 1.000000000000000000 ) ) ;
#48441 = ORIENTED_EDGE ( 'NONE', *, *, #35058, .T. ) ;
#48442 = VERTEX_POINT ( 'NONE', #27047 ) ;
#48443 = ADVANCED_FACE ( 'NONE', ( #42054 ), #50730, .F. ) ;
#48444 = ORIENTED_EDGE ( 'NONE', *, *, #30331, .F. ) ;
#48445 = DIRECTION ( 'NONE',  ( -0.000000000000000000, 1.000000000000000000, -0.000000000000000000 ) ) ;
#48446 = CARTESIAN_POINT ( 'NONE',  ( 63.39453919430263085, -193.5000000000000000, 53.48161459190911415 ) ) ;
#48447 = CIRCLE ( 'NONE', #14884, 125.0000000000000000 ) ;
#48449 = VERTEX_POINT ( 'NONE', #46027 ) ;
#48448 = LINE ( 'NONE', #44238, #1452 ) ;
#48450 = VECTOR ( 'NONE', #15795, 1000.000000000000000 ) ;
#48451 = EDGE_CURVE ( 'NONE', #14774, #15949, #26797, .T. ) ;
#48452 = CARTESIAN_POINT ( 'NONE',  ( -56.71246971489870958, -193.5000000000000000, -124.7285535218267682 ) ) ;
#48453 = DIRECTION ( 'NONE',  ( 0.000000000000000000, 0.000000000000000000, 1.000000000000000000 ) ) ;
#48454 = ORIENTED_EDGE ( 'NONE', *, *, #6699, .F. ) ;
#48455 = FACE_OUTER_BOUND ( 'NONE', #8541, .T. ) ;
#48456 = VECTOR ( 'NONE', #11959, 1000.000000000000000 ) ;
#48457 = DIRECTION ( 'NONE',  ( 0.9993203489176063492, 0.000000000000000000, 0.03686245026030503941 ) ) ;
#48458 = EDGE_CURVE ( 'NONE', #7752, #6661, #26029, .T. ) ;
#48459 = CARTESIAN_POINT ( 'NONE',  ( -47.50057025920934706, -189.7472609257535510, -0.2059786187410884151 ) ) ;
#48460 = LINE ( 'NONE', #12437, #24909 ) ;
#48461 = EDGE_CURVE ( 'NONE', #5412, #19912, #6590, .T. ) ;
#48462 = EDGE_LOOP ( 'NONE', ( #3853, #17120, #40689, #45345 ) ) ;
#48463 = ORIENTED_EDGE ( 'NONE', *, *, #39737, .F. ) ;
#48464 = AXIS2_PLACEMENT_3D ( 'NONE', #31621, #44493, #47676 ) ;
#48465 = EDGE_LOOP ( 'NONE', ( #43749, #7624, #18975, #46414 ) ) ;
#48466 = CARTESIAN_POINT ( 'NONE',  ( 74.31448861501726810, -193.5000000000000000, -23.38221600314288651 ) ) ;
#48467 = EDGE_CURVE ( 'NONE', #246, #26523, #6321, .T. ) ;
#48468 = DIRECTION ( 'NONE',  ( -1.000000000000000000, 0.000000000000000000, 1.043714542225393381E-14 ) ) ;
#48469 = VECTOR ( 'NONE', #7898, 1000.000000000000227 ) ;
#48470 = EDGE_LOOP ( 'NONE', ( #24263, #42131, #13241, #17768 ) ) ;
#48471 = LINE ( 'NONE', #12176, #39137 ) ;
#48472 = CIRCLE ( 'NONE', #45139, 60.00000000000000000 ) ;
#48473 = EDGE_CURVE ( 'NONE', #25260, #32165, #47046, .T. ) ;
#48474 = DIRECTION ( 'NONE',  ( -0.9995608365087946812, 0.000000000000000000, 0.02963332782254913048 ) ) ;
#48475 = ORIENTED_EDGE ( 'NONE', *, *, #37399, .T. ) ;
#48476 = DIRECTION ( 'NONE',  ( -0.000000000000000000, -0.9927088740980530845, 0.1205366802553303057 ) ) ;
#48477 = VECTOR ( 'NONE', #20267, 1000.000000000000000 ) ;
#48478 = EDGE_CURVE ( 'NONE', #22578, #10499, #6067, .T. ) ;
#48479 = PLANE ( 'NONE',  #18870 ) ;
#48480 = AXIS2_PLACEMENT_3D ( 'NONE', #24203, #274, #3438 ) ;
#48481 = ORIENTED_EDGE ( 'NONE', *, *, #35937, .T. ) ;
#48482 = CARTESIAN_POINT ( 'NONE',  ( -48.47912675150885065, -183.6283474603465606, 6.938893903907228378E-15 ) ) ;
#48483 = EDGE_LOOP ( 'NONE', ( #33936, #19950, #38981, #45351 ) ) ;
#48484 = FACE_BOUND ( 'NONE', #1554, .T. ) ;
#48485 = CARTESIAN_POINT ( 'NONE',  ( -336.3521761649654422, -159.1821513111375452, -47.06073758877369073 ) ) ;
#48486 = VERTEX_POINT ( 'NONE', #46790 ) ;
#48487 = DIRECTION ( 'NONE',  ( -0.000000000000000000, 1.000000000000000000, -0.000000000000000000 ) ) ;
#48488 = DIRECTION ( 'NONE',  ( 0.000000000000000000, 1.000000000000000000, 0.000000000000000000 ) ) ;
#48489 = DIRECTION ( 'NONE',  ( 0.000000000000000000, 1.000000000000000000, 0.000000000000000000 ) ) ;
#48490 = DIRECTION ( 'NONE',  ( 0.000000000000000000, 0.6631226582407937498, -0.7485107481711024136 ) ) ;
#48491 = EDGE_CURVE ( 'NONE', #41165, #16448, #2384, .T. ) ;
#48492 = ORIENTED_EDGE ( 'NONE', *, *, #33148, .T. ) ;
#48493 = FACE_OUTER_BOUND ( 'NONE', #5753, .T. ) ;
#48494 = ORIENTED_EDGE ( 'NONE', *, *, #10450, .F. ) ;
#48495 = ORIENTED_EDGE ( 'NONE', *, *, #44539, .T. ) ;
#48496 = AXIS2_PLACEMENT_3D ( 'NONE', #45045, #25835, #40810 ) ;
#48497 = AXIS2_PLACEMENT_3D ( 'NONE', #16537, #44905, #20727 ) ;
#48498 = CARTESIAN_POINT ( 'NONE',  ( -332.3517673607765914, -142.8954717479169574, 55.74477592174805096 ) ) ;
#48500 = ORIENTED_EDGE ( 'NONE', *, *, #41879, .T. ) ;
#48499 = CARTESIAN_POINT ( 'NONE',  ( 4.951097822533392803E-16, 48.00406676456095312, -15.93472476940568860 ) ) ;
#48501 = VECTOR ( 'NONE', #11891, 999.9999999999998863 ) ;
#48502 = ORIENTED_EDGE ( 'NONE', *, *, #368, .F. ) ;
#48503 = PLANE ( 'NONE',  #30324 ) ;
#48504 = EDGE_CURVE ( 'NONE', #42645, #48757, #46526, .T. ) ;
#48505 = DIRECTION ( 'NONE',  ( -0.000000000000000000, -0.4647231720437695057, -0.8854560256532093554 ) ) ;
#48506 = VECTOR ( 'NONE', #28249, 1000.000000000000000 ) ;
#48507 = ORIENTED_EDGE ( 'NONE', *, *, #48982, .F. ) ;
#48508 = DIRECTION ( 'NONE',  ( -1.000000000000000000, 0.000000000000000000, -0.000000000000000000 ) ) ;
#48509 = ORIENTED_EDGE ( 'NONE', *, *, #25647, .F. ) ;
#48510 = LINE ( 'NONE', #15926, #663 ) ;
#48511 = CARTESIAN_POINT ( 'NONE',  ( -78.64590280292341617, -193.5000000000000000, -121.3052580173827408 ) ) ;
#48512 = AXIS2_PLACEMENT_3D ( 'NONE', #12955, #627, #4567 ) ;
#48513 = EDGE_CURVE ( 'NONE', #43312, #11444, #22862, .T. ) ;
#48514 = ADVANCED_FACE ( 'NONE', ( #18150 ), #34177, .F. ) ;
#48515 = CARTESIAN_POINT ( 'NONE',  ( -336.3521761649654422, -152.3639871485048900, -51.48334306143194539 ) ) ;
#48516 = DIRECTION ( 'NONE',  ( 0.000000000000000000, -0.000000000000000000, 1.000000000000000000 ) ) ;
#48517 = VERTEX_POINT ( 'NONE', #37853 ) ;
#48518 = ORIENTED_EDGE ( 'NONE', *, *, #45894, .F. ) ;
#48519 = ADVANCED_FACE ( 'NONE', ( #10778 ), #6836, .T. ) ;
#48520 = VERTEX_POINT ( 'NONE', #14471 ) ;
#48521 = VECTOR ( 'NONE', #43070, 1000.000000000000114 ) ;
#48522 = EDGE_CURVE ( 'NONE', #33847, #16474, #16454, .T. ) ;
#48523 = CARTESIAN_POINT ( 'NONE',  ( -48.82732838694325750, -177.1207230881787780, 0.9374196611341252261 ) ) ;
#48524 = LINE ( 'NONE', #31947, #41104 ) ;
#48525 = DIRECTION ( 'NONE',  ( -0.000000000000000000, -1.000000000000000000, 0.000000000000000000 ) ) ;
#48526 = FACE_BOUND ( 'NONE', #27889, .T. ) ;
#48527 = CARTESIAN_POINT ( 'NONE',  ( -77.03256798524179771, -189.7472609257535510, 121.6951149130964751 ) ) ;
#48528 = ORIENTED_EDGE ( 'NONE', *, *, #29496, .F. ) ;
#48529 = ORIENTED_EDGE ( 'NONE', *, *, #43123, .F. ) ;
#48531 = ORIENTED_EDGE ( 'NONE', *, *, #16467, .T. ) ;
#48530 = DIRECTION ( 'NONE',  ( 0.4566292373937200777, 0.000000000000000000, -0.8896570909947436601 ) ) ;
#48532 = LINE ( 'NONE', #12510, #29664 ) ;
#48533 = AXIS2_PLACEMENT_3D ( 'NONE', #11337, #32342, #19488 ) ;
#48534 = VERTEX_POINT ( 'NONE', #1849 ) ;
#48535 = AXIS2_PLACEMENT_3D ( 'NONE', #15178, #47492, #50660 ) ;
#48536 = EDGE_CURVE ( 'NONE', #11081, #29368, #17893, .T. ) ;
#48537 = DIRECTION ( 'NONE',  ( 1.043714542225393223E-14, -0.3546048870425363986, -0.9350162426854146114 ) ) ;
#48538 = DIRECTION ( 'NONE',  ( -0.000000000000000000, 0.8229838658936556861, -0.5680647467311569221 ) ) ;
#48539 = CIRCLE ( 'NONE', #15793, 125.0000000000000000 ) ;
#48540 = DIRECTION ( 'NONE',  ( 1.043714542225393223E-14, 0.5680647467311626952, 0.8229838658936516893 ) ) ;
#48541 = DIRECTION ( 'NONE',  ( -1.000000000000000000, 0.000000000000000000, 0.000000000000000000 ) ) ;
#48542 = ORIENTED_EDGE ( 'NONE', *, *, #41028, .T. ) ;
#48543 = CARTESIAN_POINT ( 'NONE',  ( -170.9948556092908518, -189.7472609257535510, 19.12855698118476511 ) ) ;
#48544 = ORIENTED_EDGE ( 'NONE', *, *, #1381, .T. ) ;
#48545 = ADVANCED_FACE ( 'NONE', ( #12047 ), #15779, .T. ) ;
#48546 = ORIENTED_EDGE ( 'NONE', *, *, #47554, .T. ) ;
#48547 = DIRECTION ( 'NONE',  ( -0.000000000000000000, 1.000000000000000000, -0.000000000000000000 ) ) ;
#48548 = AXIS2_PLACEMENT_3D ( 'NONE', #49924, #9208, #22313 ) ;
#48549 = DIRECTION ( 'NONE',  ( 0.000000000000000000, 0.000000000000000000, -1.000000000000000000 ) ) ;
#48550 = DIRECTION ( 'NONE',  ( 0.000000000000000000, 1.000000000000000000, 0.000000000000000000 ) ) ;
#48551 = CARTESIAN_POINT ( 'NONE',  ( -330.4913330509368166, -116.8846903019851311, -58.63009191191288494 ) ) ;
#48552 = CARTESIAN_POINT ( 'NONE',  ( -63.43218022845228887, -175.3837268820161057, 124.1024020384604540 ) ) ;
#48553 = LINE ( 'NONE', #21192, #17011 ) ;
#48554 = ORIENTED_EDGE ( 'NONE', *, *, #29964, .T. ) ;
#48555 = CARTESIAN_POINT ( 'NONE',  ( -148.0127667507368585, -177.1207230881787780, -75.61781872352626976 ) ) ;
#48556 = DIRECTION ( 'NONE',  ( 0.000000000000000000, 0.2393156642875516049, -0.9709418174260534551 ) ) ;
#48557 = CARTESIAN_POINT ( 'NONE',  ( -48.65601702663141737, -189.7472609257535510, -0.9842305779475923888 ) ) ;
#48558 = FACE_BOUND ( 'NONE', #3121, .T. ) ;
#48559 = ORIENTED_EDGE ( 'NONE', *, *, #34651, .T. ) ;
#48560 = LINE ( 'NONE', #24616, #30649 ) ;
#48561 = LINE ( 'NONE', #28555, #16913 ) ;
#48562 = VERTEX_POINT ( 'NONE', #51253 ) ;
#48563 = DIRECTION ( 'NONE',  ( 0.000000000000000000, -1.000000000000000000, 0.000000000000000000 ) ) ;
#48564 = ORIENTED_EDGE ( 'NONE', *, *, #28772, .T. ) ;
#48565 = PRODUCT_DEFINITION_FORMATION_WITH_SPECIFIED_SOURCE ( 'ANY', '', #13844, .NOT_KNOWN. ) ;
#48566 = CARTESIAN_POINT ( 'NONE',  ( -339.1964088526558498, -67.57827586672145515, 21.74306257088659677 ) ) ;
#48567 = VECTOR ( 'NONE', #28214, 1000.000000000000000 ) ;
#48568 = CIRCLE ( 'NONE', #31789, 125.0000000000000000 ) ;
#48569 = PLANE ( 'NONE',  #46110 ) ;
#48571 = ORIENTED_EDGE ( 'NONE', *, *, #46548, .T. ) ;
#48570 = CARTESIAN_POINT ( 'NONE',  ( -330.4913330509368166, -65.36517161715283919, -14.84391218300977400 ) ) ;
#48572 = VECTOR ( 'NONE', #26831, 1000.000000000000000 ) ;
#48573 = EDGE_CURVE ( 'NONE', #6375, #19121, #8125, .T. ) ;
#48574 = ADVANCED_FACE ( 'NONE', ( #35713 ), #43607, .T. ) ;
#48575 = DIRECTION ( 'NONE',  ( -0.000000000000000000, 1.000000000000000000, -0.000000000000000000 ) ) ;
#48576 = ORIENTED_EDGE ( 'NONE', *, *, #33618, .T. ) ;
#48577 = EDGE_LOOP ( 'NONE', ( #45725, #27974, #32524, #40064 ) ) ;
#48578 = PLANE ( 'NONE',  #14183 ) ;
#48579 = AXIS2_PLACEMENT_3D ( 'NONE', #733, #24138, #23856 ) ;
#48580 = ORIENTED_EDGE ( 'NONE', *, *, #39240, .F. ) ;
#48581 = DIRECTION ( 'NONE',  ( 0.000000000000000000, 0.000000000000000000, 1.000000000000000000 ) ) ;
#48582 = DIRECTION ( 'NONE',  ( -0.000000000000000000, 1.000000000000000000, -0.000000000000000000 ) ) ;
#48583 = DIRECTION ( 'NONE',  ( 0.9960498426152165630, 0.000000000000000000, 0.08879589532293852283 ) ) ;
#48584 = AXIS2_PLACEMENT_3D ( 'NONE', #29635, #5488, #41982 ) ;
#48585 = CARTESIAN_POINT ( 'NONE',  ( -336.3521761649653854, -164.4944191672036311, -43.81161486573634534 ) ) ;
#48586 = LINE ( 'NONE', #16787, #2956 ) ;
#48587 = EDGE_LOOP ( 'NONE', ( #45711, #12873, #35885, #48819 ) ) ;
#48590 = ORIENTED_EDGE ( 'NONE', *, *, #13438, .T. ) ;
#48589 = DIRECTION ( 'NONE',  ( -1.000000000000000000, -0.000000000000000000, 0.000000000000000000 ) ) ;
#48588 = PLANE ( 'NONE',  #36603 ) ;
#48591 = ORIENTED_EDGE ( 'NONE', *, *, #7030, .T. ) ;
#48592 = EDGE_CURVE ( 'NONE', #41107, #30895, #3929, .T. ) ;
#48593 = CARTESIAN_POINT ( 'NONE',  ( 33.75048693540708911, -193.5000000000000000, 94.14505102712816154 ) ) ;
#48594 = VERTEX_POINT ( 'NONE', #28347 ) ;
#48595 = PLANE ( 'NONE',  #8820 ) ;
#48596 = ORIENTED_EDGE ( 'NONE', *, *, #36716, .F. ) ;
#48597 = CARTESIAN_POINT ( 'NONE',  ( -169.0855799822425638, -183.6283474603465606, -28.81338593823979011 ) ) ;
#48598 = CARTESIAN_POINT ( 'NONE',  ( 70.19984492582109681, -189.7472609257535510, 39.24667733211968823 ) ) ;
#48599 = ORIENTED_EDGE ( 'NONE', *, *, #30163, .T. ) ;
#48601 = LINE ( 'NONE', #36760, #49317 ) ;
#48600 = FACE_OUTER_BOUND ( 'NONE', #36889, .T. ) ;
#48602 = ORIENTED_EDGE ( 'NONE', *, *, #33614, .T. ) ;
#48603 = ADVANCED_FACE ( 'NONE', ( #7858 ), #15238, .T. ) ;
#48604 = ORIENTED_EDGE ( 'NONE', *, *, #1216, .F. ) ;
#48605 = LINE ( 'NONE', #19953, #36280 ) ;
#48606 = CARTESIAN_POINT ( 'NONE',  ( -336.3521761649654422, -174.5186198893880771, 29.74944317415823392 ) ) ;
#48607 = VECTOR ( 'NONE', #24689, 1000.000000000000000 ) ;
#48608 = CARTESIAN_POINT ( 'NONE',  ( -49.35486169370448550, -189.7472609257535510, -0.4827922027307481878 ) ) ;
#48609 = DIRECTION ( 'NONE',  ( -0.000000000000000000, 0.9350162426854146114, -0.3546048870425363986 ) ) ;
#48610 = CARTESIAN_POINT ( 'NONE',  ( -172.2289551866394106, -175.3837268820161057, -17.63462396184707970 ) ) ;
#48611 = AXIS2_PLACEMENT_3D ( 'NONE', #23858, #52006, #15995 ) ;
#48612 = CARTESIAN_POINT ( 'NONE',  ( 30.00000000000000711, -43.50000000000000000, 30.00000000000000355 ) ) ;
#48613 = CONTEXT_DEPENDENT_SHAPE_REPRESENTATION ( #10870, #18477 ) ;
#48614 = CARTESIAN_POINT ( 'NONE',  ( -339.1964088526558498, -162.9984922102927385, -43.83057281297435992 ) ) ;
#48615 = EDGE_CURVE ( 'NONE', #12206, #14876, #16269, .T. ) ;
#48616 = DIRECTION ( 'NONE',  ( 0.9960498426152171181, 0.000000000000000000, -0.08879589532293157006 ) ) ;
#48617 = FACE_OUTER_BOUND ( 'NONE', #37508, .T. ) ;
#48618 = LINE ( 'NONE', #12591, #35806 ) ;
#48619 = EDGE_LOOP ( 'NONE', ( #15870, #3357, #1447, #33806, #29694, #8032, #12079, #19675 ) ) ;
#48620 = AXIS2_PLACEMENT_3D ( 'NONE', #9135, #20961, #49071 ) ;
#48621 = ORIENTED_EDGE ( 'NONE', *, *, #20174, .F. ) ;
#48622 = CARTESIAN_POINT ( 'NONE',  ( -168.3100285466275636, -175.3837268820161057, -31.88354567335001377 ) ) ;
#48623 = DIRECTION ( 'NONE',  ( -0.000000000000000000, -1.000000000000000000, 0.000000000000000000 ) ) ;
#48624 = DIRECTION ( 'NONE',  ( -0.000000000000000000, 1.000000000000000000, -0.000000000000000000 ) ) ;
#48625 = ORIENTED_EDGE ( 'NONE', *, *, #29862, .F. ) ;
#48626 = VERTEX_POINT ( 'NONE', #47824 ) ;
#48627 = ORIENTED_EDGE ( 'NONE', *, *, #30449, .T. ) ;
#48628 = CIRCLE ( 'NONE', #40227, 125.0000000000000000 ) ;
#48629 = ADVANCED_FACE ( 'NONE', ( #39901 ), #19683, .F. ) ;
#48630 = FACE_OUTER_BOUND ( 'NONE', #8783, .T. ) ;
#48631 = CARTESIAN_POINT ( 'NONE',  ( -48.47912675150885065, -189.7472609257535510, 6.938893903907228378E-15 ) ) ;
#48632 = CARTESIAN_POINT ( 'NONE',  ( 0.000000000000000000, -79.33786585790457480, 39.12423683620640702 ) ) ;
#48633 = DIRECTION ( 'NONE',  ( 0.000000000000000000, -1.000000000000000000, 0.000000000000000000 ) ) ;
#48634 = ORIENTED_EDGE ( 'NONE', *, *, #7982, .T. ) ;
#48635 = LINE ( 'NONE', #36517, #19930 ) ;
#48636 = ADVANCED_FACE ( 'NONE', ( #7365 ), #52035, .T. ) ;
#48637 = EDGE_CURVE ( 'NONE', #975, #12201, #13106, .T. ) ;
#48638 = CARTESIAN_POINT ( 'NONE',  ( -48.47912675150885065, -183.6283474603465606, 6.938893903907228378E-15 ) ) ;
#48639 = VERTEX_POINT ( 'NONE', #23125 ) ;
#48640 = PLANE ( 'NONE',  #37381 ) ;
#48641 = ORIENTED_EDGE ( 'NONE', *, *, #904, .T. ) ;
#48642 = EDGE_CURVE ( 'NONE', #36663, #2925, #23387, .T. ) ;
#48643 = VECTOR ( 'NONE', #3555, 1000.000000000000000 ) ;
#48644 = EDGE_LOOP ( 'NONE', ( #26380, #10572, #18069, #5074 ) ) ;
#48645 = CARTESIAN_POINT ( 'NONE',  ( 48.06131630543706024, -175.3837268820161057, -79.40367028273054473 ) ) ;
#48646 = VECTOR ( 'NONE', #8305, 1000.000000000000000 ) ;
#48647 = LINE ( 'NONE', #28383, #25044 ) ;
#48648 = CARTESIAN_POINT ( 'NONE',  ( -305.0000000000000568, -116.7644047441732340, -59.62073260661667717 ) ) ;
#48651 = ORIENTED_EDGE ( 'NONE', *, *, #33863, .T. ) ;
#48650 = LINE ( 'NONE', #20779, #35883 ) ;
#48649 = CARTESIAN_POINT ( 'NONE',  ( -339.1964088526558498, -64.86990808808704401, 6.615309698014191220 ) ) ;
#48652 = EDGE_CURVE ( 'NONE', #13513, #3372, #48068, .T. ) ;
#48653 = FACE_OUTER_BOUND ( 'NONE', #4589, .T. ) ;
#48654 = ORIENTED_EDGE ( 'NONE', *, *, #51902, .T. ) ;
#48655 = DIRECTION ( 'NONE',  ( 0.000000000000000000, -1.000000000000000000, 0.000000000000000000 ) ) ;
#48656 = LINE ( 'NONE', #811, #20757 ) ;
#48657 = ORIENTED_EDGE ( 'NONE', *, *, #30693, .F. ) ;
#48658 = PLANE ( 'NONE',  #14030 ) ;
#48659 = DIRECTION ( 'NONE',  ( -0.1768902751225802927, 0.000000000000000000, 0.9842305779475953864 ) ) ;
#48661 = CARTESIAN_POINT ( 'NONE',  ( -47.48307690889363641, -193.5000000000000000, -0.08879589532292464504 ) ) ;
#48660 = DIRECTION ( 'NONE',  ( 0.000000000000000000, -1.000000000000000000, 0.000000000000000000 ) ) ;
#48662 = VECTOR ( 'NONE', #15937, 999.9999999999998863 ) ;
#48663 = DIRECTION ( 'NONE',  ( -0.9266896074318343723, 0.000000000000000000, 0.3758275821142357809 ) ) ;
#48664 = DIRECTION ( 'NONE',  ( -1.000000000000000000, 0.000000000000000000, -0.000000000000000000 ) ) ;
#48665 = LINE ( 'NONE', #28658, #49206 ) ;
#48666 = ORIENTED_EDGE ( 'NONE', *, *, #12465, .F. ) ;
#48667 = DIRECTION ( 'NONE',  ( 0.000000000000000000, 0.000000000000000000, 1.000000000000000000 ) ) ;
#48668 = CARTESIAN_POINT ( 'NONE',  ( -99.02518858244150124, -175.3837268820161057, 114.3245189510261497 ) ) ;
#48669 = DIRECTION ( 'NONE',  ( -0.000000000000000000, -1.000000000000000000, 0.000000000000000000 ) ) ;
#48670 = VERTEX_POINT ( 'NONE', #39138 ) ;
#48671 = DIRECTION ( 'NONE',  ( 1.000000000000000000, 0.000000000000000000, 0.000000000000000000 ) ) ;
#48672 = EDGE_LOOP ( 'NONE', ( #44630, #23953, #3864, #10679 ) ) ;
#48673 = CARTESIAN_POINT ( 'NONE',  ( -99.62791064391784346, -193.5000000000000000, -114.0561348912352173 ) ) ;
#48674 = VERTEX_POINT ( 'NONE', #20209 ) ;
#48675 = AXIS2_PLACEMENT_3D ( 'NONE', #30204, #29937, #2071 ) ;
#48676 = CARTESIAN_POINT ( 'NONE',  ( 46.00000000000000711, 20.00000000000000000, -51.00000000000000000 ) ) ;
#48677 = DIRECTION ( 'NONE',  ( 0.000000000000000000, -7.193320013717159664E-14, 1.000000000000000000 ) ) ;
#48678 = DIRECTION ( 'NONE',  ( 0.000000000000000000, 0.000000000000000000, -1.000000000000000000 ) ) ;
#48679 = ADVANCED_FACE ( 'NONE', ( #36230 ), #32282, .T. ) ;
#48680 = DIRECTION ( 'NONE',  ( -1.000000000000000000, 0.000000000000000000, -0.000000000000000000 ) ) ;
#48681 = CARTESIAN_POINT ( 'NONE',  ( 3.686287386450715076E-15, 0.000000000000000000, -46.00000000000000711 ) ) ;
#48682 = CARTESIAN_POINT ( 'NONE',  ( -89.73513343757494454, -183.6283474603465606, -117.9955164924467397 ) ) ;
#48683 = CARTESIAN_POINT ( 'NONE',  ( -332.3517673607765914, -65.58448481710581746, 11.56382487286456140 ) ) ;
#48684 = CARTESIAN_POINT ( 'NONE',  ( -154.6193097927903182, -189.7472609257535510, -66.02470404298122730 ) ) ;
#48686 = ORIENTED_EDGE ( 'NONE', *, *, #31065, .T. ) ;
#48685 = DIRECTION ( 'NONE',  ( -0.000000000000000000, 1.000000000000000000, -0.000000000000000000 ) ) ;
#48687 = VERTEX_POINT ( 'NONE', #12315 ) ;
#48688 = FACE_OUTER_BOUND ( 'NONE', #29386, .T. ) ;
#48689 = ADVANCED_FACE ( 'NONE', ( #3149 ), #19429, .F. ) ;
#48690 = EDGE_CURVE ( 'NONE', #3147, #25168, #28165, .T. ) ;
#48691 = AXIS2_PLACEMENT_3D ( 'NONE', #34783, #46382, #23493 ) ;
#48692 = CIRCLE ( 'NONE', #26025, 60.00000000000000000 ) ;
#48693 = DIRECTION ( 'NONE',  ( 0.000000000000000000, 0.000000000000000000, -1.000000000000000000 ) ) ;
#48694 = VERTEX_POINT ( 'NONE', #37276 ) ;
#48695 = VERTEX_POINT ( 'NONE', #13622 ) ;
#48696 = EDGE_CURVE ( 'NONE', #3020, #13909, #24018, .T. ) ;
#48697 = ORIENTED_EDGE ( 'NONE', *, *, #5775, .T. ) ;
#48698 = CARTESIAN_POINT ( 'NONE',  ( -336.3521761649654422, -111.9361751271348879, -57.91551518289410438 ) ) ;
#48699 = DIRECTION ( 'NONE',  ( 0.000000000000000000, 0.2393156642875685913, 0.9709418174260493473 ) ) ;
#48700 = DIRECTION ( 'NONE',  ( -1.000000000000000000, 9.758900497077185133E-15, 3.701062773504781726E-15 ) ) ;
#48701 = ORIENTED_EDGE ( 'NONE', *, *, #17622, .T. ) ;
#48702 = VERTEX_POINT ( 'NONE', #44398 ) ;
#48703 = LINE ( 'NONE', #44754, #8159 ) ;
#48704 = DIRECTION ( 'NONE',  ( -0.000000000000000000, 1.000000000000000000, -0.000000000000000000 ) ) ;
#48706 = ORIENTED_EDGE ( 'NONE', *, *, #20569, .F. ) ;
#48705 = DIRECTION ( 'NONE',  ( 0.000000000000000000, 0.000000000000000000, -1.000000000000000000 ) ) ;
#48707 = CIRCLE ( 'NONE', #3374, 125.0000000000000000 ) ;
#48708 = DIRECTION ( 'NONE',  ( 0.000000000000000000, 1.000000000000000000, 0.000000000000000000 ) ) ;
#48709 = CARTESIAN_POINT ( 'NONE',  ( -25.55153130240594450, -189.7472609257535510, 122.8793122007210741 ) ) ;
#48710 = ORIENTED_EDGE ( 'NONE', *, *, #12471, .F. ) ;
#48711 = DIRECTION ( 'NONE',  ( -1.000000000000000000, 0.000000000000000000, 0.000000000000000000 ) ) ;
#48712 = ORIENTED_EDGE ( 'NONE', *, *, #45472, .T. ) ;
#48713 = CARTESIAN_POINT ( 'NONE',  ( -332.3517673607765914, -70.03480886230919111, 25.08789112700620194 ) ) ;
#48714 = DIRECTION ( 'NONE',  ( 0.5085311186492216251, 0.000000000000000000, -0.8610436117673548884 ) ) ;
#48715 = DIRECTION ( 'NONE',  ( -0.5338233779647887367, 0.000000000000000000, -0.8455960035018273979 ) ) ;
#48716 = ORIENTED_EDGE ( 'NONE', *, *, #11333, .F. ) ;
#48717 = ORIENTED_EDGE ( 'NONE', *, *, #14336, .T. ) ;
#48718 = FACE_OUTER_BOUND ( 'NONE', #9082, .T. ) ;
#48719 = DIRECTION ( 'NONE',  ( -0.000000000000000000, 1.000000000000000000, -0.000000000000000000 ) ) ;
#48720 = ORIENTED_EDGE ( 'NONE', *, *, #41361, .T. ) ;
#48721 = DIRECTION ( 'NONE',  ( 1.000000000000000000, -0.000000000000000000, -0.000000000000000000 ) ) ;
#48722 = PLANE ( 'NONE',  #48046 ) ;
#48723 = VERTEX_POINT ( 'NONE', #48606 ) ;
#48724 = LINE ( 'NONE', #51626, #30919 ) ;
#48725 = DIRECTION ( 'NONE',  ( 0.000000000000000000, -0.9350162426854181641, -0.3546048870425267951 ) ) ;
#48726 = AXIS2_PLACEMENT_3D ( 'NONE', #30273, #25817, #14777 ) ;
#48727 = VECTOR ( 'NONE', #15078, 1000.000000000000000 ) ;
#48728 = ORIENTED_EDGE ( 'NONE', *, *, #16324, .F. ) ;
#48729 = CARTESIAN_POINT ( 'NONE',  ( -330.4913330509368166, -115.8919814278863356, 58.50955523165747252 ) ) ;
#48730 = ORIENTED_EDGE ( 'NONE', *, *, #51118, .T. ) ;
#48731 = CARTESIAN_POINT ( 'NONE',  ( -336.3521761649654422, -139.2044816956407089, -56.89493493766761389 ) ) ;
#48732 = CARTESIAN_POINT ( 'NONE',  ( 75.32224018181403835, -193.5000000000000000, 7.024906801079474405 ) ) ;
#48733 = EDGE_LOOP ( 'NONE', ( #34305, #39932, #27650, #14873 ) ) ;
#48734 = ADVANCED_FACE ( 'NONE', ( #13102 ), #40955, .F. ) ;
#48735 = CARTESIAN_POINT ( 'NONE',  ( 71.87891646118019651, -175.3837268820161057, -33.74820638215423685 ) ) ;
#48736 = ADVANCED_FACE ( 'NONE', ( #45436 ), #20732, .F. ) ;
#48737 = CARTESIAN_POINT ( 'NONE',  ( 60.00000000000001421, -63.50000000000000000, 0.000000000000000000 ) ) ;
#48738 = CARTESIAN_POINT ( 'NONE',  ( -49.21696003055057389, -193.5000000000000000, -0.6749830015182127774 ) ) ;
#48739 = EDGE_CURVE ( 'NONE', #8885, #34018, #49382, .T. ) ;
#48740 = DIRECTION ( 'NONE',  ( 0.000000000000000000, -1.000000000000000000, 0.000000000000000000 ) ) ;
#48741 = EDGE_CURVE ( 'NONE', #41226, #18084, #41468, .T. ) ;
#48742 = ORIENTED_EDGE ( 'NONE', *, *, #12429, .F. ) ;
#48743 = DIRECTION ( 'NONE',  ( 0.000000000000000000, -1.000000000000000000, 0.000000000000000000 ) ) ;
#48744 = ORIENTED_EDGE ( 'NONE', *, *, #2892, .T. ) ;
#48745 = EDGE_LOOP ( 'NONE', ( #10696, #25804, #37047, #48977 ) ) ;
#48746 = AXIS2_PLACEMENT_3D ( 'NONE', #4099, #16964, #32970 ) ;
#48747 = EDGE_CURVE ( 'NONE', #12568, #33588, #49118, .T. ) ;
#48748 = CARTESIAN_POINT ( 'NONE',  ( -49.42645310536303782, -189.7472609257535510, -0.3202698538628417357 ) ) ;
#48750 = ORIENTED_EDGE ( 'NONE', *, *, #22003, .T. ) ;
#48749 = FACE_OUTER_BOUND ( 'NONE', #23645, .T. ) ;
#48751 = EDGE_CURVE ( 'NONE', #38969, #42568, #17323, .T. ) ;
#48752 = ORIENTED_EDGE ( 'NONE', *, *, #41674, .T. ) ;
#48753 = FACE_OUTER_BOUND ( 'NONE', #34828, .T. ) ;
#48754 = EDGE_CURVE ( 'NONE', #28415, #8761, #37541, .T. ) ;
#48755 = EDGE_CURVE ( 'NONE', #467, #38948, #8385, .T. ) ;
#48756 = DIRECTION ( 'NONE',  ( -1.000000000000000000, -5.928974370888873265E-15, 8.589602288500856790E-15 ) ) ;
#48757 = VERTEX_POINT ( 'NONE', #1540 ) ;
#48758 = EDGE_CURVE ( 'NONE', #31354, #26252, #13368, .T. ) ;
#48759 = DIRECTION ( 'NONE',  ( 0.000000000000000000, 1.000000000000000000, -0.000000000000000000 ) ) ;
#48760 = VERTEX_POINT ( 'NONE', #8897 ) ;
#48761 = DIRECTION ( 'NONE',  ( 0.000000000000000000, 0.000000000000000000, 1.000000000000000000 ) ) ;
#48762 = CARTESIAN_POINT ( 'NONE',  ( -48.47912675150885065, -175.3837268820161057, 6.938893903907228378E-15 ) ) ;
#48763 = AXIS2_PLACEMENT_3D ( 'NONE', #51083, #23708, #19757 ) ;
#48764 = ADVANCED_FACE ( 'NONE', ( #8639 ), #24938, .T. ) ;
#48765 = DIRECTION ( 'NONE',  ( -0.000000000000000000, 1.000000000000000000, -0.000000000000000000 ) ) ;
#48766 = DIRECTION ( 'NONE',  ( 0.000000000000000000, 0.000000000000000000, 1.000000000000000000 ) ) ;
#48767 = VERTEX_POINT ( 'NONE', #40679 ) ;
#48768 = ORIENTED_EDGE ( 'NONE', *, *, #11459, .F. ) ;
#48770 = ORIENTED_EDGE ( 'NONE', *, *, #15136, .F. ) ;
#48769 = CIRCLE ( 'NONE', #33634, 125.0000000000000000 ) ;
#48771 = DIRECTION ( 'NONE',  ( -0.000000000000000000, 0.5680647467311540355, -0.8229838658936575735 ) ) ;
#48772 = CARTESIAN_POINT ( 'NONE',  ( 76.31829002442924548, -193.5000000000000000, 7.113702696402420145 ) ) ;
#48773 = LINE ( 'NONE', #12742, #48646 ) ;
#48774 = FACE_BOUND ( 'NONE', #10940, .T. ) ;
#48775 = DIRECTION ( 'NONE',  ( -0.1182731709213730997, 0.000000000000000000, 0.9929810960135161402 ) ) ;
#48776 = VERTEX_POINT ( 'NONE', #1011 ) ;
#48777 = EDGE_CURVE ( 'NONE', #35850, #10308, #4702, .T. ) ;
#48778 = EDGE_LOOP ( 'NONE', ( #17601, #9107, #5480, #32517 ) ) ;
#48780 = ORIENTED_EDGE ( 'NONE', *, *, #26463, .T. ) ;
#48779 = FACE_OUTER_BOUND ( 'NONE', #10201, .T. ) ;
#48781 = VERTEX_POINT ( 'NONE', #16808 ) ;
#48782 = AXIS2_PLACEMENT_3D ( 'NONE', #37112, #28956, #17687 ) ;
#48783 = DIRECTION ( 'NONE',  ( 0.6528221181905174975, 0.000000000000000000, 0.7575112421616236880 ) ) ;
#48784 = PLANE ( 'NONE',  #34204 ) ;
#48785 = CARTESIAN_POINT ( 'NONE',  ( 66.03142248012325410, -193.5000000000000000, 50.12318939044039467 ) ) ;
#48786 = FACE_OUTER_BOUND ( 'NONE', #8230, .T. ) ;
#48787 = VERTEX_POINT ( 'NONE', #4977 ) ;
#48788 = CARTESIAN_POINT ( 'NONE',  ( 73.62243227112293198, -177.1207230881787780, 21.61797988633237821 ) ) ;
#48789 = ORIENTED_EDGE ( 'NONE', *, *, #10213, .F. ) ;
#48790 = ADVANCED_FACE ( 'NONE', ( #44910 ), #481, .T. ) ;
#48791 = EDGE_LOOP ( 'NONE', ( #15621, #17973, #5538, #7094 ) ) ;
#48792 = DIRECTION ( 'NONE',  ( -0.000000000000000000, 0.2393156642875547968, -0.9709418174260527890 ) ) ;
#48793 = CARTESIAN_POINT ( 'NONE',  ( 32.49319223169170812, -175.3837268820161057, -95.22858582633060109 ) ) ;
#48794 = DIRECTION ( 'NONE',  ( 0.000000000000000000, -1.000000000000000000, 0.000000000000000000 ) ) ;
#48795 = FACE_OUTER_BOUND ( 'NONE', #1778, .T. ) ;
#48796 = AXIS2_PLACEMENT_3D ( 'NONE', #33017, #37740, #29334 ) ;
#48797 = EDGE_CURVE ( 'NONE', #44067, #30050, #28950, .T. ) ;
#48798 = ADVANCED_FACE ( 'NONE', ( #20462 ), #25200, .F. ) ;
#48799 = CARTESIAN_POINT ( 'NONE',  ( -171.1451123608488274, -189.7472609257535510, 18.13990644964088261 ) ) ;
#48800 = EDGE_CURVE ( 'NONE', #38881, #49882, #13888, .T. ) ;
#48801 = FACE_OUTER_BOUND ( 'NONE', #44634, .T. ) ;
#48802 = CARTESIAN_POINT ( 'NONE',  ( 75.48400724637754422, -183.6283474603465606, -16.06677968424457248 ) ) ;
#48803 = EDGE_CURVE ( 'NONE', #840, #20061, #9951, .T. ) ;
#48804 = ORIENTED_EDGE ( 'NONE', *, *, #43198, .T. ) ;
#48805 = DIRECTION ( 'NONE',  ( 0.000000000000000000, 0.000000000000000000, -1.000000000000000000 ) ) ;
#48806 = DIRECTION ( 'NONE',  ( 0.000000000000000000, 0.000000000000000000, -1.000000000000000000 ) ) ;
#48807 = EDGE_CURVE ( 'NONE', #1947, #36354, #38043, .T. ) ;
#48808 = VECTOR ( 'NONE', #31211, 999.9999999999998863 ) ;
#48809 = LINE ( 'NONE', #1740, #21964 ) ;
#48810 = FACE_BOUND ( 'NONE', #33615, .T. ) ;
#48811 = VERTEX_POINT ( 'NONE', #29904 ) ;
#48812 = EDGE_CURVE ( 'NONE', #40042, #11813, #46216, .T. ) ;
#48813 = CARTESIAN_POINT ( 'NONE',  ( -58.29063029684667185, -193.5000000000000000, 124.6143426664034877 ) ) ;
#48814 = ORIENTED_EDGE ( 'NONE', *, *, #27494, .T. ) ;
#48815 = LINE ( 'NONE', #12539, #32841 ) ;
#48816 = ORIENTED_EDGE ( 'NONE', *, *, #45851, .T. ) ;
#48817 = DIRECTION ( 'NONE',  ( -0.000000000000000000, -0.4647231720437604574, 0.8854560256532141294 ) ) ;
#48818 = ADVANCED_FACE ( 'NONE', ( #6780 ), #10193, .F. ) ;
#48819 = ORIENTED_EDGE ( 'NONE', *, *, #24333, .T. ) ;
#48820 = CIRCLE ( 'NONE', #23621, 125.0000000000000000 ) ;
#48821 = EDGE_CURVE ( 'NONE', #38934, #23682, #25966, .T. ) ;
#48822 = DIRECTION ( 'NONE',  ( -1.000000000000000000, 0.000000000000000000, 0.000000000000000000 ) ) ;
#48823 = AXIS2_PLACEMENT_3D ( 'NONE', #13991, #1377, #41054 ) ;
#48824 = EDGE_CURVE ( 'NONE', #27774, #39327, #42240, .T. ) ;
#48825 = DIRECTION ( 'NONE',  ( -1.000000000000000000, -0.000000000000000000, 0.000000000000000000 ) ) ;
#48827 = ORIENTED_EDGE ( 'NONE', *, *, #35402, .T. ) ;
#48826 = LINE ( 'NONE', #49344, #9498 ) ;
#48828 = EDGE_CURVE ( 'NONE', #6831, #21096, #17830, .T. ) ;
#48829 = DIRECTION ( 'NONE',  ( 1.000000000000000000, -0.000000000000000000, -0.000000000000000000 ) ) ;
#48830 = ORIENTED_EDGE ( 'NONE', *, *, #20210, .F. ) ;
#48831 = EDGE_CURVE ( 'NONE', #45569, #33712, #33850, .T. ) ;
#48832 = VERTEX_POINT ( 'NONE', #45963 ) ;
#48833 = DIRECTION ( 'NONE',  ( 0.000000000000000000, 1.000000000000000000, 0.000000000000000000 ) ) ;
#48834 = LINE ( 'NONE', #8868, #7534 ) ;
#48835 = VERTEX_POINT ( 'NONE', #41742 ) ;
#48836 = CARTESIAN_POINT ( 'NONE',  ( 71.35177504360963496, -189.7472609257535510, 31.88354567335082024 ) ) ;
#48837 = CARTESIAN_POINT ( 'NONE',  ( -339.1964088526558498, -102.1108035431478811, -54.98865587491830809 ) ) ;
#48838 = AXIS2_PLACEMENT_3D ( 'NONE', #3713, #31574, #20521 ) ;
#48839 = VECTOR ( 'NONE', #47703, 1000.000000000000000 ) ;
#48840 = AXIS2_PLACEMENT_3D ( 'NONE', #9257, #1631, #25278 ) ;
#48841 = EDGE_CURVE ( 'NONE', #41328, #19801, #2323, .T. ) ;
#48842 = DIRECTION ( 'NONE',  ( 0.000000000000000000, -0.8229838658936494689, 0.5680647467311658039 ) ) ;
#48843 = CARTESIAN_POINT ( 'NONE',  ( -48.47912675150885065, -189.7472609257535510, 6.938893903907228378E-15 ) ) ;
#48844 = ORIENTED_EDGE ( 'NONE', *, *, #11455, .T. ) ;
#48847 = EDGE_LOOP ( 'NONE', ( #5813, #13501, #17849, #40546 ) ) ;
#48846 = DIRECTION ( 'NONE',  ( 0.000000000000000000, 0.000000000000000000, 1.000000000000000000 ) ) ;
#48845 = DIRECTION ( 'NONE',  ( 0.000000000000000000, -1.000000000000000000, 0.000000000000000000 ) ) ;
#48848 = ORIENTED_EDGE ( 'NONE', *, *, #44811, .F. ) ;
#48849 = CARTESIAN_POINT ( 'NONE',  ( 65.52619748798556998, -193.5000000000000000, 48.77484799213969069 ) ) ;
#48850 = ORIENTED_EDGE ( 'NONE', *, *, #11459, .T. ) ;
#48851 = PLANE ( 'NONE',  #12143 ) ;
#48852 = ORIENTED_EDGE ( 'NONE', *, *, #20484, .T. ) ;
#48853 = CARTESIAN_POINT ( 'NONE',  ( -49.30901192927172616, -175.3837268820161057, -124.9972451320097093 ) ) ;
#48854 = LINE ( 'NONE', #29118, #34286 ) ;
#48855 = ORIENTED_EDGE ( 'NONE', *, *, #8938, .T. ) ;
#48857 = CARTESIAN_POINT ( 'NONE',  ( -330.4913330509368166, -123.5000000000000284, 0.000000000000000000 ) ) ;
#48856 = DIRECTION ( 'NONE',  ( 0.000000000000000000, 0.000000000000000000, -1.000000000000000000 ) ) ;
#48858 = ORIENTED_EDGE ( 'NONE', *, *, #23043, .F. ) ;
#48859 = AXIS2_PLACEMENT_3D ( 'NONE', #23717, #39724, #19767 ) ;
#48860 = VERTEX_POINT ( 'NONE', #18355 ) ;
#48861 = FACE_OUTER_BOUND ( 'NONE', #25962, .T. ) ;
#48862 = CIRCLE ( 'NONE', #48021, 10.00000000000000711 ) ;
#48864 = VECTOR ( 'NONE', #6507, 1000.000000000000000 ) ;
#48863 = CARTESIAN_POINT ( 'NONE',  ( -238.7407812814481076, -213.5000000000000000, 10.00000000000000178 ) ) ;
#48865 = CARTESIAN_POINT ( 'NONE',  ( -137.2624501260119700, -177.1207230881787780, 87.99159897727969337 ) ) ;
#48866 = FACE_OUTER_BOUND ( 'NONE', #31406, .T. ) ;
#48867 = VERTEX_POINT ( 'NONE', #18850 ) ;
#48868 = DIRECTION ( 'NONE',  ( 0.000000000000000000, -1.000000000000000000, 0.000000000000000000 ) ) ;
#48869 = EDGE_CURVE ( 'NONE', #2101, #10970, #31471, .T. ) ;
#48870 = EDGE_CURVE ( 'NONE', #13263, #11286, #39006, .T. ) ;
#48871 = PLANE ( 'NONE',  #38773 ) ;
#48872 = CARTESIAN_POINT ( 'NONE',  ( -111.8989814360438686, -189.7472609257535510, -107.7168604805787169 ) ) ;
#48873 = DIRECTION ( 'NONE',  ( 0.000000000000000000, -1.000000000000000000, 0.000000000000000000 ) ) ;
#48874 = DIRECTION ( 'NONE',  ( 1.000000000000000000, -0.000000000000000000, -0.000000000000000000 ) ) ;
#48875 = ORIENTED_EDGE ( 'NONE', *, *, #43217, .F. ) ;
#48876 = ORIENTED_EDGE ( 'NONE', *, *, #15111, .T. ) ;
#48877 = DIRECTION ( 'NONE',  ( 0.8455960035018272869, 0.000000000000000000, -0.5338233779647886257 ) ) ;
#48878 = AXIS2_PLACEMENT_3D ( 'NONE', #27818, #8123, #19427 ) ;
#48879 = DIRECTION ( 'NONE',  ( 0.000000000000000000, 0.000000000000000000, -1.000000000000000000 ) ) ;
#48880 = FACE_OUTER_BOUND ( 'NONE', #12723, .T. ) ;
#48881 = ORIENTED_EDGE ( 'NONE', *, *, #23597, .F. ) ;
#48882 = VERTEX_POINT ( 'NONE', #10715 ) ;
#48883 = ORIENTED_EDGE ( 'NONE', *, *, #9475, .T. ) ;
#48884 = AXIS2_PLACEMENT_3D ( 'NONE', #47847, #35225, #15524 ) ;
#48885 = DIRECTION ( 'NONE',  ( 0.000000000000000000, 0.000000000000000000, 1.000000000000000000 ) ) ;
#48886 = FACE_OUTER_BOUND ( 'NONE', #1115, .T. ) ;
#48887 = EDGE_CURVE ( 'NONE', #11654, #46759, #50664, .T. ) ;
#48888 = DIRECTION ( 'NONE',  ( 0.000000000000000000, -1.000000000000000000, 0.000000000000000000 ) ) ;
#48889 = CARTESIAN_POINT ( 'NONE',  ( -48.47912675150885065, -177.1207230881787780, 6.938893903907228378E-15 ) ) ;
#48890 = ORIENTED_EDGE ( 'NONE', *, *, #17690, .F. ) ;
#48891 = DIRECTION ( 'NONE',  ( 1.000000000000000000, -0.000000000000000000, -0.000000000000000000 ) ) ;
#48892 = FACE_OUTER_BOUND ( 'NONE', #28597, .T. ) ;
#48893 = AXIS2_PLACEMENT_3D ( 'NONE', #32055, #47849, #3679 ) ;
#48894 = CIRCLE ( 'NONE', #28712, 60.00000000000000000 ) ;
#48895 = EDGE_CURVE ( 'NONE', #30411, #31046, #38570, .T. ) ;
#48896 = DIRECTION ( 'NONE',  ( 0.000000000000000000, 0.6631226582407989678, 0.7485107481710977506 ) ) ;
#48897 = ORIENTED_EDGE ( 'NONE', *, *, #51976, .F. ) ;
#48898 = CIRCLE ( 'NONE', #30416, 125.0000000000000000 ) ;
#48899 = AXIS2_PLACEMENT_3D ( 'NONE', #23031, #3060, #39564 ) ;
#48900 = ORIENTED_EDGE ( 'NONE', *, *, #36200, .T. ) ;
#48901 = CARTESIAN_POINT ( 'NONE',  ( -48.47912675150885065, -177.1207230881787780, 6.938893903907228378E-15 ) ) ;
#48902 = CARTESIAN_POINT ( 'NONE',  ( -60.00000000000000000, -63.50000000000000000, -60.00000000000000711 ) ) ;
#48903 = DIRECTION ( 'NONE',  ( 0.000000000000000000, 0.000000000000000000, 1.000000000000000000 ) ) ;
#48906 = ORIENTED_EDGE ( 'NONE', *, *, #19549, .F. ) ;
#48905 = CARTESIAN_POINT ( 'NONE',  ( -80.85382946868861609, -193.5000000000000000, 119.6996507684852986 ) ) ;
#48904 = FACE_OUTER_BOUND ( 'NONE', #19514, .T. ) ;
#48907 = DIRECTION ( 'NONE',  ( 0.8610436117673585521, 0.000000000000000000, -0.5085311186492154079 ) ) ;
#48908 = EDGE_LOOP ( 'NONE', ( #5631, #39556, #23476, #44793 ) ) ;
#48909 = DIRECTION ( 'NONE',  ( 0.000000000000000000, 0.000000000000000000, -1.000000000000000000 ) ) ;
#48910 = VECTOR ( 'NONE', #52034, 1000.000000000000000 ) ;
#48911 = CARTESIAN_POINT ( 'NONE',  ( -48.47912675150885065, -177.1207230881787780, 6.938893903907228378E-15 ) ) ;
#48912 = EDGE_LOOP ( 'NONE', ( #781, #29145, #51688, #28762 ) ) ;
#48913 = CARTESIAN_POINT ( 'NONE',  ( -332.3517673607765914, -177.7325358280884586, 23.38292116578760726 ) ) ;
#48915 = DIRECTION ( 'NONE',  ( -0.6068001458185834363, 0.000000000000000000, -0.7948544414133608127 ) ) ;
#48914 = DIRECTION ( 'NONE',  ( -0.000000000000000000, 1.000000000000000000, -0.000000000000000000 ) ) ;
#48916 = ORIENTED_EDGE ( 'NONE', *, *, #49984, .F. ) ;
#48917 = VECTOR ( 'NONE', #24969, 1000.000000000000000 ) ;
#48918 = FACE_OUTER_BOUND ( 'NONE', #5864, .T. ) ;
#48919 = FACE_OUTER_BOUND ( 'NONE', #31817, .T. ) ;
#48920 = DIRECTION ( 'NONE',  ( 1.000000000000000000, 0.000000000000000000, 0.000000000000000000 ) ) ;
#48921 = ORIENTED_EDGE ( 'NONE', *, *, #5334, .T. ) ;
#48922 = DIRECTION ( 'NONE',  ( 0.000000000000000000, 0.000000000000000000, -1.000000000000000000 ) ) ;
#48923 = FACE_OUTER_BOUND ( 'NONE', #28046, .T. ) ;
#48924 = EDGE_LOOP ( 'NONE', ( #5772, #24568, #38164, #45622 ) ) ;
#48925 = ADVANCED_FACE ( 'NONE', ( #34371 ), #50930, .T. ) ;
#48926 = VECTOR ( 'NONE', #11760, 1000.000000000000000 ) ;
#48927 = DIRECTION ( 'NONE',  ( 0.000000000000000000, -0.000000000000000000, -1.000000000000000000 ) ) ;
#48928 = DIRECTION ( 'NONE',  ( 0.000000000000000000, -0.8229838658936516893, 0.5680647467311625842 ) ) ;
#48929 = VERTEX_POINT ( 'NONE', #2570 ) ;
#48930 = VECTOR ( 'NONE', #25216, 1000.000000000000227 ) ;
#48931 = CIRCLE ( 'NONE', #29595, 125.0000000000000000 ) ;
#48932 = DIRECTION ( 'NONE',  ( -1.000000000000000000, -0.000000000000000000, -0.000000000000000000 ) ) ;
#48933 = CARTESIAN_POINT ( 'NONE',  ( -108.4791267515088435, -132.5479369270331915, -60.00000000000002842 ) ) ;
#48934 = DIRECTION ( 'NONE',  ( -1.000000000000000000, -0.000000000000000000, -0.000000000000000000 ) ) ;
#48935 = CARTESIAN_POINT ( 'NONE',  ( -117.0614752283615161, -175.3837268820161057, 103.3076327631967786 ) ) ;
#48936 = DIRECTION ( 'NONE',  ( -0.000000000000000000, 0.9927088740980553050, 0.1205366802553130001 ) ) ;
#48937 = VECTOR ( 'NONE', #47268, 1000.000000000000000 ) ;
#48938 = PLANE ( 'NONE',  #28791 ) ;
#48939 = CARTESIAN_POINT ( 'NONE',  ( 68.24201764719070695, -183.6283474603465606, -44.73448837594910543 ) ) ;
#48940 = EDGE_CURVE ( 'NONE', #7798, #28664, #14659, .T. ) ;
#48941 = DIRECTION ( 'NONE',  ( 0.000000000000000000, 0.000000000000000000, 1.000000000000000000 ) ) ;
#48943 = ORIENTED_EDGE ( 'NONE', *, *, #12653, .T. ) ;
#48942 = LINE ( 'NONE', #44212, #22839 ) ;
#48944 = VECTOR ( 'NONE', #12252, 999.9999999999998863 ) ;
#48945 = ORIENTED_EDGE ( 'NONE', *, *, #15823, .F. ) ;
#48946 = CARTESIAN_POINT ( 'NONE',  ( -305.0000000000000568, -101.7569374291128383, -55.92172413327835301 ) ) ;
#48947 = AXIS2_PLACEMENT_3D ( 'NONE', #22701, #50826, #38714 ) ;
#48948 = LINE ( 'NONE', #46055, #20422 ) ;
#48949 = ORIENTED_EDGE ( 'NONE', *, *, #14304, .T. ) ;
#48950 = VERTEX_POINT ( 'NONE', #22802 ) ;
#48951 = ORIENTED_EDGE ( 'NONE', *, *, #20558, .F. ) ;
#48952 = DIRECTION ( 'NONE',  ( 0.000000000000000000, 0.000000000000000000, -1.000000000000000000 ) ) ;
#48953 = PLANE ( 'NONE',  #31172 ) ;
#48954 = CARTESIAN_POINT ( 'NONE',  ( -330.4913330509368166, -123.5000000000000284, 0.000000000000000000 ) ) ;
#48956 = ORIENTED_EDGE ( 'NONE', *, *, #5565, .F. ) ;
#48955 = AXIS2_PLACEMENT_3D ( 'NONE', #17405, #33428, #51782 ) ;
#48957 = VECTOR ( 'NONE', #10410, 1000.000000000000114 ) ;
#48958 = EDGE_LOOP ( 'NONE', ( #50567, #33843, #30657, #32920 ) ) ;
#48959 = DIRECTION ( 'NONE',  ( 0.000000000000000000, -0.000000000000000000, 1.000000000000000000 ) ) ;
#48961 = VERTEX_POINT ( 'NONE', #45693 ) ;
#48960 = CYLINDRICAL_SURFACE ( 'NONE', #46772, 125.0000000000000000 ) ;
#48962 = VECTOR ( 'NONE', #12129, 1000.000000000000000 ) ;
#48963 = DIRECTION ( 'NONE',  ( 0.000000000000000000, 1.000000000000000000, 0.000000000000000000 ) ) ;
#48964 = ORIENTED_EDGE ( 'NONE', *, *, #12058, .T. ) ;
#48965 = DIRECTION ( 'NONE',  ( 1.043714542225393539E-14, 0.4647231720437755564, 0.8854560256532062468 ) ) ;
#48966 = VERTEX_POINT ( 'NONE', #9682 ) ;
#48967 = EDGE_CURVE ( 'NONE', #30801, #3547, #25708, .T. ) ;
#48968 = AXIS2_PLACEMENT_3D ( 'NONE', #49592, #5190, #41427 ) ;
#48969 = LINE ( 'NONE', #36878, #39992 ) ;
#48970 = DIRECTION ( 'NONE',  ( 0.000000000000000000, 1.000000000000000000, -0.000000000000000000 ) ) ;
#48971 = DIRECTION ( 'NONE',  ( 0.000000000000000000, 0.000000000000000000, 1.000000000000000000 ) ) ;
#48972 = ADVANCED_FACE ( 'NONE', ( #19125 ), #36897, .T. ) ;
#48973 = ORIENTED_EDGE ( 'NONE', *, *, #31065, .F. ) ;
#48974 = ORIENTED_EDGE ( 'NONE', *, *, #45603, .T. ) ;
#48975 = DIRECTION ( 'NONE',  ( 0.000000000000000000, 0.000000000000000000, -1.000000000000000000 ) ) ;
#48976 = CARTESIAN_POINT ( 'NONE',  ( -330.4913330509368166, -168.7406467949202806, 39.41172259083927543 ) ) ;
#48977 = ORIENTED_EDGE ( 'NONE', *, *, #23994, .T. ) ;
#48978 = PLANE ( 'NONE',  #50082 ) ;
#48979 = VECTOR ( 'NONE', #20334, 1000.000000000000000 ) ;
#48980 = DIRECTION ( 'NONE',  ( -1.000000000000000000, 0.000000000000000000, 0.000000000000000000 ) ) ;
#48981 = VERTEX_POINT ( 'NONE', #27516 ) ;
#48982 = EDGE_CURVE ( 'NONE', #16149, #23737, #51196, .T. ) ;
#48983 = DIRECTION ( 'NONE',  ( 0.000000000000000000, -0.000000000000000000, 1.000000000000000000 ) ) ;
#48984 = ADVANCED_FACE ( 'NONE', ( #26992 ), #48479, .F. ) ;
#48986 = VECTOR ( 'NONE', #29389, 1000.000000000000000 ) ;
#48985 = LINE ( 'NONE', #21116, #12268 ) ;
#48987 = ORIENTED_EDGE ( 'NONE', *, *, #10213, .T. ) ;
#48988 = DIRECTION ( 'NONE',  ( 0.000000000000000000, 0.000000000000000000, -1.000000000000000000 ) ) ;
#48989 = ORIENTED_EDGE ( 'NONE', *, *, #46097, .T. ) ;
#48990 = FACE_BOUND ( 'NONE', #18780, .T. ) ;
#48991 = ADVANCED_FACE ( 'NONE', ( #39073 ), #7549, .T. ) ;
#48992 = DIRECTION ( 'NONE',  ( -0.9960498426152171181, 0.000000000000000000, 0.08879589532293157006 ) ) ;
#48993 = ORIENTED_EDGE ( 'NONE', *, *, #50243, .F. ) ;
#48994 = LINE ( 'NONE', #33211, #28176 ) ;
#48995 = LINE ( 'NONE', #45065, #23862 ) ;
#48996 = FACE_OUTER_BOUND ( 'NONE', #40779, .T. ) ;
#48997 = VECTOR ( 'NONE', #20856, 1000.000000000000000 ) ;
#48998 = DIRECTION ( 'NONE',  ( -1.000000000000000000, 0.000000000000000000, 0.000000000000000000 ) ) ;
#48999 = ORIENTED_EDGE ( 'NONE', *, *, #49031, .T. ) ;
#49000 = LINE ( 'NONE', #17476, #7707 ) ;
#49001 = ORIENTED_EDGE ( 'NONE', *, *, #20518, .T. ) ;
#49002 = ORIENTED_EDGE ( 'NONE', *, *, #37863, .F. ) ;
#49003 = VECTOR ( 'NONE', #23563, 1000.000000000000000 ) ;
#49004 = EDGE_CURVE ( 'NONE', #14774, #25561, #7294, .T. ) ;
#49005 = DIRECTION ( 'NONE',  ( -0.000000000000000000, -0.000000000000000000, -1.000000000000000000 ) ) ;
#49007 = ORIENTED_EDGE ( 'NONE', *, *, #6757, .F. ) ;
#49006 = CARTESIAN_POINT ( 'NONE',  ( -332.3517673607765914, -98.41210887299327226, -53.46519113769058151 ) ) ;
#49008 = ORIENTED_EDGE ( 'NONE', *, *, #48430, .F. ) ;
#49009 = PLANE ( 'NONE',  #33261 ) ;
#49010 = CARTESIAN_POINT ( 'NONE',  ( -173.4787860028527007, -193.5000000000000000, 0.2918682030023981300 ) ) ;
#49011 = LINE ( 'NONE', #42082, #13444 ) ;
#49012 = VERTEX_POINT ( 'NONE', #7033 ) ;
#49013 = CARTESIAN_POINT ( 'NONE',  ( -340.0000000000000568, -168.5000000000000284, 0.000000000000000000 ) ) ;
#49014 = VERTEX_POINT ( 'NONE', #47249 ) ;
#49015 = DIRECTION ( 'NONE',  ( 0.000000000000000000, -1.000000000000000000, 0.000000000000000000 ) ) ;
#49016 = CARTESIAN_POINT ( 'NONE',  ( 54.54686566053560881, -193.5000000000000000, 69.00559874123594284 ) ) ;
#49017 = AXIS2_PLACEMENT_3D ( 'NONE', #37797, #17839, #9692 ) ;
#49018 = CARTESIAN_POINT ( 'NONE',  ( -160.9694636715425702, -189.7472609257535510, 54.50618404931040573 ) ) ;
#49019 = CARTESIAN_POINT ( 'NONE',  ( -47.60339180931321579, -193.5000000000000000, -0.4827922027307358088 ) ) ;
#49020 = ORIENTED_EDGE ( 'NONE', *, *, #822, .T. ) ;
#49021 = ORIENTED_EDGE ( 'NONE', *, *, #46036, .F. ) ;
#49022 = VECTOR ( 'NONE', #23336, 999.9999999999998863 ) ;
#49023 = VERTEX_POINT ( 'NONE', #43286 ) ;
#49024 = FACE_OUTER_BOUND ( 'NONE', #2731, .T. ) ;
#49025 = DIRECTION ( 'NONE',  ( -0.9890401873221644768, 0.000000000000000000, 0.1476465640024779702 ) ) ;
#49026 = DIRECTION ( 'NONE',  ( 1.000000000000000000, 0.000000000000000000, 5.782411586589357392E-17 ) ) ;
#49027 = FACE_BOUND ( 'NONE', #27360, .T. ) ;
#49028 = DIRECTION ( 'NONE',  ( 0.000000000000000000, -1.000000000000000000, 0.000000000000000000 ) ) ;
#49029 = VERTEX_POINT ( 'NONE', #30943 ) ;
#49030 = EDGE_CURVE ( 'NONE', #35703, #45018, #44046, .T. ) ;
#49031 = EDGE_CURVE ( 'NONE', #50633, #3034, #14934, .T. ) ;
#49032 = VECTOR ( 'NONE', #21230, 1000.000000000000000 ) ;
#49033 = EDGE_LOOP ( 'NONE', ( #17813, #37396, #16197, #14247 ) ) ;
#49035 = VERTEX_POINT ( 'NONE', #20872 ) ;
#49034 = CARTESIAN_POINT ( 'NONE',  ( 69.66827051661184100, -175.3837268820161057, -40.81902153125260213 ) ) ;
#49036 = DIRECTION ( 'NONE',  ( 0.000000000000000000, -0.000000000000000000, -1.000000000000000000 ) ) ;
#49037 = ORIENTED_EDGE ( 'NONE', *, *, #42316, .T. ) ;
#49038 = DIRECTION ( 'NONE',  ( 0.000000000000000000, 0.000000000000000000, 1.000000000000000000 ) ) ;
#49039 = PLANE ( 'NONE',  #49333 ) ;
#49040 = CARTESIAN_POINT ( 'NONE',  ( -336.3521761649653854, -129.1091364105427033, 59.73723787327234191 ) ) ;
#49041 = CARTESIAN_POINT ( 'NONE',  ( -330.4913330509368166, -123.5000000000000284, 0.000000000000000000 ) ) ;
#49042 = LINE ( 'NONE', #20393, #45262 ) ;
#49043 = EDGE_CURVE ( 'NONE', #18767, #24959, #19376, .T. ) ;
#49044 = CARTESIAN_POINT ( 'NONE',  ( -332.3517673607765914, -63.67752800890095699, 4.612141029301498385 ) ) ;
#49045 = VERTEX_POINT ( 'NONE', #46987 ) ;
#49046 = EDGE_CURVE ( 'NONE', #38839, #5823, #16368, .T. ) ;
#49047 = ORIENTED_EDGE ( 'NONE', *, *, #36515, .F. ) ;
#49048 = FACE_OUTER_BOUND ( 'NONE', #16603, .T. ) ;
#49049 = ADVANCED_FACE ( 'NONE', ( #23060 ), #35391, .T. ) ;
#49050 = DIRECTION ( 'NONE',  ( 0.000000000000000000, -1.000000000000000000, 0.000000000000000000 ) ) ;
#49051 = AXIS2_PLACEMENT_3D ( 'NONE', #1658, #45803, #40800 ) ;
#49052 = EDGE_CURVE ( 'NONE', #37318, #15638, #15445, .T. ) ;
#49053 = VECTOR ( 'NONE', #45965, 1000.000000000000000 ) ;
#49054 = LINE ( 'NONE', #1205, #23951 ) ;
#49055 = CARTESIAN_POINT ( 'NONE',  ( 21.49274850782855495, -175.3837268820161057, -103.5805805771126558 ) ) ;
#49056 = FACE_OUTER_BOUND ( 'NONE', #5169, .T. ) ;
#49057 = VERTEX_POINT ( 'NONE', #31451 ) ;
#49058 = CARTESIAN_POINT ( 'NONE',  ( -68.21229068036657850, -193.5000000000000000, -123.4325817657429809 ) ) ;
#49059 = PLANE ( 'NONE',  #26519 ) ;
#49060 = CARTESIAN_POINT ( 'NONE',  ( -48.47912675150885065, -175.3837268820161057, 6.938893903907228378E-15 ) ) ;
#49061 = FACE_BOUND ( 'NONE', #49575, .T. ) ;
#49062 = EDGE_LOOP ( 'NONE', ( #30357, #26436, #20650, #4428 ) ) ;
#49063 = DIRECTION ( 'NONE',  ( 1.000000000000000000, -0.000000000000000000, -0.000000000000000000 ) ) ;
#49064 = EDGE_LOOP ( 'NONE', ( #43934, #6600, #1562, #34764 ) ) ;
#49065 = FACE_OUTER_BOUND ( 'NONE', #12036, .T. ) ;
#49066 = ORIENTED_EDGE ( 'NONE', *, *, #37874, .T. ) ;
#49067 = DIRECTION ( 'NONE',  ( 0.9646355819083576311, 0.000000000000000000, 0.2635871660690715101 ) ) ;
#49068 = AXIS2_PLACEMENT_3D ( 'NONE', #39565, #51683, #24084 ) ;
#49069 = ORIENTED_EDGE ( 'NONE', *, *, #37166, .F. ) ;
#49070 = CARTESIAN_POINT ( 'NONE',  ( -151.1459075827612537, -183.6283474603465606, 69.53890913632950799 ) ) ;
#49071 = DIRECTION ( 'NONE',  ( 0.000000000000000000, -3.393119119010634677E-13, 1.000000000000000000 ) ) ;
#49073 = ORIENTED_EDGE ( 'NONE', *, *, #47195, .T. ) ;
#49072 = DIRECTION ( 'NONE',  ( -0.000000000000000000, 0.9709418174260519008, -0.2393156642875582940 ) ) ;
#49074 = PLANE ( 'NONE',  #26889 ) ;
#49075 = EDGE_LOOP ( 'NONE', ( #3014, #41113, #40073, #42133 ) ) ;
#49076 = ORIENTED_EDGE ( 'NONE', *, *, #15735, .F. ) ;
#49077 = VERTEX_POINT ( 'NONE', #16682 ) ;
#49078 = EDGE_CURVE ( 'NONE', #40382, #12661, #47499, .T. ) ;
#49079 = DIRECTION ( 'NONE',  ( -1.000000000000000000, 0.000000000000000000, -0.000000000000000000 ) ) ;
#49080 = CARTESIAN_POINT ( 'NONE',  ( -107.6930423737362190, -193.5000000000000000, 110.0850225811110761 ) ) ;
#49081 = VECTOR ( 'NONE', #38303, 1000.000000000000000 ) ;
#49082 = EDGE_LOOP ( 'NONE', ( #43982, #40992, #26699, #9605 ) ) ;
#49083 = CARTESIAN_POINT ( 'NONE',  ( -48.47912675150883643, -193.5000000000000000, -125.0000000000000000 ) ) ;
#49084 = AXIS2_PLACEMENT_3D ( 'NONE', #50464, #46514, #26787 ) ;
#49085 = LINE ( 'NONE', #39431, #46311 ) ;
#49086 = CARTESIAN_POINT ( 'NONE',  ( 34.93559171950835918, -177.1207230881787780, -93.09664195018496002 ) ) ;
#49087 = EDGE_LOOP ( 'NONE', ( #29399, #42869, #31498, #17785 ) ) ;
#49088 = VECTOR ( 'NONE', #19766, 1000.000000000000000 ) ;
#49089 = ADVANCED_FACE ( 'NONE', ( #19629 ), #35653, .T. ) ;
#49090 = EDGE_CURVE ( 'NONE', #22824, #23304, #20595, .T. ) ;
#49091 = EDGE_CURVE ( 'NONE', #39789, #36788, #12700, .T. ) ;
#49092 = VECTOR ( 'NONE', #50035, 1000.000000000000000 ) ;
#49093 = EDGE_CURVE ( 'NONE', #25190, #50966, #7136, .T. ) ;
#49094 = DIRECTION ( 'NONE',  ( 0.000000000000000000, -0.8854560256532141294, -0.4647231720437604574 ) ) ;
#49095 = DIRECTION ( 'NONE',  ( 0.000000000000000000, 1.000000000000000000, 0.000000000000000000 ) ) ;
#49096 = VERTEX_POINT ( 'NONE', #13496 ) ;
#49099 = ORIENTED_EDGE ( 'NONE', *, *, #46587, .T. ) ;
#49098 = DIRECTION ( 'NONE',  ( 0.000000000000000000, -5.851800525628429686E-14, -1.000000000000000000 ) ) ;
#49097 = DIRECTION ( 'NONE',  ( 0.000000000000000000, 0.8854560256532062468, -0.4647231720437755564 ) ) ;
#49100 = EDGE_LOOP ( 'NONE', ( #5153, #42531, #21014, #32540 ) ) ;
#49101 = EDGE_CURVE ( 'NONE', #25971, #33577, #50024, .T. ) ;
#49102 = VECTOR ( 'NONE', #13413, 1000.000000000000000 ) ;
#49103 = CARTESIAN_POINT ( 'NONE',  ( -27.18512803868276251, -193.5000000000000000, -123.1729094355498404 ) ) ;
#49104 = ORIENTED_EDGE ( 'NONE', *, *, #15989, .T. ) ;
#49105 = DIRECTION ( 'NONE',  ( -0.000000000000000000, -0.9927088740980548609, -0.1205366802553164696 ) ) ;
#49106 = VECTOR ( 'NONE', #49279, 1000.000000000000000 ) ;
#49107 = ORIENTED_EDGE ( 'NONE', *, *, #45270, .F. ) ;
#49108 = CARTESIAN_POINT ( 'NONE',  ( -169.6719064342497632, -193.5000000000000000, 30.61552143554992256 ) ) ;
#49109 = FACE_OUTER_BOUND ( 'NONE', #22897, .T. ) ;
#49110 = ORIENTED_EDGE ( 'NONE', *, *, #43935, .T. ) ;
#49111 = EDGE_CURVE ( 'NONE', #46692, #51208, #6142, .T. ) ;
#49112 = DIRECTION ( 'NONE',  ( 0.000000000000000000, -0.000000000000000000, 1.000000000000000000 ) ) ;
#49113 = AXIS2_PLACEMENT_3D ( 'NONE', #51123, #31888, #51364 ) ;
#49114 = VERTEX_POINT ( 'NONE', #5104 ) ;
#49115 = ADVANCED_FACE ( 'NONE', ( #46093 ), #17461, .F. ) ;
#49116 = ORIENTED_EDGE ( 'NONE', *, *, #33251, .F. ) ;
#49117 = LINE ( 'NONE', #24667, #14478 ) ;
#49118 = LINE ( 'NONE', #45188, #23083 ) ;
#49119 = EDGE_CURVE ( 'NONE', #44157, #36786, #48985, .T. ) ;
#49120 = CARTESIAN_POINT ( 'NONE',  ( -56.65322908700500903, -193.5000000000000000, -123.7303097900624493 ) ) ;
#49121 = EDGE_LOOP ( 'NONE', ( #2722, #47975, #17569, #37231 ) ) ;
#49122 = DIRECTION ( 'NONE',  ( 0.000000000000000000, 0.000000000000000000, 1.000000000000000000 ) ) ;
#49123 = ADVANCED_FACE ( 'NONE', ( #21650 ), #41871, .F. ) ;
#49124 = APPLICATION_PROTOCOL_DEFINITION ( 'draft international standard', 'automotive_design', 1998, #18627 ) ;
#49125 = FACE_OUTER_BOUND ( 'NONE', #9073, .T. ) ;
#49126 = DIRECTION ( 'NONE',  ( 0.5586467658036594619, 0.000000000000000000, -0.8294056854501971054 ) ) ;
#49127 = DIRECTION ( 'NONE',  ( 0.000000000000000000, 0.000000000000000000, 1.000000000000000000 ) ) ;
#49128 = CARTESIAN_POINT ( 'NONE',  ( 65.38692482895589819, -177.1207230881787780, -51.57055649762702387 ) ) ;
#49129 = EDGE_CURVE ( 'NONE', #31195, #15564, #17185, .T. ) ;
#49130 = DIRECTION ( 'NONE',  ( -0.000000000000000000, 1.000000000000000000, -0.000000000000000000 ) ) ;
#49131 = ORIENTED_EDGE ( 'NONE', *, *, #34958, .F. ) ;
#49132 = AXIS2_PLACEMENT_3D ( 'NONE', #45680, #25698, #4691 ) ;
#49133 = AXIS2_PLACEMENT_3D ( 'NONE', #51979, #48275, #43554 ) ;
#49134 = CARTESIAN_POINT ( 'NONE',  ( -48.47912675150885065, -187.5000000000000284, -14.99999999999999289 ) ) ;
#49135 = DIRECTION ( 'NONE',  ( -0.000000000000000000, -0.8854560256532126861, -0.4647231720437631775 ) ) ;
#49136 = ORIENTED_EDGE ( 'NONE', *, *, #16276, .T. ) ;
#49137 = ORIENTED_EDGE ( 'NONE', *, *, #32596, .T. ) ;
#49138 = EDGE_LOOP ( 'NONE', ( #41905, #21045, #7244, #1847 ) ) ;
#49139 = EDGE_CURVE ( 'NONE', #40790, #13171, #29769, .T. ) ;
#49140 = VECTOR ( 'NONE', #1997, 1000.000000000000000 ) ;
#49141 = DIRECTION ( 'NONE',  ( -0.9995608365087940150, 0.000000000000000000, -0.02963332782257007206 ) ) ;
#49142 = FACE_OUTER_BOUND ( 'NONE', #37595, .T. ) ;
#49143 = VECTOR ( 'NONE', #49615, 1000.000000000000114 ) ;
#49144 = CARTESIAN_POINT ( 'NONE',  ( -123.4791267515088435, -198.5000000000000000, 80.00000000000000000 ) ) ;
#49145 = DIRECTION ( 'NONE',  ( -0.6068001458185834363, 0.000000000000000000, -0.7948544414133608127 ) ) ;
#49146 = CIRCLE ( 'NONE', #9710, 10.00000000000000711 ) ;
#49147 = VERTEX_POINT ( 'NONE', #9815 ) ;
#49148 = VECTOR ( 'NONE', #39628, 999.9999999999998863 ) ;
#49149 = LINE ( 'NONE', #24441, #47846 ) ;
#49150 = DIRECTION ( 'NONE',  ( 0.9266896074318343723, 0.000000000000000000, -0.3758275821142357809 ) ) ;
#49151 = VERTEX_POINT ( 'NONE', #17712 ) ;
#49152 = AXIS2_PLACEMENT_3D ( 'NONE', #17169, #48970, #32916 ) ;
#49153 = DIRECTION ( 'NONE',  ( 0.000000000000000000, 1.000000000000000000, -0.000000000000000000 ) ) ;
#49154 = ORIENTED_EDGE ( 'NONE', *, *, #25952, .F. ) ;
#49155 = DIRECTION ( 'NONE',  ( 0.000000000000000000, 0.000000000000000000, 1.000000000000000000 ) ) ;
#49156 = ADVANCED_FACE ( 'NONE', ( #33479 ), #49248, .F. ) ;
#49157 = EDGE_CURVE ( 'NONE', #16904, #37128, #880, .T. ) ;
#49158 = EDGE_CURVE ( 'NONE', #49151, #32802, #5584, .T. ) ;
#49159 = EDGE_CURVE ( 'NONE', #28151, #13401, #32933, .T. ) ;
#49160 = PLANE ( 'NONE',  #17515 ) ;
#49161 = DIRECTION ( 'NONE',  ( 0.000000000000000000, -0.3546048870425396182, -0.9350162426854132791 ) ) ;
#49164 = ORIENTED_EDGE ( 'NONE', *, *, #48030, .F. ) ;
#49163 = DIRECTION ( 'NONE',  ( 1.000000000000000000, 0.000000000000000000, 0.000000000000000000 ) ) ;
#49162 = PLANE ( 'NONE',  #13245 ) ;
#49165 = DIRECTION ( 'NONE',  ( 0.000000000000000000, 0.8854560256532079121, -0.4647231720437725033 ) ) ;
#49166 = CIRCLE ( 'NONE', #23131, 125.0000000000000000 ) ;
#49167 = ORIENTED_EDGE ( 'NONE', *, *, #21395, .T. ) ;
#49168 = FACE_OUTER_BOUND ( 'NONE', #35232, .T. ) ;
#49169 = CARTESIAN_POINT ( 'NONE',  ( 46.00000000000000711, 20.00000000000000000, -41.00000000000000000 ) ) ;
#49170 = ORIENTED_EDGE ( 'NONE', *, *, #29022, .T. ) ;
#49171 = VECTOR ( 'NONE', #42591, 1000.000000000000114 ) ;
#49172 = CARTESIAN_POINT ( 'NONE',  ( -81.14588623932559130, -177.1207230881787780, 120.6560517527618117 ) ) ;
#49174 = DIRECTION ( 'NONE',  ( 0.000000000000000000, -1.000000000000000000, 0.000000000000000000 ) ) ;
#49173 = CARTESIAN_POINT ( 'NONE',  ( -12.76653800058364574, -189.7472609257535510, -119.7898618611244927 ) ) ;
#49175 = ORIENTED_EDGE ( 'NONE', *, *, #15375, .T. ) ;
#49176 = CARTESIAN_POINT ( 'NONE',  ( -5.142695285147754980, -189.7472609257535510, -116.1806952091177578 ) ) ;
#49177 = DIRECTION ( 'NONE',  ( -1.000000000000000000, 0.000000000000000000, 0.000000000000000000 ) ) ;
#49178 = CARTESIAN_POINT ( 'NONE',  ( -106.4764934152196645, -193.5000000000000000, 110.7307791902282759 ) ) ;
#49179 = EDGE_CURVE ( 'NONE', #42349, #42455, #13244, .T. ) ;
#49180 = ORIENTED_EDGE ( 'NONE', *, *, #10868, .T. ) ;
#49181 = AXIS2_PLACEMENT_3D ( 'NONE', #27367, #27876, #23942 ) ;
#49182 = CYLINDRICAL_SURFACE ( 'NONE', #38402, 125.0000000000000000 ) ;
#49183 = DIRECTION ( 'NONE',  ( 0.000000000000000000, 0.000000000000000000, -1.000000000000000000 ) ) ;
#49184 = LINE ( 'NONE', #29449, #16747 ) ;
#49185 = VECTOR ( 'NONE', #15642, 1000.000000000000000 ) ;
#49186 = DIRECTION ( 'NONE',  ( -0.5586467658036594619, 0.000000000000000000, 0.8294056854501971054 ) ) ;
#49187 = EDGE_LOOP ( 'NONE', ( #28982, #841, #40579, #33163 ) ) ;
#49188 = AXIS2_PLACEMENT_3D ( 'NONE', #32544, #20193, #44108 ) ;
#49189 = CARTESIAN_POINT ( 'NONE',  ( -305.0000000000000568, -183.4979166304964622, 0.4999999999996888600 ) ) ;
#49190 = CARTESIAN_POINT ( 'NONE',  ( 0.000000000000000000, 65.00000000000000000, 0.000000000000000000 ) ) ;
#49191 = EDGE_CURVE ( 'NONE', #21096, #6808, #25325, .T. ) ;
#49192 = CIRCLE ( 'NONE', #24866, 125.0000000000000000 ) ;
#49193 = LINE ( 'NONE', #48408, #11498 ) ;
#49194 = ORIENTED_EDGE ( 'NONE', *, *, #12653, .F. ) ;
#49195 = LINE ( 'NONE', #46043, #41568 ) ;
#49196 = DIRECTION ( 'NONE',  ( 0.000000000000000000, -1.000000000000000000, 0.000000000000000000 ) ) ;
#49197 = DIRECTION ( 'NONE',  ( 0.000000000000000000, 1.000000000000000000, 0.000000000000000000 ) ) ;
#49198 = DIRECTION ( 'NONE',  ( 0.000000000000000000, -1.000000000000000000, 0.000000000000000000 ) ) ;
#49199 = FACE_OUTER_BOUND ( 'NONE', #45257, .T. ) ;
#49200 = AXIS2_PLACEMENT_3D ( 'NONE', #11491, #11746, #24116 ) ;
#49201 = VECTOR ( 'NONE', #46728, 1000.000000000000114 ) ;
#49202 = CARTESIAN_POINT ( 'NONE',  ( -169.8550585387149852, -193.5000000000000000, 25.37485791684384751 ) ) ;
#49203 = DIRECTION ( 'NONE',  ( 0.000000000000000000, 0.000000000000000000, 1.000000000000000000 ) ) ;
#49205 = ORIENTED_EDGE ( 'NONE', *, *, #13436, .T. ) ;
#49204 = LINE ( 'NONE', #45276, #4385 ) ;
#49206 = VECTOR ( 'NONE', #820, 1000.000000000000114 ) ;
#49207 = AXIS2_PLACEMENT_3D ( 'NONE', #4513, #32094, #3994 ) ;
#49208 = ORIENTED_EDGE ( 'NONE', *, *, #36252, .T. ) ;
#49209 = DIRECTION ( 'NONE',  ( 0.000000000000000000, 0.4647231720437664526, -0.8854560256532110207 ) ) ;
#49210 = LINE ( 'NONE', #29734, #22948 ) ;
#49212 = ORIENTED_EDGE ( 'NONE', *, *, #26615, .F. ) ;
#49211 = CARTESIAN_POINT ( 'NONE',  ( -336.3521761649654422, -165.2193480479701293, -43.12187378178660424 ) ) ;
#49213 = ORIENTED_EDGE ( 'NONE', *, *, #2411, .F. ) ;
#49214 = VECTOR ( 'NONE', #7665, 1000.000000000000000 ) ;
#49215 = ORIENTED_EDGE ( 'NONE', *, *, #617, .T. ) ;
#49216 = LINE ( 'NONE', #21350, #4903 ) ;
#49217 = VECTOR ( 'NONE', #18297, 1000.000000000000000 ) ;
#49218 = CIRCLE ( 'NONE', #13120, 60.00000000000000000 ) ;
#49219 = ADVANCED_FACE ( 'NONE', ( #1925 ), #45568, .F. ) ;
#49221 = VECTOR ( 'NONE', #29871, 1000.000000000000114 ) ;
#49220 = CARTESIAN_POINT ( 'NONE',  ( -123.8574911141017765, -175.3837268820161057, 98.45863302693528851 ) ) ;
#49222 = CARTESIAN_POINT ( 'NONE',  ( -155.4465502054561057, -177.1207230881787780, 64.67588669375881238 ) ) ;
#49223 = ORIENTED_EDGE ( 'NONE', *, *, #7982, .F. ) ;
#49224 = AXIS2_PLACEMENT_3D ( 'NONE', #42634, #19480, #14267 ) ;
#49225 = DIRECTION ( 'NONE',  ( -0.9995608365087940150, 0.000000000000000000, -0.02963332782257007206 ) ) ;
#49227 = VERTEX_POINT ( 'NONE', #17964 ) ;
#49226 = CARTESIAN_POINT ( 'NONE',  ( -172.4195137048758397, -193.5000000000000000, -3.844569333772363873 ) ) ;
#49228 = CARTESIAN_POINT ( 'NONE',  ( -332.3517673607765914, -133.3383340306578759, -59.18789727217212970 ) ) ;
#49229 = ORIENTED_EDGE ( 'NONE', *, *, #49400, .F. ) ;
#49230 = LINE ( 'NONE', #13480, #15477 ) ;
#49231 = VERTEX_POINT ( 'NONE', #5360 ) ;
#49232 = CARTESIAN_POINT ( 'NONE',  ( 51.65665342072240662, -183.6283474603465606, 74.81861753132422166 ) ) ;
#49233 = PLANE ( 'NONE',  #9527 ) ;
#49234 = DIRECTION ( 'NONE',  ( -0.9473263538541876194, 0.000000000000000000, -0.3202698538628486746 ) ) ;
#49235 = ORIENTED_EDGE ( 'NONE', *, *, #11825, .F. ) ;
#49236 = AXIS2_PLACEMENT_3D ( 'NONE', #38758, #26157, #13831 ) ;
#49237 = ORIENTED_EDGE ( 'NONE', *, *, #42262, .F. ) ;
#49238 = CARTESIAN_POINT ( 'NONE',  ( -339.1964088526558498, -179.7763290203206452, 20.80804632820241906 ) ) ;
#49239 = AXIS2_PLACEMENT_3D ( 'NONE', #49528, #9315, #5642 ) ;
#49240 = LINE ( 'NONE', #37395, #27532 ) ;
#49241 = VERTEX_POINT ( 'NONE', #21378 ) ;
#49242 = EDGE_CURVE ( 'NONE', #14193, #9248, #12186, .T. ) ;
#49243 = DIRECTION ( 'NONE',  ( 0.000000000000000000, -0.000000000000000000, -1.000000000000000000 ) ) ;
#49244 = VECTOR ( 'NONE', #13434, 1000.000000000000114 ) ;
#49245 = DIRECTION ( 'NONE',  ( 0.000000000000000000, 0.000000000000000000, 1.000000000000000000 ) ) ;
#49246 = ORIENTED_EDGE ( 'NONE', *, *, #19405, .F. ) ;
#49247 = FACE_BOUND ( 'NONE', #21694, .T. ) ;
#49248 = PLANE ( 'NONE',  #38189 ) ;
#49249 = EDGE_LOOP ( 'NONE', ( #21866, #41838, #35166, #44055 ) ) ;
#49250 = DIRECTION ( 'NONE',  ( 0.000000000000000000, -0.8854560256532044704, 0.4647231720437789981 ) ) ;
#49251 = VERTEX_POINT ( 'NONE', #38442 ) ;
#49252 = AXIS2_PLACEMENT_3D ( 'NONE', #675, #24577, #12494 ) ;
#49253 = CARTESIAN_POINT ( 'NONE',  ( 75.02564229359539638, -189.7472609257535510, -19.27620354518634826 ) ) ;
#49254 = AXIS2_PLACEMENT_3D ( 'NONE', #40180, #47570, #51770 ) ;
#49255 = CARTESIAN_POINT ( 'NONE',  ( -48.47912675150885065, -189.7472609257535510, 6.938893903907228378E-15 ) ) ;
#49256 = VERTEX_POINT ( 'NONE', #19260 ) ;
#49257 = VECTOR ( 'NONE', #32148, 1000.000000000000114 ) ;
#49258 = VECTOR ( 'NONE', #30671, 1000.000000000000000 ) ;
#49259 = CARTESIAN_POINT ( 'NONE',  ( -133.0671220150036334, -177.1207230881787780, -92.03190238880748097 ) ) ;
#49260 = CARTESIAN_POINT ( 'NONE',  ( -330.4913330509368166, -63.99980407363855761, 7.728304129923846411 ) ) ;
#49261 = LINE ( 'NONE', #22436, #19037 ) ;
#49262 = ADVANCED_FACE ( 'NONE', ( #6658 ), #50289, .F. ) ;
#49263 = DIRECTION ( 'NONE',  ( -0.000000000000000000, -0.8229838658936596829, -0.5680647467311510379 ) ) ;
#49264 = ORIENTED_EDGE ( 'NONE', *, *, #9939, .F. ) ;
#49266 = AXIS2_PLACEMENT_3D ( 'NONE', #46270, #46782, #2375 ) ;
#49265 = CARTESIAN_POINT ( 'NONE',  ( -5.142695285147754980, -175.3837268820161057, -116.1806952091177578 ) ) ;
#49267 = ORIENTED_EDGE ( 'NONE', *, *, #24257, .T. ) ;
#49268 = ORIENTED_EDGE ( 'NONE', *, *, #35036, .T. ) ;
#49269 = DIRECTION ( 'NONE',  ( -0.000000000000000000, 1.000000000000000000, -0.000000000000000000 ) ) ;
#49271 = EDGE_LOOP ( 'NONE', ( #960, #2000, #49736, #35085 ) ) ;
#49270 = CARTESIAN_POINT ( 'NONE',  ( -339.1964088526558498, -130.1153096980144426, 58.63009191191295599 ) ) ;
#49272 = EDGE_LOOP ( 'NONE', ( #8730, #12849, #6890, #27768 ) ) ;
#49273 = CARTESIAN_POINT ( 'NONE',  ( -336.3521761649654422, -123.5000000000000284, 0.000000000000000000 ) ) ;
#49274 = EDGE_CURVE ( 'NONE', #32293, #23451, #22935, .T. ) ;
#49275 = FACE_OUTER_BOUND ( 'NONE', #50022, .T. ) ;
#49276 = FACE_OUTER_BOUND ( 'NONE', #38894, .T. ) ;
#49277 = AXIS2_PLACEMENT_3D ( 'NONE', #8515, #40566, #45068 ) ;
#49278 = ORIENTED_EDGE ( 'NONE', *, *, #47450, .T. ) ;
#49279 = DIRECTION ( 'NONE',  ( -0.000000000000000000, 1.000000000000000000, -0.000000000000000000 ) ) ;
#49280 = ORIENTED_EDGE ( 'NONE', *, *, #4258, .F. ) ;
#49281 = DIRECTION ( 'NONE',  ( 0.000000000000000000, -1.000000000000000000, 0.000000000000000000 ) ) ;
#49282 = FACE_OUTER_BOUND ( 'NONE', #38968, .T. ) ;
#49283 = AXIS2_PLACEMENT_3D ( 'NONE', #12924, #37363, #20827 ) ;
#49284 = EDGE_CURVE ( 'NONE', #49743, #19374, #34244, .T. ) ;
#49285 = FACE_OUTER_BOUND ( 'NONE', #32863, .T. ) ;
#49286 = CARTESIAN_POINT ( 'NONE',  ( -332.3517673607765914, -64.50000000000000000, -1.632288850093980725 ) ) ;
#49287 = ORIENTED_EDGE ( 'NONE', *, *, #36192, .T. ) ;
#49288 = ORIENTED_EDGE ( 'NONE', *, *, #10451, .T. ) ;
#49289 = VERTEX_POINT ( 'NONE', #6902 ) ;
#49290 = CARTESIAN_POINT ( 'NONE',  ( -171.7300019102062549, -183.6283474603465606, -20.83798868929510562 ) ) ;
#49291 = DIRECTION ( 'NONE',  ( 0.000000000000000000, 0.9709418174260544543, 0.2393156642875482742 ) ) ;
#49292 = VECTOR ( 'NONE', #27990, 1000.000000000000000 ) ;
#49293 = ADVANCED_FACE ( 'NONE', ( #15307 ), #15066, .F. ) ;
#49294 = VECTOR ( 'NONE', #27623, 1000.000000000000000 ) ;
#49295 = VECTOR ( 'NONE', #24214, 1000.000000000000000 ) ;
#49296 = CARTESIAN_POINT ( 'NONE',  ( -336.3521761649654422, -180.1556192733800117, 16.67542351306693149 ) ) ;
#49297 = DIRECTION ( 'NONE',  ( -0.000000000000000000, 1.000000000000000000, -0.000000000000000000 ) ) ;
#49298 = ORIENTED_EDGE ( 'NONE', *, *, #44942, .F. ) ;
#49299 = AXIS2_PLACEMENT_3D ( 'NONE', #31617, #39253, #75 ) ;
#49300 = AXIS2_PLACEMENT_3D ( 'NONE', #32551, #16015, #39635 ) ;
#49301 = EDGE_LOOP ( 'NONE', ( #20103, #2114, #31312, #31825 ) ) ;
#49303 = ORIENTED_EDGE ( 'NONE', *, *, #8678, .F. ) ;
#49302 = DIRECTION ( 'NONE',  ( 0.000000000000000000, 1.000000000000000000, 0.000000000000000000 ) ) ;
#49304 = ORIENTED_EDGE ( 'NONE', *, *, #44973, .T. ) ;
#49305 = CARTESIAN_POINT ( 'NONE',  ( 51.70113075622899856, 30.00000000000000355, -45.78969942005421956 ) ) ;
#49306 = ADVANCED_FACE ( 'NONE', ( #18475 ), #10329, .T. ) ;
#49307 = CARTESIAN_POINT ( 'NONE',  ( -25.72842157752850056, -193.5000000000000000, 121.8950816227734606 ) ) ;
#49308 = DIRECTION ( 'NONE',  ( -0.000000000000000000, -1.000000000000000000, 0.000000000000000000 ) ) ;
#49309 = CARTESIAN_POINT ( 'NONE',  ( -100.6109117578263152, -177.1207230881787780, 112.5098962032393359 ) ) ;
#49310 = CARTESIAN_POINT ( 'NONE',  ( -155.9608607592036833, -193.5000000000000000, 63.81752780153064464 ) ) ;
#49311 = ORIENTED_EDGE ( 'NONE', *, *, #35155, .T. ) ;
#49312 = DIRECTION ( 'NONE',  ( -0.6528221181905119463, 0.000000000000000000, -0.7575112421616284619 ) ) ;
#49313 = VERTEX_POINT ( 'NONE', #51075 ) ;
#49314 = ORIENTED_EDGE ( 'NONE', *, *, #4364, .F. ) ;
#49315 = DIRECTION ( 'NONE',  ( 0.000000000000000000, 0.000000000000000000, -1.000000000000000000 ) ) ;
#49316 = VECTOR ( 'NONE', #7788, 1000.000000000000227 ) ;
#49317 = VECTOR ( 'NONE', #222, 1000.000000000000114 ) ;
#49318 = DIRECTION ( 'NONE',  ( -0.9890401873221654760, 0.000000000000000000, 0.1476465640024710868 ) ) ;
#49319 = VERTEX_POINT ( 'NONE', #38171 ) ;
#49320 = AXIS2_PLACEMENT_3D ( 'NONE', #44425, #8413, #29412 ) ;
#49321 = CARTESIAN_POINT ( 'NONE',  ( -88.78924379339703421, -183.6283474603465606, -118.3219948448692804 ) ) ;
#49322 = DIRECTION ( 'NONE',  ( 0.000000000000000000, 0.000000000000000000, -1.000000000000000000 ) ) ;
#49323 = CARTESIAN_POINT ( 'NONE',  ( -330.4913330509368166, -182.1300919119129560, -6.615309698014691264 ) ) ;
#49324 = DIRECTION ( 'NONE',  ( -0.1768902751225733261, 0.000000000000000000, 0.9842305779475966077 ) ) ;
#49325 = LINE ( 'NONE', #20674, #31587 ) ;
#49326 = FACE_OUTER_BOUND ( 'NONE', #39743, .T. ) ;
#49327 = DIRECTION ( 'NONE',  ( -0.000000000000000000, -1.000000000000000000, -0.000000000000000000 ) ) ;
#49328 = EDGE_LOOP ( 'NONE', ( #37860, #34665, #17728, #4826 ) ) ;
#49329 = CIRCLE ( 'NONE', #30033, 125.0000000000000000 ) ;
#49330 = CIRCLE ( 'NONE', #29168, 125.0000000000000000 ) ;
#49331 = CARTESIAN_POINT ( 'NONE',  ( -98.31070548515593543, -189.7472609257535510, -113.5465278748093567 ) ) ;
#49332 = ORIENTED_EDGE ( 'NONE', *, *, #16342, .F. ) ;
#49333 = AXIS2_PLACEMENT_3D ( 'NONE', #37199, #13020, #29046 ) ;
#49334 = LINE ( 'NONE', #26876, #31978 ) ;
#49335 = EDGE_CURVE ( 'NONE', #20197, #42260, #2954, .T. ) ;
#49336 = ORIENTED_EDGE ( 'NONE', *, *, #20539, .F. ) ;
#49337 = ADVANCED_FACE ( 'NONE', ( #47368 ), #18992, .T. ) ;
#49338 = CARTESIAN_POINT ( 'NONE',  ( -18.95304271317703382, -175.3837268820161057, -121.4627941443854837 ) ) ;
#49339 = CIRCLE ( 'NONE', #6424, 125.0000000000000000 ) ;
#49340 = VERTEX_POINT ( 'NONE', #22677 ) ;
#49341 = VECTOR ( 'NONE', #45479, 1000.000000000000000 ) ;
#49342 = DIRECTION ( 'NONE',  ( 0.1768902751225666370, 0.000000000000000000, 0.9842305779475979399 ) ) ;
#49343 = FACE_BOUND ( 'NONE', #3621, .T. ) ;
#49345 = ORIENTED_EDGE ( 'NONE', *, *, #51024, .T. ) ;
#49344 = CARTESIAN_POINT ( 'NONE',  ( 69.88207517204678254, -175.3837268820161057, 40.19484891390058579 ) ) ;
#49346 = ADVANCED_FACE ( 'NONE', ( #26862 ), #46343, .F. ) ;
#49347 = FACE_OUTER_BOUND ( 'NONE', #139, .T. ) ;
#49348 = ORIENTED_EDGE ( 'NONE', *, *, #12317, .F. ) ;
#49349 = VERTEX_POINT ( 'NONE', #47112 ) ;
#49350 = EDGE_CURVE ( 'NONE', #44102, #40165, #2180, .T. ) ;
#49351 = ORIENTED_EDGE ( 'NONE', *, *, #15645, .T. ) ;
#49352 = FACE_OUTER_BOUND ( 'NONE', #46181, .T. ) ;
#49353 = AXIS2_PLACEMENT_3D ( 'NONE', #29043, #33260, #17514 ) ;
#49354 = CARTESIAN_POINT ( 'NONE',  ( -336.3521761649653854, -103.7577981350106313, -56.65902810251876787 ) ) ;
#49355 = VECTOR ( 'NONE', #1194, 1000.000000000000000 ) ;
#49356 = EDGE_CURVE ( 'NONE', #19121, #12363, #27378, .T. ) ;
#49357 = ORIENTED_EDGE ( 'NONE', *, *, #49356, .F. ) ;
#49358 = DIRECTION ( 'NONE',  ( 1.000000000000000000, -0.000000000000000000, -0.000000000000000000 ) ) ;
#49359 = DIRECTION ( 'NONE',  ( -0.000000000000000000, 0.3546048870425235200, -0.9350162426854194964 ) ) ;
#49360 = EDGE_LOOP ( 'NONE', ( #37689, #17490, #8219, #40848 ) ) ;
#49361 = VECTOR ( 'NONE', #2724, 1000.000000000000000 ) ;
#49362 = EDGE_CURVE ( 'NONE', #37884, #19283, #10583, .T. ) ;
#49363 = CARTESIAN_POINT ( 'NONE',  ( -60.00000000000000000, -43.50000000000000000, -60.00000000000000711 ) ) ;
#49364 = CARTESIAN_POINT ( 'NONE',  ( 26.62880456707186028, -193.5000000000000000, 98.66508442481510599 ) ) ;
#49365 = VERTEX_POINT ( 'NONE', #38689 ) ;
#49368 = VERTEX_POINT ( 'NONE', #43429 ) ;
#49367 = LINE ( 'NONE', #45419, #21447 ) ;
#49366 = CARTESIAN_POINT ( 'NONE',  ( -332.3517673607765914, -101.0520950768976149, 54.58714071513087873 ) ) ;
#49369 = VECTOR ( 'NONE', #11375, 1000.000000000000000 ) ;
#49370 = ORIENTED_EDGE ( 'NONE', *, *, #24652, .F. ) ;
#49371 = ORIENTED_EDGE ( 'NONE', *, *, #51070, .F. ) ;
#49372 = DIRECTION ( 'NONE',  ( 0.000000000000000000, 1.000000000000000000, -0.000000000000000000 ) ) ;
#49373 = EDGE_LOOP ( 'NONE', ( #10764, #17189, #37728, #22322 ) ) ;
#49374 = CARTESIAN_POINT ( 'NONE',  ( -330.4913330509368166, -138.1050951016791544, -57.16590939599326049 ) ) ;
#49375 = LINE ( 'NONE', #21249, #14971 ) ;
#49376 = ORIENTED_EDGE ( 'NONE', *, *, #38521, .T. ) ;
#49377 = CARTESIAN_POINT ( 'NONE',  ( -170.0000000000000284, -123.5000000000000284, 6.938893903907228378E-15 ) ) ;
#49378 = ORIENTED_EDGE ( 'NONE', *, *, #31386, .T. ) ;
#49379 = VECTOR ( 'NONE', #13168, 999.9999999999998863 ) ;
#49380 = ORIENTED_EDGE ( 'NONE', *, *, #44001, .F. ) ;
#49381 = FACE_OUTER_BOUND ( 'NONE', #24275, .T. ) ;
#49382 = LINE ( 'NONE', #16544, #50032 ) ;
#49383 = DIRECTION ( 'NONE',  ( 0.000000000000000000, 0.000000000000000000, 1.000000000000000000 ) ) ;
#49384 =( NAMED_UNIT ( * ) PLANE_ANGLE_UNIT ( ) SI_UNIT ( $, .RADIAN. ) );
#49385 = ORIENTED_EDGE ( 'NONE', *, *, #19716, .T. ) ;
#49386 = CARTESIAN_POINT ( 'NONE',  ( -27.36201831380533989, -193.5000000000000000, -122.1886788576022411 ) ) ;
#49387 = DIRECTION ( 'NONE',  ( 0.000000000000000000, -1.000000000000000000, 0.000000000000000000 ) ) ;
#49388 = ITEM_DEFINED_TRANSFORMATION ( 'NONE', 'NONE', #35983,  #31742 ) ;
#49389 = CARTESIAN_POINT ( 'NONE',  ( 64.44365795514079309, -193.5000000000000000, -53.60452120946194299 ) ) ;
#49390 = CARTESIAN_POINT ( 'NONE',  ( 58.48829670243886625, -177.1207230881787780, -64.67588669375805921 ) ) ;
#49391 = DIRECTION ( 'NONE',  ( -0.000000000000000000, 0.9350162426854194964, 0.3546048870425235200 ) ) ;
#49392 = CARTESIAN_POINT ( 'NONE',  ( -213.8817838414232426, -193.5000000000000000, 2.819679052520814125E-14 ) ) ;
#49393 = LINE ( 'NONE', #5776, #13159 ) ;
#49394 = VERTEX_POINT ( 'NONE', #43154 ) ;
#49395 = AXIS2_PLACEMENT_3D ( 'NONE', #32925, #44774, #13750 ) ;
#49396 = ORIENTED_EDGE ( 'NONE', *, *, #259, .T. ) ;
#49397 = AXIS2_PLACEMENT_3D ( 'NONE', #45817, #37922, #13495 ) ;
#49398 = PRESENTATION_LAYER_ASSIGNMENT (  '', '', ( #13294 ) ) ;
#49399 = AXIS2_PLACEMENT_3D ( 'NONE', #30014, #17685, #24768 ) ;
#49400 = EDGE_CURVE ( 'NONE', #14548, #43146, #7434, .T. ) ;
#49401 = CARTESIAN_POINT ( 'NONE',  ( -332.3517673607765914, -123.5000000000000284, 0.000000000000000000 ) ) ;
#49402 = CARTESIAN_POINT ( 'NONE',  ( 75.48825557695654709, -175.3837268820161057, 2.844930291601486694 ) ) ;
#49403 = EDGE_CURVE ( 'NONE', #39091, #11866, #46864, .T. ) ;
#49404 = EDGE_LOOP ( 'NONE', ( #11266, #5401, #17435, #36018 ) ) ;
#49405 = ADVANCED_FACE ( 'NONE', ( #23199 ), #31323, .F. ) ;
#49406 = CARTESIAN_POINT ( 'NONE',  ( -332.3517673607765914, -106.5990858529439578, 57.57047073799066794 ) ) ;
#49407 = EDGE_LOOP ( 'NONE', ( #9648, #3135, #36943, #9608 ) ) ;
#49408 = ADVANCED_FACE ( 'NONE', ( #47 ), #32098, .F. ) ;
#49409 = ADVANCED_FACE ( 'NONE', ( #51840 ), #8196, .F. ) ;
#49410 = CIRCLE ( 'NONE', #25906, 125.0000000000000000 ) ;
#49411 = FACE_OUTER_BOUND ( 'NONE', #9137, .T. ) ;
#49412 = EDGE_CURVE ( 'NONE', #16981, #29431, #44195, .T. ) ;
#49413 = PLANE ( 'NONE',  #15297 ) ;
#49414 = DIRECTION ( 'NONE',  ( -0.000000000000000000, 1.000000000000000000, -0.000000000000000000 ) ) ;
#49415 = CARTESIAN_POINT ( 'NONE',  ( 30.67449672666758431, -177.1207230881787780, 95.45105364470144593 ) ) ;
#49416 = ADVANCED_FACE ( 'NONE', ( #7674 ), #35518, .F. ) ;
#49417 = ORIENTED_EDGE ( 'NONE', *, *, #46546, .T. ) ;
#49418 = DIRECTION ( 'NONE',  ( 0.000000000000000000, 0.6631226582407937498, -0.7485107481711024136 ) ) ;
#49419 = EDGE_CURVE ( 'NONE', #12178, #11142, #7174, .T. ) ;
#49420 = CARTESIAN_POINT ( 'NONE',  ( -332.3517673607765914, -176.9651911376907094, -25.08789112700655721 ) ) ;
#49421 = ORIENTED_EDGE ( 'NONE', *, *, #6108, .T. ) ;
#49422 = ADVANCED_FACE ( 'NONE', ( #27648 ), #47635, .F. ) ;
#49423 = VECTOR ( 'NONE', #12829, 1000.000000000000000 ) ;
#49424 = PLANE ( 'NONE',  #18935 ) ;
#49425 = VERTEX_POINT ( 'NONE', #24228 ) ;
#49426 = LINE ( 'NONE', #29417, #30070 ) ;
#49427 = EDGE_CURVE ( 'NONE', #12206, #19921, #7922, .T. ) ;
#49428 = ORIENTED_EDGE ( 'NONE', *, *, #13621, .F. ) ;
#49429 = DIRECTION ( 'NONE',  ( 0.000000000000000000, 0.9709418174260511236, -0.2393156642875615969 ) ) ;
#49430 = EDGE_CURVE ( 'NONE', #43701, #3626, #48144, .T. ) ;
#49431 = ORIENTED_EDGE ( 'NONE', *, *, #42039, .F. ) ;
#49432 = DIRECTION ( 'NONE',  ( 1.000000000000000000, -0.000000000000000000, -0.000000000000000000 ) ) ;
#49433 = DIRECTION ( 'NONE',  ( 1.000000000000000000, 0.000000000000000000, 0.000000000000000000 ) ) ;
#49434 = ORIENTED_EDGE ( 'NONE', *, *, #50112, .F. ) ;
#49435 =( GEOMETRIC_REPRESENTATION_CONTEXT ( 3 ) GLOBAL_UNCERTAINTY_ASSIGNED_CONTEXT ( ( #51612 ) ) GLOBAL_UNIT_ASSIGNED_CONTEXT ( ( #44130, #18926, #34941 ) ) REPRESENTATION_CONTEXT ( 'NONE', 'WORKASPACE' ) );
#49438 = VERTEX_POINT ( 'NONE', #4252 ) ;
#49437 = DIRECTION ( 'NONE',  ( 0.1768902751225592818, 0.000000000000000000, 0.9842305779475992722 ) ) ;
#49436 = DIRECTION ( 'NONE',  ( -0.5315839928299663786, 0.000000000000000000, 0.8470055835512244613 ) ) ;
#49439 = VECTOR ( 'NONE', #19494, 1000.000000000000114 ) ;
#49440 = VECTOR ( 'NONE', #26256, 1000.000000000000000 ) ;
#49441 = CARTESIAN_POINT ( 'NONE',  ( 68.21542617880035664, -177.1207230881787780, 41.93543928473692262 ) ) ;
#49442 = EDGE_LOOP ( 'NONE', ( #27330, #1826, #42914, #50345 ) ) ;
#49443 = CARTESIAN_POINT ( 'NONE',  ( -48.47912675150885065, -177.1207230881787780, 6.938893903907228378E-15 ) ) ;
#49444 = VECTOR ( 'NONE', #32594, 1000.000000000000000 ) ;
#49445 = ORIENTED_EDGE ( 'NONE', *, *, #10349, .F. ) ;
#49446 = CARTESIAN_POINT ( 'NONE',  ( 15.23368049493604381, -175.3837268820161057, -107.5438431188757420 ) ) ;
#49449 = VERTEX_POINT ( 'NONE', #32627 ) ;
#49448 = CARTESIAN_POINT ( 'NONE',  ( -47.51449116960048968, -193.5000000000000000, 0.2635871660690785045 ) ) ;
#49447 = LINE ( 'NONE', #21579, #22441 ) ;
#49450 = ADVANCED_FACE ( 'NONE', ( #36300 ), #39971, .F. ) ;
#49451 = ORIENTED_EDGE ( 'NONE', *, *, #31055, .F. ) ;
#49452 = AXIS2_PLACEMENT_3D ( 'NONE', #41697, #42467, #22518 ) ;
#49453 = DIRECTION ( 'NONE',  ( 0.000000000000000000, 0.000000000000000000, -1.000000000000000000 ) ) ;
#49454 = CARTESIAN_POINT ( 'NONE',  ( 42.96730897722186171, 30.00000000000000355, -41.16782622478179832 ) ) ;
#49455 = CARTESIAN_POINT ( 'NONE',  ( -48.47912675150885065, -175.3837268820161057, 6.938893903907228378E-15 ) ) ;
#49456 = EDGE_LOOP ( 'NONE', ( #24634, #30110, #45128, #40667 ) ) ;
#49457 = CARTESIAN_POINT ( 'NONE',  ( 52.98246549829695340, -193.5000000000000000, 73.01058346660533971 ) ) ;
#49458 = DIRECTION ( 'NONE',  ( 0.000000000000000000, 0.000000000000000000, -1.000000000000000000 ) ) ;
#49459 = CARTESIAN_POINT ( 'NONE',  ( -336.3521761649654422, -182.3871109312487420, -4.498567634386014369 ) ) ;
#49460 = CARTESIAN_POINT ( 'NONE',  ( -339.1964088526558498, -74.65991953890876687, -33.10432812419148263 ) ) ;
#49461 = VERTEX_POINT ( 'NONE', #28667 ) ;
#49462 = FACE_OUTER_BOUND ( 'NONE', #30964, .T. ) ;
#49463 = DIRECTION ( 'NONE',  ( -0.2348860457809707758, 0.000000000000000000, -0.9720229140804138579 ) ) ;
#49464 = CIRCLE ( 'NONE', #24229, 125.0000000000000000 ) ;
#49465 = EDGE_CURVE ( 'NONE', #8505, #21100, #27893, .T. ) ;
#49466 = DIRECTION ( 'NONE',  ( -1.000000000000000000, 0.000000000000000000, 0.000000000000000000 ) ) ;
#49467 = ORIENTED_EDGE ( 'NONE', *, *, #19209, .T. ) ;
#49468 = CARTESIAN_POINT ( 'NONE',  ( 62.43652093785069468, -193.5000000000000000, 55.44293326708522329 ) ) ;
#49469 = PLANE ( 'NONE',  #49621 ) ;
#49470 = ADVANCED_FACE ( 'NONE', ( #43930 ), #44718, .T. ) ;
#49471 = DIRECTION ( 'NONE',  ( 0.000000000000000000, -1.000000000000000000, 0.000000000000000000 ) ) ;
#49472 = CARTESIAN_POINT ( 'NONE',  ( -339.1964088526558498, -171.7720157143598669, 33.92731199008546383 ) ) ;
#49473 = EDGE_CURVE ( 'NONE', #20303, #35874, #36048, .T. ) ;
#49474 = ADVANCED_FACE ( 'NONE', ( #43676 ), #23456, .T. ) ;
#49475 = EDGE_CURVE ( 'NONE', #11500, #4839, #8447, .T. ) ;
#49476 = FACE_OUTER_BOUND ( 'NONE', #36017, .T. ) ;
#49477 = AXIS2_PLACEMENT_3D ( 'NONE', #6553, #43308, #39604 ) ;
#49478 = LINE ( 'NONE', #28680, #33711 ) ;
#49479 = LINE ( 'NONE', #29468, #4408 ) ;
#49481 = ORIENTED_EDGE ( 'NONE', *, *, #40919, .T. ) ;
#49480 = DIRECTION ( 'NONE',  ( -8.718379230999708359E-17, -0.9709418174260544543, -0.2393156642875482742 ) ) ;
#49482 = AXIS2_PLACEMENT_3D ( 'NONE', #8039, #31694, #19866 ) ;
#49483 = ORIENTED_EDGE ( 'NONE', *, *, #15046, .F. ) ;
#49484 = CARTESIAN_POINT ( 'NONE',  ( 1.150725574412418739, -175.3837268820161057, -114.7252272087845881 ) ) ;
#49485 = EDGE_CURVE ( 'NONE', #16796, #48776, #24475, .T. ) ;
#49486 = CARTESIAN_POINT ( 'NONE',  ( -84.19171550243319757, -193.5000000000000000, 119.7898618611247628 ) ) ;
#49488 = ORIENTED_EDGE ( 'NONE', *, *, #13450, .T. ) ;
#49487 = DIRECTION ( 'NONE',  ( 0.000000000000000000, 0.000000000000000000, -1.000000000000000000 ) ) ;
#49489 = ORIENTED_EDGE ( 'NONE', *, *, #48160, .T. ) ;
#49490 = ADVANCED_FACE ( 'NONE', ( #41027 ), #1080, .F. ) ;
#49491 = ORIENTED_EDGE ( 'NONE', *, *, #36433, .T. ) ;
#49492 = CARTESIAN_POINT ( 'NONE',  ( -47.87232660569025455, -177.1207230881787780, -0.7948544414133454916 ) ) ;
#49493 = ADVANCED_FACE ( 'NONE', ( #45507 ), #32873, .T. ) ;
#49494 = CARTESIAN_POINT ( 'NONE',  ( -48.47912675150885065, -173.5000000000000284, -14.99999999999999289 ) ) ;
#49495 = DIRECTION ( 'NONE',  ( -0.9890401873221633666, 0.000000000000000000, -0.1476465640024850756 ) ) ;
#49496 = EDGE_LOOP ( 'NONE', ( #6075, #6307, #41142, #11094 ) ) ;
#49497 = EDGE_CURVE ( 'NONE', #17350, #7135, #11359, .T. ) ;
#49498 = VECTOR ( 'NONE', #34686, 1000.000000000000000 ) ;
#49499 = FACE_OUTER_BOUND ( 'NONE', #3808, .T. ) ;
#49501 = EDGE_LOOP ( 'NONE', ( #27381, #51433, #1560, #25184 ) ) ;
#49500 = PLANE ( 'NONE',  #50164 ) ;
#49502 = DIRECTION ( 'NONE',  ( 0.000000000000000000, 0.8229838658936575735, 0.5680647467311540355 ) ) ;
#49503 = VERTEX_POINT ( 'NONE', #9499 ) ;
#49504 = DIRECTION ( 'NONE',  ( 0.000000000000000000, 1.000000000000000000, 0.000000000000000000 ) ) ;
#49505 = EDGE_LOOP ( 'NONE', ( #13056, #34546, #6674, #35651 ) ) ;
#49506 = DIRECTION ( 'NONE',  ( 0.7948544414133565938, 0.000000000000000000, -0.6068001458185890984 ) ) ;
#49507 = DIRECTION ( 'NONE',  ( -0.6068001458185945385, 0.000000000000000000, 0.7948544414133523750 ) ) ;
#49508 = CARTESIAN_POINT ( 'NONE',  ( -169.2746641285359317, -175.3837268820161057, -32.14713283941905786 ) ) ;
#49509 = EDGE_CURVE ( 'NONE', #43537, #16076, #44991, .T. ) ;
#49510 = EDGE_LOOP ( 'NONE', ( #49517, #7636, #19840, #39237 ) ) ;
#49511 = ORIENTED_EDGE ( 'NONE', *, *, #37704, .F. ) ;
#49512 = CARTESIAN_POINT ( 'NONE',  ( -260.0000000000000000, -93.50000000000001421, -51.54700538379269403 ) ) ;
#49514 = VECTOR ( 'NONE', #15146, 1000.000000000000000 ) ;
#49513 = DIRECTION ( 'NONE',  ( -0.000000000000000000, 1.000000000000000000, -0.000000000000000000 ) ) ;
#49515 = VERTEX_POINT ( 'NONE', #21593 ) ;
#49516 = CARTESIAN_POINT ( 'NONE',  ( 8.750818922897904528, -189.7472609257535510, -111.1293539894138434 ) ) ;
#49517 = ORIENTED_EDGE ( 'NONE', *, *, #23976, .T. ) ;
#49518 = CARTESIAN_POINT ( 'NONE',  ( -339.1964088526558498, -167.3305728129742249, 39.49849221029288060 ) ) ;
#49519 = DIRECTION ( 'NONE',  ( -1.000000000000000000, 0.000000000000000000, -0.000000000000000000 ) ) ;
#49520 = ORIENTED_EDGE ( 'NONE', *, *, #47213, .T. ) ;
#49521 = DIRECTION ( 'NONE',  ( 0.1768902751225666370, 0.000000000000000000, 0.9842305779475979399 ) ) ;
#49522 = EDGE_LOOP ( 'NONE', ( #48228, #8925, #27790, #36610 ) ) ;
#49523 = CARTESIAN_POINT ( 'NONE',  ( -173.3294908491238004, -177.1207230881787780, -6.114457023560960991 ) ) ;
#49524 = PLANE ( 'NONE',  #22830 ) ;
#49525 = ORIENTED_EDGE ( 'NONE', *, *, #28306, .F. ) ;
#49526 = PLANE ( 'NONE',  #34087 ) ;
#49527 = DIRECTION ( 'NONE',  ( 1.000000000000000000, -0.000000000000000000, 0.000000000000000000 ) ) ;
#49528 = CARTESIAN_POINT ( 'NONE',  ( -47.53180039765465636, -189.7472609257535510, -0.3202698538628280800 ) ) ;
#49529 = EDGE_CURVE ( 'NONE', #27596, #11286, #25268, .T. ) ;
#49530 = EDGE_CURVE ( 'NONE', #46184, #42344, #41818, .T. ) ;
#49531 = CARTESIAN_POINT ( 'NONE',  ( -48.13092511607445800, -175.3837268820161057, 0.9374196611341301111 ) ) ;
#49532 = VECTOR ( 'NONE', #20703, 1000.000000000000114 ) ;
#49533 = VERTEX_POINT ( 'NONE', #5046 ) ;
#49534 = CIRCLE ( 'NONE', #35237, 60.00000000000000000 ) ;
#49535 = DIRECTION ( 'NONE',  ( -0.000000000000000000, -1.000000000000000000, 0.000000000000000000 ) ) ;
#49536 = ORIENTED_EDGE ( 'NONE', *, *, #51246, .F. ) ;
#49537 = ORIENTED_EDGE ( 'NONE', *, *, #44788, .T. ) ;
#49538 = LINE ( 'NONE', #41890, #27704 ) ;
#49540 = ORIENTED_EDGE ( 'NONE', *, *, #10535, .F. ) ;
#49539 = LINE ( 'NONE', #37422, #6901 ) ;
#49541 = EDGE_LOOP ( 'NONE', ( #42151, #32680, #17921, #7518 ) ) ;
#49542 = LINE ( 'NONE', #45078, #19818 ) ;
#49543 = PLANE ( 'NONE',  #34676 ) ;
#49544 = ORIENTED_EDGE ( 'NONE', *, *, #35915, .T. ) ;
#49545 = VECTOR ( 'NONE', #38131, 1000.000000000000114 ) ;
#49546 = CARTESIAN_POINT ( 'NONE',  ( -48.47912675150885065, -183.6283474603465606, 6.938893903907228378E-15 ) ) ;
#49547 = EDGE_CURVE ( 'NONE', #17630, #45109, #33916, .T. ) ;
#49548 = VERTEX_POINT ( 'NONE', #49964 ) ;
#49549 = DIRECTION ( 'NONE',  ( 0.000000000000000000, -0.8660254037844378194, -0.5000000000000012212 ) ) ;
#49550 = DIRECTION ( 'NONE',  ( 0.000000000000000000, 0.000000000000000000, -1.000000000000000000 ) ) ;
#49551 = DIRECTION ( 'NONE',  ( 1.000000000000000000, 0.000000000000000000, 0.000000000000000000 ) ) ;
#49552 = LINE ( 'NONE', #45606, #19871 ) ;
#49553 = VERTEX_POINT ( 'NONE', #25785 ) ;
#49554 = ORIENTED_EDGE ( 'NONE', *, *, #33967, .F. ) ;
#49555 = EDGE_CURVE ( 'NONE', #30281, #24385, #5568, .T. ) ;
#49556 = ORIENTED_EDGE ( 'NONE', *, *, #32735, .T. ) ;
#49557 = CARTESIAN_POINT ( 'NONE',  ( -111.8989814360438828, -193.5000000000000000, -107.7168604805787027 ) ) ;
#49558 = FACE_OUTER_BOUND ( 'NONE', #30636, .T. ) ;
#49559 = FACE_OUTER_BOUND ( 'NONE', #15905, .T. ) ;
#49560 = PLANE ( 'NONE',  #2879 ) ;
#49561 = ORIENTED_EDGE ( 'NONE', *, *, #39098, .T. ) ;
#49562 = VECTOR ( 'NONE', #9275, 1000.000000000000114 ) ;
#49563 = AXIS2_PLACEMENT_3D ( 'NONE', #5313, #36842, #45268 ) ;
#49564 = ORIENTED_EDGE ( 'NONE', *, *, #1739, .T. ) ;
#49566 = ORIENTED_EDGE ( 'NONE', *, *, #5233, .T. ) ;
#49565 = PLANE ( 'NONE',  #42411 ) ;
#49567 = EDGE_LOOP ( 'NONE', ( #13984, #48830, #30939, #29867 ) ) ;
#49568 = CARTESIAN_POINT ( 'NONE',  ( 74.00867759460086859, -193.5000000000000000, 24.93467037017222410 ) ) ;
#49569 = CARTESIAN_POINT ( 'NONE',  ( -78.64590280292341617, -193.5000000000000000, -121.3052580173827408 ) ) ;
#49570 = CARTESIAN_POINT ( 'NONE',  ( -339.1964088526558498, -84.00150778970699150, 43.83057281297409702 ) ) ;
#49571 = DIRECTION ( 'NONE',  ( -1.000000000000000000, -1.013386094502324141E-14, -2.497772389992512055E-15 ) ) ;
#49572 = ORIENTED_EDGE ( 'NONE', *, *, #50354, .T. ) ;
#49573 = CARTESIAN_POINT ( 'NONE',  ( -49.08592689732743963, -175.3837268820161057, -0.7948544414133539293 ) ) ;
#49574 = EDGE_LOOP ( 'NONE', ( #16243, #4002, #2415, #27344 ) ) ;
#49575 = EDGE_LOOP ( 'NONE', ( #40525, #12259, #36544, #30125 ) ) ;
#49576 = LINE ( 'NONE', #5170, #39647 ) ;
#49577 = VECTOR ( 'NONE', #48575, 1000.000000000000000 ) ;
#49578 = DIRECTION ( 'NONE',  ( 0.000000000000000000, 0.000000000000000000, 1.000000000000000000 ) ) ;
#49579 = ORIENTED_EDGE ( 'NONE', *, *, #33329, .F. ) ;
#49580 = DIRECTION ( 'NONE',  ( -0.000000000000000000, 1.000000000000000000, -0.000000000000000000 ) ) ;
#49581 = CARTESIAN_POINT ( 'NONE',  ( -48.47912675150885065, -183.6283474603465606, 6.938893903907228378E-15 ) ) ;
#49582 = DIRECTION ( 'NONE',  ( -0.7575112421616191360, 0.000000000000000000, -0.6528221181905227155 ) ) ;
#49583 = EDGE_CURVE ( 'NONE', #36418, #35955, #21061, .T. ) ;
#49584 = DIRECTION ( 'NONE',  ( -0.000000000000000000, 1.000000000000000000, -1.541976423090494894E-16 ) ) ;
#49585 = CARTESIAN_POINT ( 'NONE',  ( -141.2664123866436512, -193.5000000000000000, -83.75869879877495805 ) ) ;
#49586 = FACE_BOUND ( 'NONE', #45211, .T. ) ;
#49587 = ORIENTED_EDGE ( 'NONE', *, *, #13571, .F. ) ;
#49588 = DIRECTION ( 'NONE',  ( -0.000000000000000000, -0.3546048870425396182, -0.9350162426854132791 ) ) ;
#49589 = ORIENTED_EDGE ( 'NONE', *, *, #38478, .T. ) ;
#49590 = CIRCLE ( 'NONE', #4259, 125.0000000000000000 ) ;
#49591 = ORIENTED_EDGE ( 'NONE', *, *, #38587, .T. ) ;
#49592 = CARTESIAN_POINT ( 'NONE',  ( 0.000000000000000000, -74.94395191227387443, 33.51582005713760282 ) ) ;
#49593 = VERTEX_POINT ( 'NONE', #13959 ) ;
#49594 = CIRCLE ( 'NONE', #26915, 60.00000000000000000 ) ;
#49595 = CARTESIAN_POINT ( 'NONE',  ( -88.78924379339714790, -177.1207230881787780, -118.3219948448692520 ) ) ;
#49596 = CARTESIAN_POINT ( 'NONE',  ( 50.27798938500056636, -193.5000000000000000, 74.98773087994526065 ) ) ;
#49598 = EDGE_LOOP ( 'NONE', ( #34802, #1318, #3958, #590 ) ) ;
#49597 = PLANE ( 'NONE',  #19530 ) ;
#49599 = ADVANCED_FACE ( 'NONE', ( #29984 ), #29714, .F. ) ;
#49600 = DIRECTION ( 'NONE',  ( 0.000000000000000000, 1.000000000000000000, -0.000000000000000000 ) ) ;
#49601 = ORIENTED_EDGE ( 'NONE', *, *, #51709, .T. ) ;
#49602 = ORIENTED_EDGE ( 'NONE', *, *, #7626, .T. ) ;
#49603 = VERTEX_POINT ( 'NONE', #17131 ) ;
#49604 = DIRECTION ( 'NONE',  ( 0.000000000000000000, 0.000000000000000000, 1.000000000000000000 ) ) ;
#49605 = CARTESIAN_POINT ( 'NONE',  ( -336.3521761649653854, -79.68838513426354098, -40.99441916720346057 ) ) ;
#49606 = AXIS2_PLACEMENT_3D ( 'NONE', #3260, #15343, #26897 ) ;
#49607 = EDGE_LOOP ( 'NONE', ( #48005, #37309, #45819, #8552 ) ) ;
#49608 = CARTESIAN_POINT ( 'NONE',  ( 44.30815888362531041, -175.3837268820161057, 83.75869879877569701 ) ) ;
#49609 = LINE ( 'NONE', #46442, #30345 ) ;
#49610 = LINE ( 'NONE', #33316, #3692 ) ;
#49611 = ORIENTED_EDGE ( 'NONE', *, *, #34784, .F. ) ;
#49612 = LINE ( 'NONE', #1769, #2419 ) ;
#49613 = CARTESIAN_POINT ( 'NONE',  ( -48.47912675150885065, -189.7472609257535510, 6.938893903907228378E-15 ) ) ;
#49614 = ORIENTED_EDGE ( 'NONE', *, *, #20569, .T. ) ;
#49616 = ORIENTED_EDGE ( 'NONE', *, *, #31283, .F. ) ;
#49615 = DIRECTION ( 'NONE',  ( -0.8124868780056863082, 0.000000000000000000, 0.5829794791144649047 ) ) ;
#49617 = VERTEX_POINT ( 'NONE', #25518 ) ;
#49618 = EDGE_LOOP ( 'NONE', ( #2962, #33456, #39762, #1759 ) ) ;
#49619 = CARTESIAN_POINT ( 'NONE',  ( -336.3521761649654422, -141.9604555052315220, 56.09938080879057765 ) ) ;
#49620 = DIRECTION ( 'NONE',  ( 0.000000000000000000, 0.6631226582407863113, -0.7485107481711089639 ) ) ;
#49621 = AXIS2_PLACEMENT_3D ( 'NONE', #2399, #26293, #13447 ) ;
#49622 = VERTEX_POINT ( 'NONE', #17403 ) ;
#49623 = ADVANCED_FACE ( 'NONE', ( #827 ), #33141, .T. ) ;
#49624 = FACE_OUTER_BOUND ( 'NONE', #32771, .T. ) ;
#49625 = CARTESIAN_POINT ( 'NONE',  ( -147.6585554144535024, -177.1207230881787780, 76.08180419845385245 ) ) ;
#49626 = EDGE_LOOP ( 'NONE', ( #37156, #24395, #19155, #49601 ) ) ;
#49627 = CARTESIAN_POINT ( 'NONE',  ( -365.0000000000001137, -168.5000000000000284, 0.000000000000000000 ) ) ;
#49628 = ORIENTED_EDGE ( 'NONE', *, *, #19778, .T. ) ;
#49629 = AXIS2_PLACEMENT_3D ( 'NONE', #4151, #719, #29074 ) ;
#49630 = EDGE_CURVE ( 'NONE', #46556, #26931, #5511, .T. ) ;
#49631 = ORIENTED_EDGE ( 'NONE', *, *, #12811, .F. ) ;
#49632 = CARTESIAN_POINT ( 'NONE',  ( 60.00000000000001421, -113.5000000000000142, -60.00000000000001421 ) ) ;
#49633 = DIRECTION ( 'NONE',  ( -0.000000000000000000, 1.000000000000000000, -0.000000000000000000 ) ) ;
#49634 = AXIS2_PLACEMENT_3D ( 'NONE', #45335, #37691, #1428 ) ;
#49635 = DIRECTION ( 'NONE',  ( -0.000000000000000000, 0.3546048870425463906, 0.9350162426854107256 ) ) ;
#49636 = ORIENTED_EDGE ( 'NONE', *, *, #37033, .T. ) ;
#49637 = CARTESIAN_POINT ( 'NONE',  ( -108.4791267515088435, -173.5000000000000284, -186.7953921478704729 ) ) ;
#49638 = DIRECTION ( 'NONE',  ( 0.000000000000000000, 0.000000000000000000, 1.000000000000000000 ) ) ;
#49639 = CONTEXT_DEPENDENT_SHAPE_REPRESENTATION ( #23315, #5018 ) ;
#49640 = CARTESIAN_POINT ( 'NONE',  ( 38.01517884164427130, -193.5000000000000000, -88.85232316304831102 ) ) ;
#49641 = CARTESIAN_POINT ( 'NONE',  ( -332.3517673607765914, -149.0257676989619142, 54.29949524055110999 ) ) ;
#49642 = EDGE_CURVE ( 'NONE', #38097, #30309, #4778, .T. ) ;
#49643 = ORIENTED_EDGE ( 'NONE', *, *, #10893, .T. ) ;
#49644 = PLANE ( 'NONE',  #33057 ) ;
#49645 = CARTESIAN_POINT ( 'NONE',  ( -49.29161362951452929, -193.5000000000000000, -0.5829794791144748967 ) ) ;
#49646 = EDGE_CURVE ( 'NONE', #22837, #22268, #15583, .T. ) ;
#49647 = CARTESIAN_POINT ( 'NONE',  ( -15.24927435600541692, -193.5000000000000000, 120.5021863277719234 ) ) ;
#49648 = ORIENTED_EDGE ( 'NONE', *, *, #11188, .T. ) ;
#49649 = EDGE_LOOP ( 'NONE', ( #51837, #2306, #23826, #34831 ) ) ;
#49650 = EDGE_CURVE ( 'NONE', #34248, #41454, #45761, .T. ) ;
#49651 = VECTOR ( 'NONE', #20838, 1000.000000000000000 ) ;
#49652 = PLANE ( 'NONE',  #15195 ) ;
#49653 = LINE ( 'NONE', #44927, #6010 ) ;
#49654 = ORIENTED_EDGE ( 'NONE', *, *, #12765, .T. ) ;
#49655 = CARTESIAN_POINT ( 'NONE',  ( -336.3521761649654422, -181.4155151828941825, -11.56382487286496463 ) ) ;
#49656 = EDGE_LOOP ( 'NONE', ( #9330, #18848, #35044, #19446 ) ) ;
#49657 = DIRECTION ( 'NONE',  ( 0.000000000000000000, 1.000000000000000000, 0.000000000000000000 ) ) ;
#49658 = CARTESIAN_POINT ( 'NONE',  ( -5.113431607746556473, -193.5000000000000000, 117.2365833888819537 ) ) ;
#49659 = LINE ( 'NONE', #20486, #1898 ) ;
#49660 = CARTESIAN_POINT ( 'NONE',  ( -336.3521761649654422, -118.0087234915157381, -58.76657425099333665 ) ) ;
#49661 = CARTESIAN_POINT ( 'NONE',  ( 0.000000000000000000, -71.25809448646026567, 27.41866715058169390 ) ) ;
#49662 = AXIS2_PLACEMENT_3D ( 'NONE', #18294, #41672, #37734 ) ;
#49663 = PLANE ( 'NONE',  #31886 ) ;
#49664 = VERTEX_POINT ( 'NONE', #16870 ) ;
#49665 = AXIS2_PLACEMENT_3D ( 'NONE', #17918, #6349, #2649 ) ;
#49666 = CARTESIAN_POINT ( 'NONE',  ( -46.00000000000000711, 20.00000000000000000, -4.999999999999988454 ) ) ;
#49667 = ORIENTED_EDGE ( 'NONE', *, *, #15006, .T. ) ;
#49668 = FACE_OUTER_BOUND ( 'NONE', #49272, .T. ) ;
#49669 = ORIENTED_EDGE ( 'NONE', *, *, #10754, .F. ) ;
#49670 = LINE ( 'NONE', #21030, #12503 ) ;
#49671 = ORIENTED_EDGE ( 'NONE', *, *, #2309, .T. ) ;
#49672 = CIRCLE ( 'NONE', #11911, 20.00000000000000000 ) ;
#49673 = DIRECTION ( 'NONE',  ( -0.1182731709213730997, 0.000000000000000000, 0.9929810960135161402 ) ) ;
#49674 = FACE_OUTER_BOUND ( 'NONE', #46268, .T. ) ;
#49675 = EDGE_LOOP ( 'NONE', ( #23277, #45547, #28873, #12473 ) ) ;
#49678 = EDGE_LOOP ( 'NONE', ( #19159, #22061, #20047, #13596 ) ) ;
#49677 = CARTESIAN_POINT ( 'NONE',  ( -332.3517673607765914, -93.75055682584159911, 51.01861988938794923 ) ) ;
#49676 = DIRECTION ( 'NONE',  ( 0.000000000000000000, 0.1205366802553338029, 0.9927088740980527515 ) ) ;
#49679 = VECTOR ( 'NONE', #24914, 1000.000000000000000 ) ;
#49680 = DIRECTION ( 'NONE',  ( 0.1768902751225802927, 0.000000000000000000, -0.9842305779475953864 ) ) ;
#49681 = ORIENTED_EDGE ( 'NONE', *, *, #43762, .F. ) ;
#49682 = LINE ( 'NONE', #40736, #34773 ) ;
#49683 = VERTEX_POINT ( 'NONE', #29454 ) ;
#49684 = ADVANCED_FACE ( 'NONE', ( #2394 ), #43098, .T. ) ;
#49685 = EDGE_CURVE ( 'NONE', #18737, #9440, #37368, .T. ) ;
#49686 = CARTESIAN_POINT ( 'NONE',  ( -54.99637373343399815, -193.5000000000000000, 123.8286356280830915 ) ) ;
#49689 = ORIENTED_EDGE ( 'NONE', *, *, #23057, .F. ) ;
#49688 = DIRECTION ( 'NONE',  ( 0.000000000000000000, 0.000000000000000000, 1.000000000000000000 ) ) ;
#49687 = CARTESIAN_POINT ( 'NONE',  ( -43.48323084606168720, -177.1207230881787780, 124.9001241957026167 ) ) ;
#49690 = ORIENTED_EDGE ( 'NONE', *, *, #35606, .F. ) ;
#49691 = CARTESIAN_POINT ( 'NONE',  ( -124.9871112439422092, -193.5000000000000000, -98.85104101073275729 ) ) ;
#49692 = DIRECTION ( 'NONE',  ( 0.000000000000000000, -0.000000000000000000, -1.000000000000000000 ) ) ;
#49693 = LINE ( 'NONE', #41528, #35750 ) ;
#49694 = EDGE_LOOP ( 'NONE', ( #16886, #19391, #14739, #28308 ) ) ;
#49695 = CARTESIAN_POINT ( 'NONE',  ( -336.3521761649654422, -176.5004679656469477, -25.97334715265976612 ) ) ;
#49696 = DIRECTION ( 'NONE',  ( -0.000000000000000000, -0.5680647467311510379, 0.8229838658936596829 ) ) ;
#49697 = EDGE_CURVE ( 'NONE', #41328, #28153, #34441, .T. ) ;
#49698 = FACE_OUTER_BOUND ( 'NONE', #30230, .T. ) ;
#49699 = CIRCLE ( 'NONE', #26152, 125.0000000000000000 ) ;
#49700 = PLANE ( 'NONE',  #522 ) ;
#49701 = ORIENTED_EDGE ( 'NONE', *, *, #22029, .F. ) ;
#49702 = EDGE_CURVE ( 'NONE', #32000, #9933, #42315, .T. ) ;
#49703 = AXIS2_PLACEMENT_3D ( 'NONE', #39224, #11868, #35523 ) ;
#49704 = CARTESIAN_POINT ( 'NONE',  ( 43.86477233319988756, -193.5000000000000000, -84.24728067915975771 ) ) ;
#49705 = DIRECTION ( 'NONE',  ( -1.000000000000000000, 0.000000000000000000, -0.000000000000000000 ) ) ;
#49706 = EDGE_CURVE ( 'NONE', #29948, #27304, #14735, .T. ) ;
#49707 = VECTOR ( 'NONE', #38333, 1000.000000000000114 ) ;
#49708 = CARTESIAN_POINT ( 'NONE',  ( 75.12566530717464275, -175.3837268820161057, 18.62405380494841367 ) ) ;
#49709 = ORIENTED_EDGE ( 'NONE', *, *, #25655, .F. ) ;
#49710 = ADVANCED_FACE ( 'NONE', ( #47056 ), #30245, .T. ) ;
#49711 = CARTESIAN_POINT ( 'NONE',  ( 141.7825277784304205, -213.5000000000000000, -9.999999999999987566 ) ) ;
#49712 = DIRECTION ( 'NONE',  ( 0.000000000000000000, -0.000000000000000000, 1.000000000000000000 ) ) ;
#49713 = EDGE_CURVE ( 'NONE', #21438, #36520, #38112, .T. ) ;
#49714 = CARTESIAN_POINT ( 'NONE',  ( -330.4913330509368166, -115.8919814278863356, 58.50955523165747252 ) ) ;
#49715 = PLANE ( 'NONE',  #4824 ) ;
#49716 = AXIS2_PLACEMENT_3D ( 'NONE', #36255, #48633, #35741 ) ;
#49717 = DIRECTION ( 'NONE',  ( -0.000000000000000000, 1.000000000000000000, -0.000000000000000000 ) ) ;
#49718 = VECTOR ( 'NONE', #26058, 1000.000000000000000 ) ;
#49719 = AXIS2_PLACEMENT_3D ( 'NONE', #336, #4042, #32143 ) ;
#49720 = DIRECTION ( 'NONE',  ( 0.000000000000000000, 0.000000000000000000, 1.000000000000000000 ) ) ;
#49721 = CARTESIAN_POINT ( 'NONE',  ( -47.48307690889363641, -193.5000000000000000, -0.08879589532292464504 ) ) ;
#49723 = ORIENTED_EDGE ( 'NONE', *, *, #12613, .F. ) ;
#49722 = DIRECTION ( 'NONE',  ( 0.000000000000000000, 1.000000000000000000, 0.000000000000000000 ) ) ;
#49724 = ORIENTED_EDGE ( 'NONE', *, *, #45542, .F. ) ;
#49725 = CARTESIAN_POINT ( 'NONE',  ( 1.150725574412418739, -193.5000000000000000, -114.7252272087845881 ) ) ;
#49726 = DIRECTION ( 'NONE',  ( 0.000000000000000000, 0.000000000000000000, 1.000000000000000000 ) ) ;
#49728 = ORIENTED_EDGE ( 'NONE', *, *, #48573, .F. ) ;
#49727 = DIRECTION ( 'NONE',  ( 0.000000000000000000, 0.000000000000000000, 1.000000000000000000 ) ) ;
#49729 = EDGE_CURVE ( 'NONE', #21286, #38437, #10027, .T. ) ;
#49730 = VERTEX_POINT ( 'NONE', #35208 ) ;
#49731 = ORIENTED_EDGE ( 'NONE', *, *, #41824, .F. ) ;
#49732 = DIRECTION ( 'NONE',  ( -0.000000000000000000, 1.000000000000000000, -0.000000000000000000 ) ) ;
#49733 = VECTOR ( 'NONE', #15961, 1000.000000000000000 ) ;
#49734 = LINE ( 'NONE', #37896, #45450 ) ;
#49735 = DIRECTION ( 'NONE',  ( -0.6068001458185945385, 0.000000000000000000, 0.7948544414133523750 ) ) ;
#49736 = ORIENTED_EDGE ( 'NONE', *, *, #33616, .F. ) ;
#49737 = AXIS2_PLACEMENT_3D ( 'NONE', #15264, #39927, #39668 ) ;
#49738 = EDGE_CURVE ( 'NONE', #17378, #16149, #34944, .T. ) ;
#49739 = CARTESIAN_POINT ( 'NONE',  ( -37.08895481556041318, -193.5000000000000000, 124.4799742258550310 ) ) ;
#49741 = VERTEX_POINT ( 'NONE', #26040 ) ;
#49740 = CARTESIAN_POINT ( 'NONE',  ( -155.4465502054561057, -183.6283474603465606, 64.67588669375881238 ) ) ;
#49742 = CARTESIAN_POINT ( 'NONE',  ( -48.64924157374596092, -189.7472609257535510, 124.9998842437354227 ) ) ;
#49743 = VERTEX_POINT ( 'NONE', #30493 ) ;
#49744 = CARTESIAN_POINT ( 'NONE',  ( -339.1964088526558498, -75.22798428563942252, 33.92731199008440512 ) ) ;
#49745 = ORIENTED_EDGE ( 'NONE', *, *, #38897, .F. ) ;
#49746 = ADVANCED_FACE ( 'NONE', ( #18677 ), #22358, .F. ) ;
#49747 = EDGE_CURVE ( 'NONE', #37538, #33858, #34186, .T. ) ;
#49748 = ADVANCED_FACE ( 'NONE', ( #46536 ), #6845, .F. ) ;
#49749 = EDGE_CURVE ( 'NONE', #138, #9404, #22624, .T. ) ;
#49750 = DIRECTION ( 'NONE',  ( -1.000000000000000000, 0.000000000000000000, 0.000000000000000000 ) ) ;
#49751 = CARTESIAN_POINT ( 'NONE',  ( -5.461633243180946451, -175.3837268820161057, 116.2991637277478247 ) ) ;
#49752 = CARTESIAN_POINT ( 'NONE',  ( -162.9896759831412965, -183.6283474603465606, -50.12318939043964861 ) ) ;
#49753 = AXIS2_PLACEMENT_3D ( 'NONE', #30440, #18381, #43055 ) ;
#49754 = VECTOR ( 'NONE', #18531, 1000.000000000000000 ) ;
#49755 = EDGE_CURVE ( 'NONE', #38638, #44868, #2184, .T. ) ;
#49756 = ORIENTED_EDGE ( 'NONE', *, *, #25671, .T. ) ;
#49757 = VECTOR ( 'NONE', #14605, 999.9999999999998863 ) ;
#49758 = EDGE_LOOP ( 'NONE', ( #6143, #25904, #47078, #4573 ) ) ;
#49759 = CARTESIAN_POINT ( 'NONE',  ( -89.73513343757491612, -177.1207230881787780, -117.9955164924467397 ) ) ;
#49760 = CARTESIAN_POINT ( 'NONE',  ( -30.00000000000000000, -43.50000000000000000, -30.00000000000000711 ) ) ;
#49761 = ORIENTED_EDGE ( 'NONE', *, *, #14190, .F. ) ;
#49762 = EDGE_CURVE ( 'NONE', #31150, #45018, #42065, .T. ) ;
#49763 = LINE ( 'NONE', #18470, #24155 ) ;
#49764 = VERTEX_POINT ( 'NONE', #14227 ) ;
#49765 = LINE ( 'NONE', #28983, #36810 ) ;
#49766 = ADVANCED_FACE ( 'NONE', ( #46290 ), #10271, .T. ) ;
#49767 = DIRECTION ( 'NONE',  ( 0.000000000000000000, -0.4647231720437573488, 0.8854560256532157947 ) ) ;
#49768 = EDGE_CURVE ( 'NONE', #10964, #51141, #26287, .T. ) ;
#49769 = VERTEX_POINT ( 'NONE', #35997 ) ;
#49770 = DIRECTION ( 'NONE',  ( 0.6528221181905280446, 0.000000000000000000, -0.7575112421616145841 ) ) ;
#49771 = ORIENTED_EDGE ( 'NONE', *, *, #51025, .F. ) ;
#49772 = DIRECTION ( 'NONE',  ( 0.000000000000000000, -1.000000000000000000, 0.000000000000000000 ) ) ;
#49773 = EDGE_CURVE ( 'NONE', #8523, #6100, #41601, .T. ) ;
#49774 = CARTESIAN_POINT ( 'NONE',  ( -14.28570516517293676, -193.5000000000000000, 120.2323164553486663 ) ) ;
#49775 = CARTESIAN_POINT ( 'NONE',  ( 47.04848625005566731, -183.6283474603465606, 80.61932246194658092 ) ) ;
#49776 = EDGE_LOOP ( 'NONE', ( #7067, #8070, #45309, #18138 ) ) ;
#49777 = CIRCLE ( 'NONE', #26265, 124.9999999999999858 ) ;
#49778 = EDGE_CURVE ( 'NONE', #33733, #602, #10547, .T. ) ;
#49779 = DIRECTION ( 'NONE',  ( 0.000000000000000000, 0.000000000000000000, -1.000000000000000000 ) ) ;
#49780 = CARTESIAN_POINT ( 'NONE',  ( -173.2765435274470178, -183.6283474603465606, -7.113702696401515979 ) ) ;
#49781 = LINE ( 'NONE', #33987, #51751 ) ;
#49782 = CARTESIAN_POINT ( 'NONE',  ( -166.2107720749849022, -175.3837268820161057, -38.92640747825594616 ) ) ;
#49783 = EDGE_CURVE ( 'NONE', #672, #16398, #19964, .T. ) ;
#49784 = VECTOR ( 'NONE', #18503, 1000.000000000000000 ) ;
#49785 = EDGE_LOOP ( 'NONE', ( #2590, #806, #43151, #45953 ) ) ;
#49786 = DIRECTION ( 'NONE',  ( 0.000000000000000000, -0.2393156642875448881, 0.9709418174260553425 ) ) ;
#49787 = ORIENTED_EDGE ( 'NONE', *, *, #11052, .T. ) ;
#49788 = DIRECTION ( 'NONE',  ( 0.000000000000000000, 1.410908427127803051E-14, 1.000000000000000000 ) ) ;
#49790 = ORIENTED_EDGE ( 'NONE', *, *, #30675, .F. ) ;
#49789 = CARTESIAN_POINT ( 'NONE',  ( -161.4019114581581391, -189.7472609257535510, 53.60452120946272458 ) ) ;
#49791 = EDGE_LOOP ( 'NONE', ( #100, #30774, #4290, #9978 ) ) ;
#49792 = CIRCLE ( 'NONE', #27103, 125.0000000000000000 ) ;
#49793 = VECTOR ( 'NONE', #30376, 1000.000000000000114 ) ;
#49794 = EDGE_CURVE ( 'NONE', #47080, #42377, #4454, .T. ) ;
#49795 = EDGE_CURVE ( 'NONE', #24853, #20197, #16030, .T. ) ;
#49796 = FACE_OUTER_BOUND ( 'NONE', #4931, .T. ) ;
#49797 = AXIS2_PLACEMENT_3D ( 'NONE', #40947, #20988, #41460 ) ;
#49798 = EDGE_LOOP ( 'NONE', ( #37334, #31899, #17592, #6996 ) ) ;
#49799 = CARTESIAN_POINT ( 'NONE',  ( -339.1964088526558498, -115.8919814278871598, -58.50955523165758621 ) ) ;
#49800 = ORIENTED_EDGE ( 'NONE', *, *, #7091, .F. ) ;
#49801 = DIRECTION ( 'NONE',  ( 0.000000000000000000, 0.000000000000000000, 1.000000000000000000 ) ) ;
#49802 = CARTESIAN_POINT ( 'NONE',  ( -336.3521761649653854, -136.2687678316390532, 58.62557946887775273 ) ) ;
#49803 = AXIS2_PLACEMENT_3D ( 'NONE', #8590, #35942, #12790 ) ;
#49804 = DIRECTION ( 'NONE',  ( 0.000000000000000000, 1.000000000000000000, 0.000000000000000000 ) ) ;
#49805 = FACE_OUTER_BOUND ( 'NONE', #9695, .T. ) ;
#49806 = ORIENTED_EDGE ( 'NONE', *, *, #30344, .T. ) ;
#49807 = VERTEX_POINT ( 'NONE', #15786 ) ;
#49808 = ORIENTED_EDGE ( 'NONE', *, *, #17319, .T. ) ;
#49809 = DIRECTION ( 'NONE',  ( -1.000000000000000000, 0.000000000000000000, 0.000000000000000000 ) ) ;
#49810 = CARTESIAN_POINT ( 'NONE',  ( -339.1964088526558498, -74.65991953890876687, -33.10432812419148263 ) ) ;
#49811 = DIRECTION ( 'NONE',  ( 0.000000000000000000, 0.000000000000000000, 1.000000000000000000 ) ) ;
#49812 = CARTESIAN_POINT ( 'NONE',  ( -170.0000000000000284, -130.6726371812771959, -60.00000000000000711 ) ) ;
#49813 = AXIS2_PLACEMENT_3D ( 'NONE', #37617, #9497, #33424 ) ;
#49814 = ORIENTED_EDGE ( 'NONE', *, *, #26326, .T. ) ;
#49815 = ADVANCED_FACE ( 'NONE', ( #8137 ), #35458, .F. ) ;
#49816 = EDGE_CURVE ( 'NONE', #46084, #16523, #36240, .T. ) ;
#49817 = VECTOR ( 'NONE', #37021, 1000.000000000000000 ) ;
#49818 = EDGE_CURVE ( 'NONE', #24385, #26442, #39911, .T. ) ;
#49819 = EDGE_CURVE ( 'NONE', #23438, #25658, #8038, .T. ) ;
#49820 = ORIENTED_EDGE ( 'NONE', *, *, #47159, .T. ) ;
#49822 = ORIENTED_EDGE ( 'NONE', *, *, #6453, .F. ) ;
#49821 = DIRECTION ( 'NONE',  ( 0.000000000000000000, 0.000000000000000000, -1.000000000000000000 ) ) ;
#49823 = ORIENTED_EDGE ( 'NONE', *, *, #8663, .T. ) ;
#49824 = LINE ( 'NONE', #18018, #39206 ) ;
#49825 = CARTESIAN_POINT ( 'NONE',  ( -332.3517673607765914, -100.1170788342122080, 54.23253582808833073 ) ) ;
#49826 = CARTESIAN_POINT ( 'NONE',  ( -48.47912675150885065, -183.6283474603465606, 6.938893903907228378E-15 ) ) ;
#49827 = CARTESIAN_POINT ( 'NONE',  ( -129.9529520667707629, -189.7472609257535510, -94.79987230211960991 ) ) ;
#49828 = ORIENTED_EDGE ( 'NONE', *, *, #25974, .T. ) ;
#49829 = CARTESIAN_POINT ( 'NONE',  ( 75.37518750349084939, -193.5000000000000000, 6.025661128238930964 ) ) ;
#49830 = AXIS2_PLACEMENT_3D ( 'NONE', #24789, #40803, #36880 ) ;
#49831 = ORIENTED_EDGE ( 'NONE', *, *, #46210, .T. ) ;
#49832 = ORIENTED_EDGE ( 'NONE', *, *, #39470, .F. ) ;
#49833 = CARTESIAN_POINT ( 'NONE',  ( -124.1938582159088327, -175.3837268820161057, -99.45993886622791536 ) ) ;
#49834 = VECTOR ( 'NONE', #13094, 1000.000000000000000 ) ;
#49835 = DIRECTION ( 'NONE',  ( 0.000000000000000000, 1.249000902703301108E-14, 1.000000000000000000 ) ) ;
#49836 = VERTEX_POINT ( 'NONE', #4199 ) ;
#49837 = DIRECTION ( 'NONE',  ( 0.000000000000000000, -6.129356281784718821E-14, -1.000000000000000000 ) ) ;
#49838 = DIRECTION ( 'NONE',  ( 1.043714542225393223E-14, -0.1205366802553164696, 0.9927088740980548609 ) ) ;
#49839 = DIRECTION ( 'NONE',  ( -0.6528221181905227155, 0.000000000000000000, 0.7575112421616191360 ) ) ;
#49840 = CARTESIAN_POINT ( 'NONE',  ( -332.3517673607765914, -100.7053649598255021, 55.50139289590170222 ) ) ;
#49841 = ADVANCED_FACE ( 'NONE', ( #15509 ), #43615, .F. ) ;
#49842 = DIRECTION ( 'NONE',  ( 0.000000000000000000, 0.000000000000000000, 1.000000000000000000 ) ) ;
#49843 = FACE_BOUND ( 'NONE', #4020, .T. ) ;
#49844 = ORIENTED_EDGE ( 'NONE', *, *, #11521, .F. ) ;
#49845 = LINE ( 'NONE', #1217, #49140 ) ;
#49846 = VERTEX_POINT ( 'NONE', #12327 ) ;
#49847 = AXIS2_PLACEMENT_3D ( 'NONE', #7614, #20878, #24421 ) ;
#49848 = EDGE_LOOP ( 'NONE', ( #19167, #37665, #44893, #5197 ) ) ;
#49849 = CARTESIAN_POINT ( 'NONE',  ( 9.518239912201957864, -193.5000000000000000, -110.7307791902283043 ) ) ;
#49850 = ORIENTED_EDGE ( 'NONE', *, *, #39475, .F. ) ;
#49851 = AXIS2_PLACEMENT_3D ( 'NONE', #30609, #23003, #30113 ) ;
#49852 = PLANE ( 'NONE',  #30172 ) ;
#49853 = PLANE ( 'NONE',  #20927 ) ;
#49855 = ORIENTED_EDGE ( 'NONE', *, *, #17090, .T. ) ;
#49854 = DIRECTION ( 'NONE',  ( 0.000000000000000000, 1.688464183284092344E-14, -1.000000000000000000 ) ) ;
#49857 = VECTOR ( 'NONE', #42868, 999.9999999999998863 ) ;
#49856 = LINE ( 'NONE', #13851, #13477 ) ;
#49858 = CARTESIAN_POINT ( 'NONE',  ( 69.99104047056319189, -189.7472609257535510, -39.87254040532513955 ) ) ;
#49859 = ORIENTED_EDGE ( 'NONE', *, *, #22086, .F. ) ;
#49860 = VERTEX_POINT ( 'NONE', #19691 ) ;
#49861 = ORIENTED_EDGE ( 'NONE', *, *, #933, .T. ) ;
#49862 = CARTESIAN_POINT ( 'NONE',  ( 60.90550954139435902, -175.3837268820161057, 60.49794494914085874 ) ) ;
#49863 = CARTESIAN_POINT ( 'NONE',  ( -339.1964088526558498, -89.57268800991514013, -48.27201571436026484 ) ) ;
#49864 = CARTESIAN_POINT ( 'NONE',  ( -15.48416040178638831, -193.5000000000000000, 119.5301634136915112 ) ) ;
#49865 = LINE ( 'NONE', #38549, #11878 ) ;
#49866 = DIRECTION ( 'NONE',  ( 1.000000000000000000, 8.151826190875911381E-17, 3.091579882402618064E-17 ) ) ;
#49867 = EDGE_LOOP ( 'NONE', ( #15934, #20348, #8770, #7482 ) ) ;
#49868 = ADVANCED_FACE ( 'NONE', ( #20471 ), #20219, .F. ) ;
#49869 = DIRECTION ( 'NONE',  ( 0.2635871660690581320, 0.000000000000000000, 0.9646355819083614058 ) ) ;
#49870 = EDGE_LOOP ( 'NONE', ( #50153, #4757, #1289, #29826 ) ) ;
#49872 = VERTEX_POINT ( 'NONE', #23395 ) ;
#49871 = FACE_OUTER_BOUND ( 'NONE', #19164, .T. ) ;
#49873 = ORIENTED_EDGE ( 'NONE', *, *, #8415, .T. ) ;
#49874 = ORIENTED_EDGE ( 'NONE', *, *, #47675, .T. ) ;
#49875 = DIRECTION ( 'NONE',  ( 1.000000000000000000, -0.000000000000000000, -0.000000000000000000 ) ) ;
#49876 = DIRECTION ( 'NONE',  ( 1.000000000000000000, -0.000000000000000000, -0.000000000000000000 ) ) ;
#49877 = AXIS2_PLACEMENT_3D ( 'NONE', #5346, #33182, #17697 ) ;
#49878 = ORIENTED_EDGE ( 'NONE', *, *, #27919, .T. ) ;
#49879 = AXIS2_PLACEMENT_3D ( 'NONE', #5239, #44651, #8899 ) ;
#49880 = CARTESIAN_POINT ( 'NONE',  ( -332.3517673607765914, -177.7994952405510389, -25.52576769896207409 ) ) ;
#49881 = DIRECTION ( 'NONE',  ( -0.000000000000000000, 1.000000000000000000, -0.000000000000000000 ) ) ;
#49882 = VERTEX_POINT ( 'NONE', #28356 ) ;
#49883 = LINE ( 'NONE', #9420, #25821 ) ;
#49884 = VERTEX_POINT ( 'NONE', #8395 ) ;
#49885 = AXIS2_PLACEMENT_3D ( 'NONE', #35028, #10858, #6411 ) ;
#49886 = ORIENTED_EDGE ( 'NONE', *, *, #4016, .T. ) ;
#49887 = CARTESIAN_POINT ( 'NONE',  ( -47.51449116960048968, -193.5000000000000000, 0.2635871660690785045 ) ) ;
#49888 = DIRECTION ( 'NONE',  ( 1.000000000000000000, -8.465038975556376573E-17, 2.086444717177636171E-17 ) ) ;
#49889 = EDGE_CURVE ( 'NONE', #37865, #22881, #492, .T. ) ;
#49890 = CARTESIAN_POINT ( 'NONE',  ( 75.12566530717464275, -175.3837268820161057, 18.62405380494841367 ) ) ;
#49891 =( NAMED_UNIT ( * ) SI_UNIT ( $, .STERADIAN. ) SOLID_ANGLE_UNIT ( ) );
#49892 = ORIENTED_EDGE ( 'NONE', *, *, #27305, .F. ) ;
#49893 = CARTESIAN_POINT ( 'NONE',  ( -118.4380981977755880, -193.5000000000000000, -102.3804074221059892 ) ) ;
#49894 = DIRECTION ( 'NONE',  ( 0.5085311186492094127, 0.000000000000000000, 0.8610436117673619938 ) ) ;
#49895 = LINE ( 'NONE', #49389, #19601 ) ;
#49896 = CARTESIAN_POINT ( 'NONE',  ( -168.8371699641976420, -193.5000000000000000, 33.74820638215509661 ) ) ;
#49897 = EDGE_LOOP ( 'NONE', ( #50681, #50544, #36029, #16850 ) ) ;
#49898 = CIRCLE ( 'NONE', #21343, 125.0000000000000000 ) ;
#49899 = DIRECTION ( 'NONE',  ( 0.000000000000000000, 0.000000000000000000, -1.000000000000000000 ) ) ;
#49900 = DIRECTION ( 'NONE',  ( 0.000000000000000000, -1.156482317317871232E-16, 1.000000000000000000 ) ) ;
#49901 = DIRECTION ( 'NONE',  ( -0.000000000000000000, 0.3546048870425331789, -0.9350162426854158326 ) ) ;
#49902 = ORIENTED_EDGE ( 'NONE', *, *, #1921, .T. ) ;
#49903 = EDGE_CURVE ( 'NONE', #210, #48594, #23892, .T. ) ;
#49904 = CARTESIAN_POINT ( 'NONE',  ( 76.52053249983504202, -177.1207230881787780, -0.2918682030015403162 ) ) ;
#49905 = FACE_BOUND ( 'NONE', #17052, .T. ) ;
#49906 = CARTESIAN_POINT ( 'NONE',  ( -332.3517673607765914, -127.9985676343858501, 58.88711093124869222 ) ) ;
#49907 = VERTEX_POINT ( 'NONE', #27321 ) ;
#49908 = LINE ( 'NONE', #37564, #23751 ) ;
#49909 = ADVANCED_FACE ( 'NONE', ( #39403 ), #31522, .T. ) ;
#49910 = EDGE_LOOP ( 'NONE', ( #1965, #51242, #30729, #11666 ) ) ;
#49911 = LINE ( 'NONE', #38067, #35156 ) ;
#49912 = EDGE_CURVE ( 'NONE', #4457, #32311, #45002, .T. ) ;
#49913 = CARTESIAN_POINT ( 'NONE',  ( -180.0000000000000568, -123.5000000000000284, -41.63467731922663972 ) ) ;
#49914 = DIRECTION ( 'NONE',  ( 5.399917434947259359E-17, 1.000000000000000000, -0.000000000000000000 ) ) ;
#49915 = AXIS2_PLACEMENT_3D ( 'NONE', #51054, #50781, #31304 ) ;
#49916 = AXIS2_PLACEMENT_3D ( 'NONE', #32031, #16026, #7862 ) ;
#49917 = DIRECTION ( 'NONE',  ( 1.000000000000000000, -0.000000000000000000, -0.000000000000000000 ) ) ;
#49918 = DIRECTION ( 'NONE',  ( 0.000000000000000000, -1.000000000000000000, 0.000000000000000000 ) ) ;
#49919 = ORIENTED_EDGE ( 'NONE', *, *, #46483, .F. ) ;
#49920 = AXIS2_PLACEMENT_3D ( 'NONE', #21791, #4525, #2340 ) ;
#49921 = DIRECTION ( 'NONE',  ( 0.000000000000000000, 0.000000000000000000, 1.000000000000000000 ) ) ;
#49922 = EDGE_CURVE ( 'NONE', #7465, #48929, #34069, .T. ) ;
#49923 = EDGE_LOOP ( 'NONE', ( #8325, #50812, #35920, #4653 ) ) ;
#49924 = CARTESIAN_POINT ( 'NONE',  ( -170.0000000000000284, -123.5000000000000284, 6.938893903907228378E-15 ) ) ;
#49925 = VERTEX_POINT ( 'NONE', #29654 ) ;
#49926 = VECTOR ( 'NONE', #41193, 1000.000000000000000 ) ;
#49927 = CARTESIAN_POINT ( 'NONE',  ( -142.9772358822569629, -193.5000000000000000, 81.82363577055969017 ) ) ;
#49928 = ORIENTED_EDGE ( 'NONE', *, *, #38827, .F. ) ;
#49929 = EDGE_CURVE ( 'NONE', #25876, #17256, #5507, .T. ) ;
#49930 = AXIS2_PLACEMENT_3D ( 'NONE', #41912, #35830, #35310 ) ;
#49931 = EDGE_CURVE ( 'NONE', #4823, #5747, #29393, .T. ) ;
#49932 = PRODUCT ( 'Angle Mounting Base', 'Angle Mounting Base', '', ( #24673 ) ) ;
#49933 = DIRECTION ( 'NONE',  ( 0.000000000000000000, 1.000000000000000000, -0.000000000000000000 ) ) ;
#49934 = ORIENTED_EDGE ( 'NONE', *, *, #38686, .T. ) ;
#49937 = ORIENTED_EDGE ( 'NONE', *, *, #32348, .T. ) ;
#49936 = CYLINDRICAL_SURFACE ( 'NONE', #15759, 124.9999999999999858 ) ;
#49935 = CARTESIAN_POINT ( 'NONE',  ( -1.446433552754633256, 50.76980153716073829, -21.20538461533670116 ) ) ;
#49938 = EDGE_CURVE ( 'NONE', #25927, #51078, #47512, .T. ) ;
#49939 = PLANE ( 'NONE',  #13882 ) ;
#49940 = ORIENTED_EDGE ( 'NONE', *, *, #42316, .F. ) ;
#49941 = DIRECTION ( 'NONE',  ( 0.000000000000000000, -1.000000000000000000, 0.000000000000000000 ) ) ;
#49942 = ORIENTED_EDGE ( 'NONE', *, *, #23614, .F. ) ;
#49943 = LINE ( 'NONE', #42564, #11622 ) ;
#49946 = ORIENTED_EDGE ( 'NONE', *, *, #44992, .T. ) ;
#49945 = CARTESIAN_POINT ( 'NONE',  ( -340.0000000000000568, -78.50000000000002842, 5.000000000000001776 ) ) ;
#49944 = CARTESIAN_POINT ( 'NONE',  ( -332.3517673607765914, -98.41210887299327226, -53.46519113769058151 ) ) ;
#49947 = EDGE_LOOP ( 'NONE', ( #23620, #29377, #22431, #24200 ) ) ;
#49948 = DIRECTION ( 'NONE',  ( 0.02963332782256331357, 0.000000000000000000, -0.9995608365087942371 ) ) ;
#49949 = ORIENTED_EDGE ( 'NONE', *, *, #13884, .F. ) ;
#49950 = DIRECTION ( 'NONE',  ( 0.000000000000000000, 0.2393156642875547968, -0.9709418174260527890 ) ) ;
#49951 = AXIS2_PLACEMENT_3D ( 'NONE', #5761, #6529, #10445 ) ;
#49952 = CARTESIAN_POINT ( 'NONE',  ( 74.03660210627323579, -193.5000000000000000, -19.12855698118387693 ) ) ;
#49953 = ORIENTED_EDGE ( 'NONE', *, *, #5803, .F. ) ;
#49954 = EDGE_CURVE ( 'NONE', #46176, #30683, #40687, .T. ) ;
#49955 = DIRECTION ( 'NONE',  ( -0.000000000000000000, 1.000000000000000000, 0.000000000000000000 ) ) ;
#49956 = FILL_AREA_STYLE ('',( #41274 ) ) ;
#49957 = DIRECTION ( 'NONE',  ( 0.000000000000000000, -0.9927088740980538617, 0.1205366802553232974 ) ) ;
#49958 = VECTOR ( 'NONE', #27296, 1000.000000000000227 ) ;
#49959 = CYLINDRICAL_SURFACE ( 'NONE', #16491, 124.9999999999999858 ) ;
#49960 = AXIS2_PLACEMENT_3D ( 'NONE', #46100, #30300, #6405 ) ;
#49961 = ORIENTED_EDGE ( 'NONE', *, *, #24072, .T. ) ;
#49963 = EDGE_CURVE ( 'NONE', #46969, #16966, #9186, .T. ) ;
#49962 = CARTESIAN_POINT ( 'NONE',  ( -213.8817838414232426, -213.5000000000000000, 2.819679052520814125E-14 ) ) ;
#49965 = AXIS2_PLACEMENT_3D ( 'NONE', #36843, #1803, #834 ) ;
#49964 = CARTESIAN_POINT ( 'NONE',  ( -336.3521761649654422, -77.59233547837267508, 37.15394033962009246 ) ) ;
#49966 = CARTESIAN_POINT ( 'NONE',  ( -180.0000000000000568, -123.5000000000000284, -41.63467731922663972 ) ) ;
#49967 = ORIENTED_EDGE ( 'NONE', *, *, #25012, .T. ) ;
#49968 = DIRECTION ( 'NONE',  ( 0.000000000000000000, 1.000000000000000000, 0.000000000000000000 ) ) ;
#49969 = FACE_OUTER_BOUND ( 'NONE', #36900, .T. ) ;
#49970 = AXIS2_PLACEMENT_3D ( 'NONE', #19109, #35126, #30398 ) ;
#49971 = VECTOR ( 'NONE', #34769, 1000.000000000000000 ) ;
#49972 = DIRECTION ( 'NONE',  ( 0.000000000000000000, 0.000000000000000000, -1.000000000000000000 ) ) ;
#49973 = CARTESIAN_POINT ( 'NONE',  ( -135.6699833737243921, -189.7472609257535510, 89.56983042009322560 ) ) ;
#49974 = AXIS2_PLACEMENT_3D ( 'NONE', #36533, #33401, #9219 ) ;
#49975 = CARTESIAN_POINT ( 'NONE',  ( 16.00000000000000000, 20.00000000000000355, 0.000000000000000000 ) ) ;
#49976 = ADVANCED_FACE ( 'NONE', ( #13381 ), #9693, .T. ) ;
#49977 = VECTOR ( 'NONE', #20505, 1000.000000000000114 ) ;
#49978 = DIRECTION ( 'NONE',  ( 0.000000000000000000, -1.000000000000000000, 0.000000000000000000 ) ) ;
#49979 = CARTESIAN_POINT ( 'NONE',  ( -173.4190745413846457, -193.5000000000000000, -3.874202661594927211 ) ) ;
#49981 = ORIENTED_EDGE ( 'NONE', *, *, #22092, .T. ) ;
#49980 = CARTESIAN_POINT ( 'NONE',  ( -339.1964088526558498, -171.7720157143598669, 33.92731199008546383 ) ) ;
#49982 = VERTEX_POINT ( 'NONE', #772 ) ;
#49983 = EDGE_CURVE ( 'NONE', #45638, #48223, #4988, .T. ) ;
#49984 = EDGE_CURVE ( 'NONE', #47736, #30910, #32566, .T. ) ;
#49985 = CARTESIAN_POINT ( 'NONE',  ( 46.00000000000000711, -43.50000000000000000, -50.00000000000000000 ) ) ;
#49987 = ORIENTED_EDGE ( 'NONE', *, *, #31788, .F. ) ;
#49986 = LINE ( 'NONE', #41837, #49718 ) ;
#49988 = ORIENTED_EDGE ( 'NONE', *, *, #42378, .T. ) ;
#49989 = VECTOR ( 'NONE', #51564, 1000.000000000000227 ) ;
#49990 = ORIENTED_EDGE ( 'NONE', *, *, #19201, .T. ) ;
#49991 = CARTESIAN_POINT ( 'NONE',  ( -77.03256798524175508, -189.7472609257535510, 121.6951149130964893 ) ) ;
#49992 = AXIS2_PLACEMENT_3D ( 'NONE', #47938, #40284, #3781 ) ;
#49993 = AXIS2_PLACEMENT_3D ( 'NONE', #20279, #48932, #3728 ) ;
#49994 = EDGE_CURVE ( 'NONE', #16360, #51365, #5247, .T. ) ;
#49995 = CARTESIAN_POINT ( 'NONE',  ( -330.4913330509368166, -138.1050951016791544, -57.16590939599326049 ) ) ;
#49996 = LINE ( 'NONE', #26066, #48127 ) ;
#49997 = ORIENTED_EDGE ( 'NONE', *, *, #49938, .T. ) ;
#49998 = EDGE_CURVE ( 'NONE', #14667, #32936, #28611, .T. ) ;
#49999 = PLANE ( 'NONE',  #46136 ) ;
#50000 = CARTESIAN_POINT ( 'NONE',  ( 39.18328161278951427, -193.5000000000000000, 89.10837311819236106 ) ) ;
#50002 = VERTEX_POINT ( 'NONE', #49128 ) ;
#50001 = CARTESIAN_POINT ( 'NONE',  ( -49.46816693883101124, -193.5000000000000000, -0.1476465640024848536 ) ) ;
#50003 = ADVANCED_FACE ( 'NONE', ( #48617 ), #21527, .F. ) ;
#50004 = AXIS2_PLACEMENT_3D ( 'NONE', #12373, #36543, #24218 ) ;
#50005 = VECTOR ( 'NONE', #36705, 1000.000000000000114 ) ;
#50006 = DIRECTION ( 'NONE',  ( 0.8896570909947436601, 0.000000000000000000, 0.4566292373937200777 ) ) ;
#50007 = ORIENTED_EDGE ( 'NONE', *, *, #4594, .F. ) ;
#50008 = DIRECTION ( 'NONE',  ( 0.000000000000000000, -0.000000000000000000, 1.000000000000000000 ) ) ;
#50009 = ADVANCED_FACE ( 'NONE', ( #37287 ), #44658, .T. ) ;
#50010 = VERTEX_POINT ( 'NONE', #12846 ) ;
#50011 = DIRECTION ( 'NONE',  ( -0.000000000000000000, 1.000000000000000000, -0.000000000000000000 ) ) ;
#50012 = VECTOR ( 'NONE', #31841, 1000.000000000000227 ) ;
#50013 = DIRECTION ( 'NONE',  ( 0.000000000000000000, 0.000000000000000000, 1.000000000000000000 ) ) ;
#50014 = DIRECTION ( 'NONE',  ( 0.05924062789370006937, 0.000000000000000000, 0.9982437317643222396 ) ) ;
#50015 = VECTOR ( 'NONE', #27689, 1000.000000000000000 ) ;
#50016 = EDGE_LOOP ( 'NONE', ( #28958, #22849, #19244, #23631 ) ) ;
#50017 = ORIENTED_EDGE ( 'NONE', *, *, #15882, .T. ) ;
#50018 = DIRECTION ( 'NONE',  ( 0.000000000000000000, 0.000000000000000000, 1.000000000000000000 ) ) ;
#50019 = CARTESIAN_POINT ( 'NONE',  ( -336.3521761649654422, -123.5000000000000284, 0.000000000000000000 ) ) ;
#50020 = VERTEX_POINT ( 'NONE', #1279 ) ;
#50021 = DIRECTION ( 'NONE',  ( 0.000000000000000000, 0.000000000000000000, -1.000000000000000000 ) ) ;
#50022 = EDGE_LOOP ( 'NONE', ( #11009, #21632, #13891, #30530 ) ) ;
#50023 = FACE_BOUND ( 'NONE', #44971, .T. ) ;
#50024 = LINE ( 'NONE', #41597, #3748 ) ;
#50025 = VERTEX_POINT ( 'NONE', #28870 ) ;
#50026 = CARTESIAN_POINT ( 'NONE',  ( -48.47912675150885065, -193.5000000000000000, 125.0000000000000000 ) ) ;
#50027 = ORIENTED_EDGE ( 'NONE', *, *, #19576, .F. ) ;
#50028 = AXIS2_PLACEMENT_3D ( 'NONE', #6542, #25979, #18364 ) ;
#50029 = DIRECTION ( 'NONE',  ( -0.000000000000000000, 1.000000000000000000, -0.000000000000000000 ) ) ;
#50030 = DIRECTION ( 'NONE',  ( -0.000000000000000000, 1.000000000000000000, -0.000000000000000000 ) ) ;
#50031 = EDGE_LOOP ( 'NONE', ( #51942, #37785, #11585, #46873 ) ) ;
#50032 = VECTOR ( 'NONE', #28601, 999.9999999999998863 ) ;
#50033 = AXIS2_PLACEMENT_3D ( 'NONE', #42643, #47109, #27375 ) ;
#50034 = LINE ( 'NONE', #10337, #1715 ) ;
#50035 = DIRECTION ( 'NONE',  ( 1.000000000000000000, -0.000000000000000000, -0.000000000000000000 ) ) ;
#50036 = DIRECTION ( 'NONE',  ( -0.8124868780056825335, 0.000000000000000000, 0.5829794791144703447 ) ) ;
#50037 = FACE_OUTER_BOUND ( 'NONE', #29340, .T. ) ;
#50038 = VERTEX_POINT ( 'NONE', #13114 ) ;
#50039 = DIRECTION ( 'NONE',  ( -0.4031234292879665171, 0.000000000000000000, -0.9151456172430210145 ) ) ;
#50040 = ORIENTED_EDGE ( 'NONE', *, *, #43287, .F. ) ;
#50041 = AXIS2_PLACEMENT_3D ( 'NONE', #25126, #45871, #37195 ) ;
#50042 = EDGE_CURVE ( 'NONE', #51627, #36158, #9438, .T. ) ;
#50043 = CARTESIAN_POINT ( 'NONE',  ( 72.31641062551800303, -175.3837268820161057, 32.14713283941989630 ) ) ;
#50045 = EDGE_LOOP ( 'NONE', ( #27839, #10411, #31360, #13200 ) ) ;
#50044 = CARTESIAN_POINT ( 'NONE',  ( -52.47502265695601409, -177.1207230881787780, -123.9361149384469485 ) ) ;
#50046 = VECTOR ( 'NONE', #6151, 1000.000000000000000 ) ;
#50047 = ADVANCED_FACE ( 'NONE', ( #8908 ), #21004, .F. ) ;
#50048 = ORIENTED_EDGE ( 'NONE', *, *, #33614, .F. ) ;
#50049 = EDGE_CURVE ( 'NONE', #42459, #29743, #31545, .T. ) ;
#50050 = EDGE_CURVE ( 'NONE', #6177, #50890, #29864, .T. ) ;
#50051 = VECTOR ( 'NONE', #2013, 1000.000000000000000 ) ;
#50052 = EDGE_CURVE ( 'NONE', #12141, #21231, #20639, .T. ) ;
#50053 = VECTOR ( 'NONE', #50588, 1000.000000000000000 ) ;
#50054 = PLANE ( 'NONE',  #18746 ) ;
#50055 = ORIENTED_EDGE ( 'NONE', *, *, #38474, .F. ) ;
#50056 = CARTESIAN_POINT ( 'NONE',  ( 76.51419089073348800, -193.5000000000000000, -1.292495564988658030 ) ) ;
#50057 = EDGE_CURVE ( 'NONE', #27843, #32868, #17840, .T. ) ;
#50058 = ORIENTED_EDGE ( 'NONE', *, *, #30137, .F. ) ;
#50059 = DIRECTION ( 'NONE',  ( -1.000000000000000000, 0.000000000000000000, 0.000000000000000000 ) ) ;
#50060 = PLANE ( 'NONE',  #12383 ) ;
#50061 = ADVANCED_FACE ( 'NONE', ( #42254 ), #22034, .T. ) ;
#50062 = LINE ( 'NONE', #33511, #16033 ) ;
#50063 = CARTESIAN_POINT ( 'NONE',  ( -339.1964088526558498, -102.6919536717982737, -56.27632902032089390 ) ) ;
#50064 = ORIENTED_EDGE ( 'NONE', *, *, #42711, .F. ) ;
#50065 = VERTEX_POINT ( 'NONE', #26484 ) ;
#50066 = ADVANCED_FACE ( 'NONE', ( #50675 ), #6791, .T. ) ;
#50067 = ORIENTED_EDGE ( 'NONE', *, *, #12765, .F. ) ;
#50068 = CARTESIAN_POINT ( 'NONE',  ( -48.47912675150885065, -183.6283474603465606, 6.938893903907228378E-15 ) ) ;
#50069 = CYLINDRICAL_SURFACE ( 'NONE', #5901, 4.999999999999997335 ) ;
#50070 = VECTOR ( 'NONE', #31977, 1000.000000000000227 ) ;
#50071 = VECTOR ( 'NONE', #2827, 1000.000000000000114 ) ;
#50072 = EDGE_CURVE ( 'NONE', #15026, #20985, #14670, .T. ) ;
#50073 = DIRECTION ( 'NONE',  ( -0.9993908270190956511, 4.273955692857142571E-18, -0.03489949670250096919 ) ) ;
#50074 = PLANE ( 'NONE',  #2054 ) ;
#50075 = ORIENTED_EDGE ( 'NONE', *, *, #24061, .F. ) ;
#50076 = VECTOR ( 'NONE', #34093, 1000.000000000000000 ) ;
#50077 = ADVANCED_FACE ( 'NONE', ( #23073 ), #14169, .F. ) ;
#50078 = ADVANCED_FACE ( 'NONE', ( #1799 ), #30681, .T. ) ;
#50079 = ORIENTED_EDGE ( 'NONE', *, *, #24481, .F. ) ;
#50081 = EDGE_LOOP ( 'NONE', ( #17223, #31904, #45481, #28172 ) ) ;
#50080 = CARTESIAN_POINT ( 'NONE',  ( 75.12566530717464275, -189.7472609257535510, 18.62405380494842433 ) ) ;
#50082 = AXIS2_PLACEMENT_3D ( 'NONE', #20075, #24533, #44258 ) ;
#50083 = DIRECTION ( 'NONE',  ( 0.000000000000000000, 0.000000000000000000, 1.000000000000000000 ) ) ;
#50084 = VECTOR ( 'NONE', #47966, 1000.000000000000000 ) ;
#50085 = FACE_OUTER_BOUND ( 'NONE', #42880, .T. ) ;
#50086 = CIRCLE ( 'NONE', #4754, 125.0000000000000000 ) ;
#50087 = VECTOR ( 'NONE', #7036, 1000.000000000000000 ) ;
#50088 = CARTESIAN_POINT ( 'NONE',  ( 75.95066919219054569, -193.5000000000000000, -11.92584929509534852 ) ) ;
#50089 = PLANE ( 'NONE',  #31011 ) ;
#50090 = ORIENTED_EDGE ( 'NONE', *, *, #33005, .F. ) ;
#50091 = CARTESIAN_POINT ( 'NONE',  ( -339.1964088526558498, -74.65991953890826949, 33.10432812419072945 ) ) ;
#50092 = AXIS2_PLACEMENT_3D ( 'NONE', #39809, #40326, #43767 ) ;
#50093 = EDGE_LOOP ( 'NONE', ( #48231, #31168, #24431, #36612 ) ) ;
#50094 = EDGE_CURVE ( 'NONE', #10964, #37735, #38581, .T. ) ;
#50095 = VECTOR ( 'NONE', #12167, 1000.000000000000000 ) ;
#50096 = ORIENTED_EDGE ( 'NONE', *, *, #14101, .F. ) ;
#50097 = CARTESIAN_POINT ( 'NONE',  ( -55.71438232577009586, -193.5000000000000000, -124.7904286264580804 ) ) ;
#50098 = LINE ( 'NONE', #30887, #43756 ) ;
#50099 = VERTEX_POINT ( 'NONE', #10203 ) ;
#50100 = DIRECTION ( 'NONE',  ( 0.000000000000000000, -0.000000000000000000, -1.000000000000000000 ) ) ;
#50101 = FACE_BOUND ( 'NONE', #37654, .T. ) ;
#50102 = CARTESIAN_POINT ( 'NONE',  ( 46.00000000000000711, -43.50000000000000000, -50.00000000000000000 ) ) ;
#50103 = LINE ( 'NONE', #21969, #36617 ) ;
#50104 = CARTESIAN_POINT ( 'NONE',  ( -339.1964088526558498, -108.8949048983204051, 57.16590939599314680 ) ) ;
#50105 = ADVANCED_FACE ( 'NONE', ( #2581 ), #14419, .T. ) ;
#50106 = EDGE_LOOP ( 'NONE', ( #34094, #51968, #20187, #26917 ) ) ;
#50107 = CIRCLE ( 'NONE', #27420, 125.0000000000000000 ) ;
#50108 = AXIS2_PLACEMENT_3D ( 'NONE', #20606, #36643, #16159 ) ;
#50109 = CARTESIAN_POINT ( 'NONE',  ( -168.1141659785444915, -177.1207230881787780, -36.22785377503943494 ) ) ;
#50110 = VERTEX_POINT ( 'NONE', #18613 ) ;
#50111 = AXIS2_PLACEMENT_3D ( 'NONE', #4114, #20129, #15945 ) ;
#50112 = EDGE_CURVE ( 'NONE', #9854, #26482, #6271, .T. ) ;
#50113 = EDGE_LOOP ( 'NONE', ( #29446, #24043, #43570, #13807 ) ) ;
#50114 = ADVANCED_FACE ( 'NONE', ( #50944 ), #34630, .T. ) ;
#50115 = LINE ( 'NONE', #17542, #43928 ) ;
#50116 = ORIENTED_EDGE ( 'NONE', *, *, #45011, .T. ) ;
#50117 = EDGE_CURVE ( 'NONE', #49394, #48961, #38317, .T. ) ;
#50118 = DIRECTION ( 'NONE',  ( 0.9266896074318343723, 0.000000000000000000, -0.3758275821142357809 ) ) ;
#50119 = AXIS2_PLACEMENT_3D ( 'NONE', #36400, #396, #16450 ) ;
#50120 = DIRECTION ( 'NONE',  ( 1.000000000000000000, 0.000000000000000000, 0.000000000000000000 ) ) ;
#50121 = AXIS2_PLACEMENT_3D ( 'NONE', #52039, #16025, #3507 ) ;
#50123 = ORIENTED_EDGE ( 'NONE', *, *, #24688, .T. ) ;
#50122 = LINE ( 'NONE', #26706, #22099 ) ;
#50124 = DIRECTION ( 'NONE',  ( 0.000000000000000000, 0.000000000000000000, 1.000000000000000000 ) ) ;
#50125 = VECTOR ( 'NONE', #4294, 1000.000000000000000 ) ;
#50126 = CIRCLE ( 'NONE', #27442, 125.0000000000000000 ) ;
#50127 = CIRCLE ( 'NONE', #37553, 125.0000000000000000 ) ;
#50128 = LINE ( 'NONE', #37756, #30248 ) ;
#50129 = CARTESIAN_POINT ( 'NONE',  ( -339.1964088526558498, -101.7569374291119857, 55.92172413327800484 ) ) ;
#50130 = ORIENTED_EDGE ( 'NONE', *, *, #1230, .T. ) ;
#50131 = ORIENTED_EDGE ( 'NONE', *, *, #41907, .T. ) ;
#50132 = ORIENTED_EDGE ( 'NONE', *, *, #4710, .F. ) ;
#50133 = CIRCLE ( 'NONE', #9835, 125.0000000000000000 ) ;
#50134 = CARTESIAN_POINT ( 'NONE',  ( -332.3517673607765914, -141.9604555052315220, 56.09938080879057765 ) ) ;
#50135 = DIRECTION ( 'NONE',  ( -0.9266896074318370369, 0.000000000000000000, 0.3758275821142292306 ) ) ;
#50136 = EDGE_CURVE ( 'NONE', #41636, #8157, #42519, .T. ) ;
#50137 = DIRECTION ( 'NONE',  ( 0.000000000000000000, 0.000000000000000000, 1.000000000000000000 ) ) ;
#50138 = FACE_OUTER_BOUND ( 'NONE', #49456, .T. ) ;
#50139 = CARTESIAN_POINT ( 'NONE',  ( 49.10711742958949344, -189.7472609257535510, 78.11481899503480975 ) ) ;
#50140 = EDGE_LOOP ( 'NONE', ( #42043, #1123, #49874, #41148 ) ) ;
#50141 = ADVANCED_FACE ( 'NONE', ( #14946 ), #30952, .F. ) ;
#50142 = EDGE_CURVE ( 'NONE', #30515, #46184, #9768, .T. ) ;
#50143 = CARTESIAN_POINT ( 'NONE',  ( -48.47912675150885065, -121.5000000000000142, 6.938893903907228378E-15 ) ) ;
#50144 = ORIENTED_EDGE ( 'NONE', *, *, #13746, .F. ) ;
#50146 = VERTEX_POINT ( 'NONE', #46474 ) ;
#50145 = DIRECTION ( 'NONE',  ( 0.000000000000000000, -0.1205366802553303196, -0.9927088740980530845 ) ) ;
#50147 = VECTOR ( 'NONE', #50398, 1000.000000000000000 ) ;
#50148 = ORIENTED_EDGE ( 'NONE', *, *, #1573, .T. ) ;
#50149 = VECTOR ( 'NONE', #22880, 999.9999999999998863 ) ;
#50150 = LINE ( 'NONE', #12624, #39975 ) ;
#50151 = VERTEX_POINT ( 'NONE', #28029 ) ;
#50152 = FACE_OUTER_BOUND ( 'NONE', #21093, .T. ) ;
#50153 = ORIENTED_EDGE ( 'NONE', *, *, #2157, .T. ) ;
#50154 = AXIS2_PLACEMENT_3D ( 'NONE', #14435, #42536, #6558 ) ;
#50155 = CARTESIAN_POINT ( 'NONE',  ( 26.70958190211001337, -175.3837268820161057, -99.85818990449013199 ) ) ;
#50156 = CARTESIAN_POINT ( 'NONE',  ( -336.3521761649654422, -159.7173995167596559, -47.83617848703447351 ) ) ;
#50157 = VERTEX_POINT ( 'NONE', #35400 ) ;
#50158 = DIRECTION ( 'NONE',  ( 0.000000000000000000, 0.000000000000000000, 1.000000000000000000 ) ) ;
#50159 = ORIENTED_EDGE ( 'NONE', *, *, #21164, .T. ) ;
#50160 = ORIENTED_EDGE ( 'NONE', *, *, #44431, .T. ) ;
#50161 = LINE ( 'NONE', #46215, #38791 ) ;
#50162 = VECTOR ( 'NONE', #34287, 1000.000000000000000 ) ;
#50163 = DIRECTION ( 'NONE',  ( 0.000000000000000000, 0.000000000000000000, 1.000000000000000000 ) ) ;
#50164 = AXIS2_PLACEMENT_3D ( 'NONE', #37902, #26070, #9531 ) ;
#50165 = CARTESIAN_POINT ( 'NONE',  ( -339.1964088526558498, -182.5000000000000568, 0.5000000000000457412 ) ) ;
#50166 = CARTESIAN_POINT ( 'NONE',  ( -170.8336150310145172, -189.7472609257535510, 25.58083653558488280 ) ) ;
#50167 = EDGE_LOOP ( 'NONE', ( #51974, #19306, #15653, #15753 ) ) ;
#50168 = CIRCLE ( 'NONE', #28302, 125.0000000000000000 ) ;
#50169 = FACE_OUTER_BOUND ( 'NONE', #13177, .T. ) ;
#50170 = DIRECTION ( 'NONE',  ( 1.000000000000000000, 0.000000000000000000, 0.000000000000000000 ) ) ;
#50171 = LINE ( 'NONE', #49640, #7853 ) ;
#50172 = LINE ( 'NONE', #9959, #5236 ) ;
#50173 = VERTEX_POINT ( 'NONE', #43296 ) ;
#50174 = CARTESIAN_POINT ( 'NONE',  ( -330.4913330509368166, -89.57268800991444380, 48.27201571435978877 ) ) ;
#50175 = DIRECTION ( 'NONE',  ( 0.000000000000000000, 0.000000000000000000, 1.000000000000000000 ) ) ;
#50176 = VECTOR ( 'NONE', #31041, 1000.000000000000000 ) ;
#50177 = DIRECTION ( 'NONE',  ( -0.000000000000000000, 1.000000000000000000, 0.000000000000000000 ) ) ;
#50178 = VERTEX_POINT ( 'NONE', #43806 ) ;
#50179 = CARTESIAN_POINT ( 'NONE',  ( -171.1451123608488274, -193.5000000000000000, 18.13990644964089682 ) ) ;
#50180 = CARTESIAN_POINT ( 'NONE',  ( -48.47912675150885065, -189.7472609257535510, 6.938893903907228378E-15 ) ) ;
#50181 = ORIENTED_EDGE ( 'NONE', *, *, #41552, .F. ) ;
#50182 = ADVANCED_FACE ( 'NONE', ( #19900 ), #7304, .F. ) ;
#50183 = EDGE_CURVE ( 'NONE', #16275, #16384, #35663, .T. ) ;
#50184 = EDGE_LOOP ( 'NONE', ( #50218, #36721, #39347, #19942 ) ) ;
#50185 = ORIENTED_EDGE ( 'NONE', *, *, #31239, .T. ) ;
#50186 =( REPRESENTATION_RELATIONSHIP ('NONE','NONE', #4578, #11639 ) REPRESENTATION_RELATIONSHIP_WITH_TRANSFORMATION ( #18092 )SHAPE_REPRESENTATION_RELATIONSHIP( ) );
#50187 = AXIS2_PLACEMENT_3D ( 'NONE', #10901, #26920, #46393 ) ;
#50188 = FACE_OUTER_BOUND ( 'NONE', #40835, .T. ) ;
#50189 = AXIS2_PLACEMENT_3D ( 'NONE', #47558, #23619, #19175 ) ;
#50190 = PLANE ( 'NONE',  #33749 ) ;
#50191 = CARTESIAN_POINT ( 'NONE',  ( -32.98951909085346301, -189.7472609257535510, 123.0287672223653033 ) ) ;
#50192 = VECTOR ( 'NONE', #1440, 1000.000000000000000 ) ;
#50193 = CARTESIAN_POINT ( 'NONE',  ( -171.9838957966129556, -189.7472609257535510, 19.27620354518722579 ) ) ;
#50194 = CARTESIAN_POINT ( 'NONE',  ( -112.1919339979530150, -175.3837268820161057, 107.5438431188761825 ) ) ;
#50195 = ORIENTED_EDGE ( 'NONE', *, *, #20205, .T. ) ;
#50196 = DIRECTION ( 'NONE',  ( 0.000000000000000000, 0.000000000000000000, -1.000000000000000000 ) ) ;
#50197 = VERTEX_POINT ( 'NONE', #8337 ) ;
#50198 = CARTESIAN_POINT ( 'NONE',  ( -116.2964108826154330, -183.6283474603465606, -105.0038855142073260 ) ) ;
#50199 = CIRCLE ( 'NONE', #42597, 125.0000000000000000 ) ;
#50200 = ORIENTED_EDGE ( 'NONE', *, *, #39133, .T. ) ;
#50201 = ADVANCED_FACE ( 'NONE', ( #19638 ), #51985, .T. ) ;
#50202 = LINE ( 'NONE', #42279, #28429 ) ;
#50203 = EDGE_CURVE ( 'NONE', #14153, #27547, #41639, .T. ) ;
#50204 = DIRECTION ( 'NONE',  ( 0.000000000000000000, 0.000000000000000000, 1.000000000000000000 ) ) ;
#50205 = CARTESIAN_POINT ( 'NONE',  ( -40.90423906728908321, -175.3837268820161057, -124.7702732086912221 ) ) ;
#50206 = EDGE_LOOP ( 'NONE', ( #36411, #50238, #19083, #18808 ) ) ;
#50209 = VERTEX_POINT ( 'NONE', #12261 ) ;
#50208 = LINE ( 'NONE', #13670, #33970 ) ;
#50207 = CARTESIAN_POINT ( 'NONE',  ( -1.160780020586678285, 50.70363469020618652, -21.26620207273386498 ) ) ;
#50210 = CARTESIAN_POINT ( 'NONE',  ( -339.1964088526558498, -173.1613497474970700, -33.67120938215281001 ) ) ;
#50211 = VERTEX_POINT ( 'NONE', #23340 ) ;
#50212 = DIRECTION ( 'NONE',  ( -0.000000000000000000, -1.000000000000000000, -0.000000000000000000 ) ) ;
#50213 = ORIENTED_EDGE ( 'NONE', *, *, #42687, .T. ) ;
#50214 = CARTESIAN_POINT ( 'NONE',  ( -48.47912675150885065, -175.3837268820161057, 6.938893903907228378E-15 ) ) ;
#50217 = ORIENTED_EDGE ( 'NONE', *, *, #28112, .F. ) ;
#50216 = CARTESIAN_POINT ( 'NONE',  ( -339.1964088526558498, -79.66942718702493664, 39.49849221029193558 ) ) ;
#50215 = DIRECTION ( 'NONE',  ( 0.9473263538541923934, 0.000000000000000000, -0.3202698538628350744 ) ) ;
#50218 = ORIENTED_EDGE ( 'NONE', *, *, #37934, .T. ) ;
#50219 = CARTESIAN_POINT ( 'NONE',  ( 75.01583293582056911, -189.7472609257535510, 11.18012358327988665 ) ) ;
#50220 = AXIS2_PLACEMENT_3D ( 'NONE', #38936, #18216, #11083 ) ;
#50221 = EDGE_LOOP ( 'NONE', ( #28445, #17477, #39162, #26736 ) ) ;
#50222 = CARTESIAN_POINT ( 'NONE',  ( -332.3517673607765914, -72.48138011061176655, -29.74944317415788930 ) ) ;
#50223 = CIRCLE ( 'NONE', #14130, 125.0000000000000000 ) ;
#50224 = DIRECTION ( 'NONE',  ( 0.000000000000000000, -1.047444401652940007E-14, -1.000000000000000000 ) ) ;
#50225 = ORIENTED_EDGE ( 'NONE', *, *, #3488, .F. ) ;
#50226 = AXIS2_PLACEMENT_3D ( 'NONE', #30272, #15280, #43127 ) ;
#50227 = LINE ( 'NONE', #47049, #26384 ) ;
#50228 = CARTESIAN_POINT ( 'NONE',  ( -336.3521761649654422, -77.59233547837267508, 37.15394033962009246 ) ) ;
#50229 = CARTESIAN_POINT ( 'NONE',  ( -104.8182102393454045, -189.7472609257535510, 111.5836353223472912 ) ) ;
#50230 = CARTESIAN_POINT ( 'NONE',  ( -47.87232660569025455, -193.5000000000000000, -0.7948544414133454916 ) ) ;
#50231 = VECTOR ( 'NONE', #49429, 1000.000000000000000 ) ;
#50232 = DIRECTION ( 'NONE',  ( 0.000000000000000000, -1.000000000000000000, -0.000000000000000000 ) ) ;
#50233 = ORIENTED_EDGE ( 'NONE', *, *, #13093, .F. ) ;
#50234 = LINE ( 'NONE', #49189, #43076 ) ;
#50235 = DIRECTION ( 'NONE',  ( 0.000000000000000000, 0.000000000000000000, -1.000000000000000000 ) ) ;
#50236 = EDGE_CURVE ( 'NONE', #44743, #29510, #27257, .T. ) ;
#50237 = DIRECTION ( 'NONE',  ( 0.000000000000000000, 1.000000000000000000, 0.000000000000000000 ) ) ;
#50238 = ORIENTED_EDGE ( 'NONE', *, *, #35248, .F. ) ;
#50239 = VECTOR ( 'NONE', #46001, 1000.000000000000114 ) ;
#50240 = LINE ( 'NONE', #25021, #18104 ) ;
#50241 = CARTESIAN_POINT ( 'NONE',  ( -339.1964088526558498, -103.0458197858333165, -55.34326076196084188 ) ) ;
#50242 = LINE ( 'NONE', #33673, #38387 ) ;
#50243 = EDGE_CURVE ( 'NONE', #21929, #46650, #12265, .T. ) ;
#50245 = VECTOR ( 'NONE', #48061, 1000.000000000000114 ) ;
#50244 = DIRECTION ( 'NONE',  ( 0.000000000000000000, 0.1205366802553199113, -0.9927088740980544168 ) ) ;
#50246 = EDGE_CURVE ( 'NONE', #37933, #25927, #15193, .T. ) ;
#50247 = DIRECTION ( 'NONE',  ( 0.000000000000000000, 0.000000000000000000, -1.000000000000000000 ) ) ;
#50248 = CARTESIAN_POINT ( 'NONE',  ( 26.52087324849106054, -173.5000000000000284, -80.00000000000002842 ) ) ;
#50249 = FACE_OUTER_BOUND ( 'NONE', #34713, .T. ) ;
#50250 = VERTEX_POINT ( 'NONE', #174 ) ;
#50251 = CARTESIAN_POINT ( 'NONE',  ( 7.403327498934737960, -193.5000000000000000, -110.6939782313521192 ) ) ;
#50252 = CARTESIAN_POINT ( 'NONE',  ( -47.74129347246712740, -183.6283474603465606, -0.6749830015182022303 ) ) ;
#50254 = ORIENTED_EDGE ( 'NONE', *, *, #10665, .T. ) ;
#50253 = DIRECTION ( 'NONE',  ( 0.9929810960135161402, 0.000000000000000000, 0.1182731709213730997 ) ) ;
#50255 = VECTOR ( 'NONE', #42715, 1000.000000000000000 ) ;
#50256 = ORIENTED_EDGE ( 'NONE', *, *, #43283, .F. ) ;
#50257 = VECTOR ( 'NONE', #51230, 1000.000000000000000 ) ;
#50258 = EDGE_LOOP ( 'NONE', ( #25391, #49987, #28146, #50318 ) ) ;
#50259 = EDGE_CURVE ( 'NONE', #19072, #6572, #15717, .T. ) ;
#50260 = DIRECTION ( 'NONE',  ( -0.2348860457809775482, 0.000000000000000000, -0.9720229140804121926 ) ) ;
#50261 = CIRCLE ( 'NONE', #24249, 60.00000000000000000 ) ;
#50262 = FACE_OUTER_BOUND ( 'NONE', #26278, .T. ) ;
#50263 = CARTESIAN_POINT ( 'NONE',  ( -48.07600332222087758, -175.3837268820161057, -0.9151456172430111335 ) ) ;
#50264 = ORIENTED_EDGE ( 'NONE', *, *, #18951, .T. ) ;
#50265 = LINE ( 'NONE', #15036, #14131 ) ;
#50266 = DIRECTION ( 'NONE',  ( -0.000000000000000000, -0.9709418174260526779, -0.2393156642875547968 ) ) ;
#50267 = CIRCLE ( 'NONE', #34309, 125.0000000000000000 ) ;
#50270 = ORIENTED_EDGE ( 'NONE', *, *, #2527, .T. ) ;
#50269 = CARTESIAN_POINT ( 'NONE',  ( -47.48307690889363641, -177.1207230881787780, 0.08879589532294547560 ) ) ;
#50268 = DIRECTION ( 'NONE',  ( 0.000000000000000000, 0.000000000000000000, 1.000000000000000000 ) ) ;
#50271 = FACE_OUTER_BOUND ( 'NONE', #997, .T. ) ;
#50272 = ORIENTED_EDGE ( 'NONE', *, *, #22869, .F. ) ;
#50273 = DIRECTION ( 'NONE',  ( 1.000000000000000000, -0.000000000000000000, -0.000000000000000000 ) ) ;
#50274 = ORIENTED_EDGE ( 'NONE', *, *, #13453, .F. ) ;
#50275 = DIRECTION ( 'NONE',  ( -0.000000000000000000, -0.1205366802553130001, 0.9927088740980551940 ) ) ;
#50276 = CYLINDRICAL_SURFACE ( 'NONE', #33036, 125.0000000000000000 ) ;
#50277 = DIRECTION ( 'NONE',  ( 1.000000000000000000, 0.000000000000000000, 0.000000000000000000 ) ) ;
#50278 = AXIS2_PLACEMENT_3D ( 'NONE', #28528, #36952, #12758 ) ;
#50279 = CARTESIAN_POINT ( 'NONE',  ( -135.4258661347518853, -175.3837268820161057, -89.80681772907010441 ) ) ;
#50280 = ORIENTED_EDGE ( 'NONE', *, *, #23356, .F. ) ;
#50281 = CARTESIAN_POINT ( 'NONE',  ( 51.05451324771860300, -177.1207230881787780, 75.61781872352698031 ) ) ;
#50282 = DIRECTION ( 'NONE',  ( -0.9995608365087946812, 0.000000000000000000, 0.02963332782254913048 ) ) ;
#50283 = ORIENTED_EDGE ( 'NONE', *, *, #51209, .T. ) ;
#50284 = FACE_OUTER_BOUND ( 'NONE', #44326, .T. ) ;
#50285 = DIRECTION ( 'NONE',  ( 0.000000000000000000, -0.9350162426854169428, -0.3546048870425300148 ) ) ;
#50286 = EDGE_CURVE ( 'NONE', #15404, #23646, #28296, .T. ) ;
#50287 = EDGE_LOOP ( 'NONE', ( #22751, #41464, #20841, #20625 ) ) ;
#50288 = DIRECTION ( 'NONE',  ( -0.9960498426152177842, 0.000000000000000000, 0.08879589532292482545 ) ) ;
#50289 = PLANE ( 'NONE',  #36532 ) ;
#50290 = ORIENTED_EDGE ( 'NONE', *, *, #26239, .F. ) ;
#50291 = CARTESIAN_POINT ( 'NONE',  ( -339.1964088526558498, -137.1341532842531876, -57.40522506028080585 ) ) ;
#50292 = ORIENTED_EDGE ( 'NONE', *, *, #51004, .F. ) ;
#50293 = CIRCLE ( 'NONE', #38534, 125.0000000000000000 ) ;
#50294 = DIRECTION ( 'NONE',  ( 0.000000000000000000, 1.000000000000000000, 0.000000000000000000 ) ) ;
#50295 = DIRECTION ( 'NONE',  ( 0.5586467658036476935, 0.000000000000000000, 0.8294056854502049880 ) ) ;
#50296 = ORIENTED_EDGE ( 'NONE', *, *, #48332, .T. ) ;
#50297 = VECTOR ( 'NONE', #47988, 1000.000000000000000 ) ;
#50298 = CARTESIAN_POINT ( 'NONE',  ( -48.47912675150885065, -187.5000000000000284, 15.00000000000000711 ) ) ;
#50299 = CARTESIAN_POINT ( 'NONE',  ( -124.3803110981236273, -189.7472609257535510, -98.05618656931940791 ) ) ;
#50300 = LINE ( 'NONE', #45327, #8109 ) ;
#50301 = ADVANCED_FACE ( 'NONE', ( #11229 ), #3093, .T. ) ;
#50302 = EDGE_CURVE ( 'NONE', #49743, #24932, #20679, .T. ) ;
#50303 = ADVANCED_FACE ( 'NONE', ( #39592 ), #27523, .F. ) ;
#50304 = EDGE_LOOP ( 'NONE', ( #45170, #16457, #7561, #44700 ) ) ;
#50305 = CARTESIAN_POINT ( 'NONE',  ( 0.000000000000000000, -66.21443277186274656, 14.11962419296515137 ) ) ;
#50306 = EDGE_LOOP ( 'NONE', ( #40820, #27721, #49724, #34768 ) ) ;
#50307 = VECTOR ( 'NONE', #3559, 1000.000000000000000 ) ;
#50308 = EDGE_CURVE ( 'NONE', #11814, #49251, #51456, .T. ) ;
#50309 = PLANE ( 'NONE',  #35352 ) ;
#50310 = CARTESIAN_POINT ( 'NONE',  ( -332.3517673607765914, -160.6539403396202772, 45.90766452162722544 ) ) ;
#50312 = ORIENTED_EDGE ( 'NONE', *, *, #17620, .T. ) ;
#50311 = CARTESIAN_POINT ( 'NONE',  ( -108.5723883981723930, -177.1207230881787780, 109.6074810615846360 ) ) ;
#50313 = ORIENTED_EDGE ( 'NONE', *, *, #43260, .F. ) ;
#50314 = AXIS2_PLACEMENT_3D ( 'NONE', #43899, #7896, #7406 ) ;
#50315 = PLANE ( 'NONE',  #51797 ) ;
#50316 = VECTOR ( 'NONE', #30879, 1000.000000000000000 ) ;
#50317 = DIRECTION ( 'NONE',  ( 0.9890401873221623674, 0.000000000000000000, 0.1476465640024917925 ) ) ;
#50318 = ORIENTED_EDGE ( 'NONE', *, *, #12108, .T. ) ;
#50319 = PLANE ( 'NONE',  #4638 ) ;
#50320 = EDGE_LOOP ( 'NONE', ( #36794, #16838, #26830, #27558 ) ) ;
#50321 = CARTESIAN_POINT ( 'NONE',  ( -173.3968853974275817, -175.3837268820161057, 4.533605064404221174 ) ) ;
#50322 = DIRECTION ( 'NONE',  ( 0.000000000000000000, 0.000000000000000000, -1.000000000000000000 ) ) ;
#50323 = DIRECTION ( 'NONE',  ( 0.000000000000000000, 0.000000000000000000, 1.000000000000000000 ) ) ;
#50324 = DIRECTION ( 'NONE',  ( -0.6528221181905227155, 0.000000000000000000, 0.7575112421616191360 ) ) ;
#50325 = ORIENTED_EDGE ( 'NONE', *, *, #12406, .F. ) ;
#50326 = ORIENTED_EDGE ( 'NONE', *, *, #28899, .T. ) ;
#50327 = ORIENTED_EDGE ( 'NONE', *, *, #39729, .T. ) ;
#50328 = CARTESIAN_POINT ( 'NONE',  ( 4.558749771216711544, -177.1207230881787780, -112.0852863853379233 ) ) ;
#50329 = DIRECTION ( 'NONE',  ( 0.000000000000000000, 1.000000000000000000, -0.000000000000000000 ) ) ;
#50330 = VECTOR ( 'NONE', #27985, 1000.000000000000000 ) ;
#50331 = LINE ( 'NONE', #41911, #7730 ) ;
#50332 = CARTESIAN_POINT ( 'NONE',  ( -48.47912675150885065, -189.7472609257535510, 6.938893903907228378E-15 ) ) ;
#50333 = ORIENTED_EDGE ( 'NONE', *, *, #46202, .T. ) ;
#50334 = AXIS2_PLACEMENT_3D ( 'NONE', #1050, #13666, #29686 ) ;
#50335 = CARTESIAN_POINT ( 'NONE',  ( -336.3521761649654422, -174.9833430614318388, 28.86398714850502856 ) ) ;
#50336 = ORIENTED_EDGE ( 'NONE', *, *, #44578, .T. ) ;
#50337 = ORIENTED_EDGE ( 'NONE', *, *, #33962, .F. ) ;
#50338 = DIRECTION ( 'NONE',  ( 0.000000000000000000, 0.000000000000000000, 1.000000000000000000 ) ) ;
#50339 = DIRECTION ( 'NONE',  ( 0.000000000000000000, 0.9350162426854132791, -0.3546048870425396182 ) ) ;
#50340 = EDGE_CURVE ( 'NONE', #42116, #50802, #47508, .T. ) ;
#50341 = PLANE ( 'NONE',  #42154 ) ;
#50342 = ADVANCED_FACE ( 'NONE', ( #23579 ), #4143, .F. ) ;
#50343 = ADVANCED_FACE ( 'NONE', ( #20156 ), #29065, .T. ) ;
#50344 = LINE ( 'NONE', #22491, #1621 ) ;
#50345 = ORIENTED_EDGE ( 'NONE', *, *, #48112, .F. ) ;
#50346 = DIRECTION ( 'NONE',  ( -0.000000000000000000, 1.000000000000000000, -0.000000000000000000 ) ) ;
#50347 = VERTEX_POINT ( 'NONE', #45642 ) ;
#50348 = EDGE_CURVE ( 'NONE', #2690, #6390, #711, .T. ) ;
#50349 = CIRCLE ( 'NONE', #29353, 125.0000000000000000 ) ;
#50350 = VERTEX_POINT ( 'NONE', #44590 ) ;
#50351 = DIRECTION ( 'NONE',  ( -0.000000000000000000, 1.000000000000000000, -0.000000000000000000 ) ) ;
#50352 = DIRECTION ( 'NONE',  ( 0.000000000000000000, -0.000000000000000000, -1.000000000000000000 ) ) ;
#50353 = VERTEX_POINT ( 'NONE', #37221 ) ;
#50354 = EDGE_CURVE ( 'NONE', #38913, #39413, #1357, .T. ) ;
#50355 = DIRECTION ( 'NONE',  ( 1.000000000000000000, 1.060575238724905929E-16, 6.123233995736780827E-17 ) ) ;
#50356 = LINE ( 'NONE', #22503, #30581 ) ;
#50357 = DIRECTION ( 'NONE',  ( -0.9720229140804107493, 0.000000000000000000, -0.2348860457809842095 ) ) ;
#50358 = EDGE_CURVE ( 'NONE', #39530, #22314, #49325, .T. ) ;
#50359 = LINE ( 'NONE', #18300, #12299 ) ;
#50360 = EDGE_CURVE ( 'NONE', #26773, #13544, #48365, .T. ) ;
#50361 = CARTESIAN_POINT ( 'NONE',  ( -95.18697522258266019, -177.1207230881787780, 115.9455772817713353 ) ) ;
#50362 = ORIENTED_EDGE ( 'NONE', *, *, #7686, .T. ) ;
#50363 = EDGE_CURVE ( 'NONE', #51994, #45030, #44155, .T. ) ;
#50364 = VECTOR ( 'NONE', #17359, 1000.000000000000000 ) ;
#50365 = DIRECTION ( 'NONE',  ( -0.000000000000000000, -0.8229838658936516893, 0.5680647467311626952 ) ) ;
#50366 = ORIENTED_EDGE ( 'NONE', *, *, #8035, .T. ) ;
#50367 = EDGE_CURVE ( 'NONE', #20252, #5652, #25707, .T. ) ;
#50368 = ORIENTED_EDGE ( 'NONE', *, *, #42309, .F. ) ;
#50369 = LINE ( 'NONE', #42460, #36348 ) ;
#50370 = ORIENTED_EDGE ( 'NONE', *, *, #6090, .F. ) ;
#50371 = PRODUCT_DEFINITION_SHAPE ( 'NONE', 'NONE',  #11949 ) ;
#50372 = CARTESIAN_POINT ( 'NONE',  ( -161.6832731452239784, -189.7472609257535510, -53.00774697410100345 ) ) ;
#50373 = ORIENTED_EDGE ( 'NONE', *, *, #24198, .T. ) ;
#50374 = FACE_OUTER_BOUND ( 'NONE', #287, .T. ) ;
#50375 = CARTESIAN_POINT ( 'NONE',  ( -163.3872488209693472, -183.6283474603465606, -49.20491319441547517 ) ) ;
#50376 = ORIENTED_EDGE ( 'NONE', *, *, #6854, .F. ) ;
#50377 = DIRECTION ( 'NONE',  ( 0.6068001458186002006, 0.000000000000000000, -0.7948544414133481562 ) ) ;
#50378 = CARTESIAN_POINT ( 'NONE',  ( -157.8637630444124511, -189.7472609257535510, -60.49794494914015530 ) ) ;
#50379 = DIRECTION ( 'NONE',  ( -0.9473263538541946138, 0.000000000000000000, 0.3202698538628279690 ) ) ;
#50380 = EDGE_CURVE ( 'NONE', #37183, #29247, #1485, .T. ) ;
#50381 = ORIENTED_EDGE ( 'NONE', *, *, #3037, .F. ) ;
#50382 = EDGE_LOOP ( 'NONE', ( #17308, #31855, #48322, #44696 ) ) ;
#50383 = AXIS2_PLACEMENT_3D ( 'NONE', #24776, #40794, #37116 ) ;
#50385 = ORIENTED_EDGE ( 'NONE', *, *, #39739, .F. ) ;
#50384 = VECTOR ( 'NONE', #40840, 1000.000000000000114 ) ;
#50386 = CARTESIAN_POINT ( 'NONE',  ( -332.3517673607765914, -69.63373947859463442, 26.42775013958025454 ) ) ;
#50387 = DIRECTION ( 'NONE',  ( -0.000000000000000000, -0.3546048870425396182, -0.9350162426854132791 ) ) ;
#50388 = CARTESIAN_POINT ( 'NONE',  ( -45.12595152424214007, -183.6283474603465606, -123.9551692589637497 ) ) ;
#50389 = DIRECTION ( 'NONE',  ( -0.000000000000000000, 1.000000000000000000, -0.000000000000000000 ) ) ;
#50390 = ORIENTED_EDGE ( 'NONE', *, *, #18532, .T. ) ;
#50391 = DIRECTION ( 'NONE',  ( 0.000000000000000000, 0.000000000000000000, 1.000000000000000000 ) ) ;
#50392 = EDGE_CURVE ( 'NONE', #10684, #17102, #15662, .T. ) ;
#50393 = ORIENTED_EDGE ( 'NONE', *, *, #13724, .F. ) ;
#50395 = ORIENTED_EDGE ( 'NONE', *, *, #12712, .F. ) ;
#50394 = CARTESIAN_POINT ( 'NONE',  ( 69.72248760683812918, -183.6283474603465606, -37.47770156625421833 ) ) ;
#50396 = ORIENTED_EDGE ( 'NONE', *, *, #34609, .T. ) ;
#50397 = VECTOR ( 'NONE', #35418, 1000.000000000000000 ) ;
#50398 = DIRECTION ( 'NONE',  ( 0.7378332790417285736, 0.000000000000000000, -0.6749830015182091136 ) ) ;
#50399 = EDGE_LOOP ( 'NONE', ( #1885, #24381, #39074, #40197 ) ) ;
#50400 = CARTESIAN_POINT ( 'NONE',  ( -305.0000000000000568, -78.25935320507949200, -39.41172259083896279 ) ) ;
#50401 = ORIENTED_EDGE ( 'NONE', *, *, #50236, .F. ) ;
#50402 = EDGE_CURVE ( 'NONE', #20303, #39961, #4921, .T. ) ;
#50403 = EDGE_CURVE ( 'NONE', #31054, #5412, #14805, .T. ) ;
#50404 = CARTESIAN_POINT ( 'NONE',  ( -126.3604277550461035, -177.1207230881787780, 96.49160960477098570 ) ) ;
#50405 = ADVANCED_FACE ( 'NONE', ( #20946 ), #36966, .F. ) ;
#50406 = ADVANCED_FACE ( 'NONE', ( #17005 ), #13314, .F. ) ;
#50407 = CARTESIAN_POINT ( 'NONE',  ( -109.9568094315246327, -177.1207230881787780, -108.8370090194290611 ) ) ;
#50408 = ORIENTED_EDGE ( 'NONE', *, *, #45193, .F. ) ;
#50409 = FACE_BOUND ( 'NONE', #20446, .T. ) ;
#50410 = ORIENTED_EDGE ( 'NONE', *, *, #3326, .F. ) ;
#50411 = ADVANCED_FACE ( 'NONE', ( #5181 ), #49059, .T. ) ;
#50412 = VERTEX_POINT ( 'NONE', #9119 ) ;
#50413 = CARTESIAN_POINT ( 'NONE',  ( -332.3517673607765914, -165.9166037625627439, 41.09453333279358134 ) ) ;
#50414 = DIRECTION ( 'NONE',  ( -0.000000000000000000, -3.491481338843133355E-15, -1.000000000000000000 ) ) ;
#50415 = EDGE_CURVE ( 'NONE', #10170, #13304, #4384, .T. ) ;
#50416 = ADVANCED_FACE ( 'NONE', ( #21195 ), #45384, .F. ) ;
#50417 = DIRECTION ( 'NONE',  ( -0.000000000000000000, 0.4647231720437755564, 0.8854560256532062468 ) ) ;
#50418 = DIRECTION ( 'NONE',  ( 0.000000000000000000, 1.000000000000000000, 0.000000000000000000 ) ) ;
#50419 = ORIENTED_EDGE ( 'NONE', *, *, #8806, .T. ) ;
#50420 = DIRECTION ( 'NONE',  ( -0.000000000000000000, 1.000000000000000000, -0.000000000000000000 ) ) ;
#50421 = CARTESIAN_POINT ( 'NONE',  ( -171.5708553757489767, -193.5000000000000000, 14.98512977653260414 ) ) ;
#50422 = CARTESIAN_POINT ( 'NONE',  ( -48.47912675150885065, -183.6283474603465606, 6.938893903907228378E-15 ) ) ;
#50423 = LINE ( 'NONE', #26746, #14496 ) ;
#50424 = EDGE_CURVE ( 'NONE', #35744, #48832, #20410, .T. ) ;
#50425 = ORIENTED_EDGE ( 'NONE', *, *, #44431, .F. ) ;
#50426 = FACE_OUTER_BOUND ( 'NONE', #12432, .T. ) ;
#50427 = DIRECTION ( 'NONE',  ( 0.000000000000000000, 0.000000000000000000, 1.000000000000000000 ) ) ;
#50428 = AXIS2_PLACEMENT_3D ( 'NONE', #28904, #24716, #28384 ) ;
#50429 = EDGE_CURVE ( 'NONE', #2064, #33404, #32410, .T. ) ;
#50430 = AXIS2_PLACEMENT_3D ( 'NONE', #31591, #3475, #19505 ) ;
#50431 = FACE_OUTER_BOUND ( 'NONE', #32789, .T. ) ;
#50432 = VERTEX_POINT ( 'NONE', #29848 ) ;
#50433 = EDGE_CURVE ( 'NONE', #16426, #42195, #10393, .T. ) ;
#50434 = CARTESIAN_POINT ( 'NONE',  ( -81.47409310123215676, -193.5000000000000000, -119.5301634136912412 ) ) ;
#50435 = CARTESIAN_POINT ( 'NONE',  ( -48.36085358058748795, -177.1207230881787780, 0.9929810960135245779 ) ) ;
#50436 = EDGE_CURVE ( 'NONE', #16821, #16432, #22225, .T. ) ;
#50437 = VERTEX_POINT ( 'NONE', #42186 ) ;
#50438 = CARTESIAN_POINT ( 'NONE',  ( -169.1033029113419559, -189.7472609257535510, 32.78426643622744052 ) ) ;
#50439 = EDGE_LOOP ( 'NONE', ( #41630, #20981, #2555, #732 ) ) ;
#50440 = EDGE_CURVE ( 'NONE', #38472, #28072, #22748, .T. ) ;
#50441 = LINE ( 'NONE', #21799, #12498 ) ;
#50442 = AXIS2_PLACEMENT_3D ( 'NONE', #22463, #38480, #43185 ) ;
#50443 = DIRECTION ( 'NONE',  ( 1.000000000000000000, 0.000000000000000000, 0.000000000000000000 ) ) ;
#50444 = LINE ( 'NONE', #14960, #32959 ) ;
#50445 = PLANE ( 'NONE',  #50154 ) ;
#50446 = DIRECTION ( 'NONE',  ( 0.000000000000000000, 0.000000000000000000, 1.000000000000000000 ) ) ;
#50447 = ORIENTED_EDGE ( 'NONE', *, *, #17297, .F. ) ;
#50449 = EDGE_CURVE ( 'NONE', #28974, #36109, #1738, .T. ) ;
#50448 = CARTESIAN_POINT ( 'NONE',  ( -49.25565061422690150, -193.5000000000000000, 0.6300878435817109935 ) ) ;
#50450 = ORIENTED_EDGE ( 'NONE', *, *, #27726, .F. ) ;
#50451 = LINE ( 'NONE', #51476, #27549 ) ;
#50452 = ORIENTED_EDGE ( 'NONE', *, *, #8869, .T. ) ;
#50453 = CARTESIAN_POINT ( 'NONE',  ( 67.64905612629584652, -177.1207230881787780, -43.47841891815122750 ) ) ;
#50454 = VECTOR ( 'NONE', #10794, 1000.000000000000000 ) ;
#50455 = VECTOR ( 'NONE', #24683, 1000.000000000000114 ) ;
#50456 = DIRECTION ( 'NONE',  ( -8.718379230999707126E-17, -0.6631226582408017434, -0.7485107481710954191 ) ) ;
#50457 = DIRECTION ( 'NONE',  ( 0.000000000000000000, -1.000000000000000000, 0.000000000000000000 ) ) ;
#50458 = EDGE_LOOP ( 'NONE', ( #17272, #3214, #33307, #21784 ) ) ;
#50461 = VERTEX_POINT ( 'NONE', #42452 ) ;
#50460 = DIRECTION ( 'NONE',  ( 0.000000000000000000, 1.000000000000000000, 0.000000000000000000 ) ) ;
#50459 = CARTESIAN_POINT ( 'NONE',  ( -48.47912675150885065, -189.7472609257535510, 6.938893903907228378E-15 ) ) ;
#50462 = LINE ( 'NONE', #17877, #19750 ) ;
#50463 = ORIENTED_EDGE ( 'NONE', *, *, #6677, .T. ) ;
#50464 = CARTESIAN_POINT ( 'NONE',  ( -49.47517659412407198, -189.7472609257535510, 0.08879589532293177823 ) ) ;
#50465 = EDGE_LOOP ( 'NONE', ( #12388, #24528, #50217, #47151 ) ) ;
#50466 = ADVANCED_FACE ( 'NONE', ( #34812, #9894 ), #25914, .F. ) ;
#50467 = ADVANCED_FACE ( 'NONE', ( #14606 ), #42725, .F. ) ;
#50468 = CARTESIAN_POINT ( 'NONE',  ( -152.8713435144644848, -177.1207230881787780, -68.75510947788595217 ) ) ;
#50471 = ORIENTED_EDGE ( 'NONE', *, *, #10777, .T. ) ;
#50470 = FACE_OUTER_BOUND ( 'NONE', #34721, .T. ) ;
#50469 = DIRECTION ( 'NONE',  ( -0.000000000000000000, 0.8854560256532157947, 0.4647231720437573488 ) ) ;
#50472 = EDGE_LOOP ( 'NONE', ( #20397, #10408, #43991, #20046 ) ) ;
#50473 = DIRECTION ( 'NONE',  ( -0.000000000000000000, 1.000000000000000000, -0.000000000000000000 ) ) ;
#50474 = ORIENTED_EDGE ( 'NONE', *, *, #41687, .F. ) ;
#50475 = LINE ( 'NONE', #30235, #17804 ) ;
#50477 = AXIS2_PLACEMENT_3D ( 'NONE', #42867, #10552, #6363 ) ;
#50476 = DIRECTION ( 'NONE',  ( 0.000000000000000000, -0.000000000000000000, -1.000000000000000000 ) ) ;
#50478 = ORIENTED_EDGE ( 'NONE', *, *, #37537, .T. ) ;
#50479 = CARTESIAN_POINT ( 'NONE',  ( 71.73509643893275722, -193.5000000000000000, -30.40954281680804172 ) ) ;
#50480 = DIRECTION ( 'NONE',  ( -0.000000000000000000, 1.000000000000000000, -0.000000000000000000 ) ) ;
#50481 = CARTESIAN_POINT ( 'NONE',  ( -365.0000000000001137, -78.50000000000002842, 5.000000000000001776 ) ) ;
#50482 = FACE_OUTER_BOUND ( 'NONE', #12689, .T. ) ;
#50483 = PLANE ( 'NONE',  #36624 ) ;
#50484 = ORIENTED_EDGE ( 'NONE', *, *, #36154, .T. ) ;
#50485 = SHAPE_REPRESENTATION_RELATIONSHIP ( 'NONE' , 'NONE' ,  #15324, #3572 ) ;
#50486 = LINE ( 'NONE', #46289, #34669 ) ;
#50487 = DIRECTION ( 'NONE',  ( -0.000000000000000000, -1.000000000000000000, 0.000000000000000000 ) ) ;
#50488 = CARTESIAN_POINT ( 'NONE',  ( 51.70113075622899856, 30.00000000000000355, -45.78969942005421956 ) ) ;
#50489 = EDGE_LOOP ( 'NONE', ( #24442, #29091, #20163, #47217 ) ) ;
#50490 = CARTESIAN_POINT ( 'NONE',  ( 75.51463005422468200, -177.1207230881787780, -1.322128892811231360 ) ) ;
#50491 = DIRECTION ( 'NONE',  ( -0.000000000000000000, -0.9350162426854121689, 0.3546048870425426158 ) ) ;
#50492 = ADVANCED_FACE ( 'NONE', ( #37990 ), #5952, .T. ) ;
#50493 = VECTOR ( 'NONE', #18549, 1000.000000000000114 ) ;
#50494 = FACE_OUTER_BOUND ( 'NONE', #30414, .T. ) ;
#50495 = DIRECTION ( 'NONE',  ( 0.000000000000000000, 0.000000000000000000, 1.000000000000000000 ) ) ;
#50496 = EDGE_LOOP ( 'NONE', ( #27280, #40780, #42863, #17798 ) ) ;
#50497 = VECTOR ( 'NONE', #19630, 1000.000000000000114 ) ;
#50498 = ADVANCED_FACE ( 'NONE', ( #26692 ), #10141, .F. ) ;
#50499 = AXIS2_PLACEMENT_3D ( 'NONE', #12130, #39234, #43693 ) ;
#50500 = DIRECTION ( 'NONE',  ( 0.000000000000000000, -1.000000000000000000, 0.000000000000000000 ) ) ;
#50501 = CARTESIAN_POINT ( 'NONE',  ( 49.10711742958948633, -175.3837268820161057, 78.11481899503480975 ) ) ;
#50502 = LINE ( 'NONE', #10285, #22873 ) ;
#50503 = FACE_OUTER_BOUND ( 'NONE', #51039, .T. ) ;
#50504 = EDGE_LOOP ( 'NONE', ( #49491, #30992, #24681, #49808 ) ) ;
#50505 = DIRECTION ( 'NONE',  ( 0.000000000000000000, 0.000000000000000000, 1.000000000000000000 ) ) ;
#50506 = AXIS2_PLACEMENT_3D ( 'NONE', #44800, #24821, #8277 ) ;
#50507 = DIRECTION ( 'NONE',  ( -0.3482016354344059095, 0.000000000000000000, 0.9374196611341183427 ) ) ;
#50508 = VERTEX_POINT ( 'NONE', #49840 ) ;
#50509 = ORIENTED_EDGE ( 'NONE', *, *, #31759, .F. ) ;
#50510 = VECTOR ( 'NONE', #34350, 1000.000000000000000 ) ;
#50511 = ORIENTED_EDGE ( 'NONE', *, *, #644, .T. ) ;
#50512 = DIRECTION ( 'NONE',  ( -0.000000000000000000, 0.9927088740980556381, 0.1205366802553095307 ) ) ;
#50513 = DIRECTION ( 'NONE',  ( -0.000000000000000000, 1.000000000000000000, 0.000000000000000000 ) ) ;
#50514 = DIRECTION ( 'NONE',  ( 0.000000000000000000, 0.000000000000000000, -1.000000000000000000 ) ) ;
#50515 = EDGE_LOOP ( 'NONE', ( #3520, #12, #1820, #30995 ) ) ;
#50516 = FACE_OUTER_BOUND ( 'NONE', #2452, .T. ) ;
#50517 = CARTESIAN_POINT ( 'NONE',  ( 72.95485052494851175, -177.1207230881787780, -29.64437826672757481 ) ) ;
#50520 = ORIENTED_EDGE ( 'NONE', *, *, #26750, .T. ) ;
#50519 = DIRECTION ( 'NONE',  ( 0.000000000000000000, -1.000000000000000000, 0.000000000000000000 ) ) ;
#50518 = DIRECTION ( 'NONE',  ( -0.000000000000000000, -0.3546048870425396182, -0.9350162426854132791 ) ) ;
#50521 = DIRECTION ( 'NONE',  ( -0.000000000000000000, 1.000000000000000000, -0.000000000000000000 ) ) ;
#50522 = ORIENTED_EDGE ( 'NONE', *, *, #9829, .T. ) ;
#50523 = DIRECTION ( 'NONE',  ( 1.000000000000000000, 0.000000000000000000, 0.000000000000000000 ) ) ;
#50524 = VECTOR ( 'NONE', #42574, 1000.000000000000000 ) ;
#50525 = ORIENTED_EDGE ( 'NONE', *, *, #28177, .T. ) ;
#50526 = EDGE_CURVE ( 'NONE', #14314, #8372, #50103, .T. ) ;
#50527 = FACE_OUTER_BOUND ( 'NONE', #22520, .T. ) ;
#50528 = CARTESIAN_POINT ( 'NONE',  ( 40.26790151320560085, -193.5000000000000000, -86.60307583628353711 ) ) ;
#50529 = VECTOR ( 'NONE', #12966, 1000.000000000000114 ) ;
#50530 = DIRECTION ( 'NONE',  ( 0.000000000000000000, 0.000000000000000000, -1.000000000000000000 ) ) ;
#50531 = AXIS2_PLACEMENT_3D ( 'NONE', #26820, #6860, #30256 ) ;
#50532 = VERTEX_POINT ( 'NONE', #30893 ) ;
#50533 = CYLINDRICAL_SURFACE ( 'NONE', #47470, 125.0000000000000000 ) ;
#50534 = FACE_OUTER_BOUND ( 'NONE', #36681, .T. ) ;
#50535 = ORIENTED_EDGE ( 'NONE', *, *, #31824, .F. ) ;
#50536 = DIRECTION ( 'NONE',  ( -0.000000000000000000, 1.000000000000000000, -0.000000000000000000 ) ) ;
#50537 = CARTESIAN_POINT ( 'NONE',  ( -47.50057025920934706, -193.5000000000000000, -0.2059786187410884151 ) ) ;
#50538 = ORIENTED_EDGE ( 'NONE', *, *, #31519, .T. ) ;
#50539 = DIRECTION ( 'NONE',  ( -1.000000000000000000, 0.000000000000000000, 0.000000000000000000 ) ) ;
#50540 = AXIS2_PLACEMENT_3D ( 'NONE', #46886, #3737, #3247 ) ;
#50541 = CARTESIAN_POINT ( 'NONE',  ( 16.00000000000000711, 65.00000000000000000, 1.959434878635766315E-15 ) ) ;
#50542 = ORIENTED_EDGE ( 'NONE', *, *, #16216, .T. ) ;
#50543 = CARTESIAN_POINT ( 'NONE',  ( 18.82962626094778003, -183.6283474603465606, 104.1428419024404377 ) ) ;
#50544 = ORIENTED_EDGE ( 'NONE', *, *, #8351, .F. ) ;
#50545 = AXIS2_PLACEMENT_3D ( 'NONE', #1018, #28609, #49126 ) ;
#50546 = VECTOR ( 'NONE', #9861, 1000.000000000000000 ) ;
#50547 = CARTESIAN_POINT ( 'NONE',  ( -339.1964088526558498, -171.7720157143598669, 33.92731199008546383 ) ) ;
#50548 = DIRECTION ( 'NONE',  ( 1.000000000000000000, -0.000000000000000000, -0.000000000000000000 ) ) ;
#50549 = ADVANCED_FACE ( 'NONE', ( #6477 ), #33244, .T. ) ;
#50550 = ORIENTED_EDGE ( 'NONE', *, *, #7554, .T. ) ;
#50551 = LINE ( 'NONE', #6666, #36977 ) ;
#50552 = DIRECTION ( 'NONE',  ( 0.000000000000000000, 0.000000000000000000, -1.000000000000000000 ) ) ;
#50553 = DIRECTION ( 'NONE',  ( 0.000000000000000000, 0.000000000000000000, 1.000000000000000000 ) ) ;
#50554 = ORIENTED_EDGE ( 'NONE', *, *, #21689, .F. ) ;
#50555 = CARTESIAN_POINT ( 'NONE',  ( 56.81546028627039391, -189.7472609257535510, 65.49088066501711580 ) ) ;
#50556 = EDGE_LOOP ( 'NONE', ( #11279, #30624, #6007, #7212 ) ) ;
#50557 = LINE ( 'NONE', #6671, #43757 ) ;
#50558 = CARTESIAN_POINT ( 'NONE',  ( 0.000000000000000000, -43.50000000000000000, 30.00000000000000355 ) ) ;
#50560 = ORIENTED_EDGE ( 'NONE', *, *, #48145, .F. ) ;
#50559 = CARTESIAN_POINT ( 'NONE',  ( -332.3517673607765914, -176.9651911376907094, -25.08789112700655721 ) ) ;
#50561 = VERTEX_POINT ( 'NONE', #1993 ) ;
#50562 = DIRECTION ( 'NONE',  ( -0.000000000000000000, 0.9927088740980553050, 0.1205366802553130001 ) ) ;
#50563 = AXIS2_PLACEMENT_3D ( 'NONE', #21072, #37096, #40772 ) ;
#50564 = DIRECTION ( 'NONE',  ( 0.000000000000000000, 0.000000000000000000, -1.000000000000000000 ) ) ;
#50565 = VERTEX_POINT ( 'NONE', #34058 ) ;
#50566 = CARTESIAN_POINT ( 'NONE',  ( -173.4724443937511467, -183.6283474603465606, 1.292495564989519785 ) ) ;
#50567 = ORIENTED_EDGE ( 'NONE', *, *, #18546, .T. ) ;
#50568 = LINE ( 'NONE', #6933, #8200 ) ;
#50569 = DIRECTION ( 'NONE',  ( 0.000000000000000000, 0.000000000000000000, -1.000000000000000000 ) ) ;
#50570 = EDGE_CURVE ( 'NONE', #35696, #43188, #3878, .T. ) ;
#50571 = DIRECTION ( 'NONE',  ( 0.000000000000000000, 0.000000000000000000, -1.000000000000000000 ) ) ;
#50572 = LINE ( 'NONE', #26653, #43366 ) ;
#50573 = ORIENTED_EDGE ( 'NONE', *, *, #35633, .T. ) ;
#50574 = ORIENTED_EDGE ( 'NONE', *, *, #9960, .T. ) ;
#50575 = VECTOR ( 'NONE', #12956, 1000.000000000000000 ) ;
#50576 = EDGE_LOOP ( 'NONE', ( #22085, #14056, #40341, #44898 ) ) ;
#50577 = EDGE_CURVE ( 'NONE', #37919, #16257, #14100, .T. ) ;
#50578 = DIRECTION ( 'NONE',  ( 0.000000000000000000, 0.000000000000000000, -1.000000000000000000 ) ) ;
#50579 = DIRECTION ( 'NONE',  ( -0.000000000000000000, 1.000000000000000000, -0.000000000000000000 ) ) ;
#50580 = VECTOR ( 'NONE', #44586, 1000.000000000000000 ) ;
#50581 = CIRCLE ( 'NONE', #20361, 125.0000000000000000 ) ;
#50582 = FACE_OUTER_BOUND ( 'NONE', #13613, .T. ) ;
#50583 = CARTESIAN_POINT ( 'NONE',  ( -48.47912675150885065, -189.7472609257535510, 6.938893903907228378E-15 ) ) ;
#50584 = EDGE_LOOP ( 'NONE', ( #41983, #35006, #4893, #14103 ) ) ;
#50585 = ADVANCED_FACE ( 'NONE', ( #30116 ), #25649, .T. ) ;
#50586 = AXIS2_PLACEMENT_3D ( 'NONE', #1561, #25987, #42261 ) ;
#50587 = DIRECTION ( 'NONE',  ( -0.000000000000000000, 0.9350162426854194964, 0.3546048870425235200 ) ) ;
#50588 = DIRECTION ( 'NONE',  ( 0.000000000000000000, 1.000000000000000000, -0.000000000000000000 ) ) ;
#50589 = EDGE_CURVE ( 'NONE', #43312, #28285, #50359, .T. ) ;
#50590 = VERTEX_POINT ( 'NONE', #31141 ) ;
#50591 = VERTEX_POINT ( 'NONE', #42969 ) ;
#50592 = DIRECTION ( 'NONE',  ( 0.000000000000000000, -0.1205366802553268640, -0.9927088740980535286 ) ) ;
#50593 = EDGE_CURVE ( 'NONE', #46272, #34416, #3296, .T. ) ;
#50594 = DIRECTION ( 'NONE',  ( -0.5315839928299663786, 0.000000000000000000, 0.8470055835512245723 ) ) ;
#50595 = DIRECTION ( 'NONE',  ( 0.000000000000000000, -0.000000000000000000, 1.000000000000000000 ) ) ;
#50596 = VECTOR ( 'NONE', #9364, 1000.000000000000000 ) ;
#50597 = DIRECTION ( 'NONE',  ( 0.000000000000000000, 0.000000000000000000, 1.000000000000000000 ) ) ;
#50598 = DIRECTION ( 'NONE',  ( -0.000000000000000000, 1.000000000000000000, 0.000000000000000000 ) ) ;
#50599 = ORIENTED_EDGE ( 'NONE', *, *, #30162, .T. ) ;
#50600 = PLANE ( 'NONE',  #47739 ) ;
#50601 = VECTOR ( 'NONE', #41232, 1000.000000000000000 ) ;
#50602 = EDGE_LOOP ( 'NONE', ( #48750, #8604, #28499, #7796 ) ) ;
#50603 = FACE_OUTER_BOUND ( 'NONE', #36524, .T. ) ;
#50604 = FACE_OUTER_BOUND ( 'NONE', #30409, .T. ) ;
#50605 = EDGE_CURVE ( 'NONE', #4319, #45025, #31395, .T. ) ;
#50606 = ORIENTED_EDGE ( 'NONE', *, *, #42247, .T. ) ;
#50607 = CARTESIAN_POINT ( 'NONE',  ( -143.3583119192899460, -183.6283474603465606, -81.38144888055207105 ) ) ;
#50608 = CARTESIAN_POINT ( 'NONE',  ( -336.3521761649654422, -73.44864141332200802, 31.34948880313848107 ) ) ;
#50609 = DIRECTION ( 'NONE',  ( -0.000000000000000000, 1.000000000000000000, 0.000000000000000000 ) ) ;
#50610 = CIRCLE ( 'NONE', #27929, 125.0000000000000000 ) ;
#50611 = DIRECTION ( 'NONE',  ( 0.000000000000000000, 1.000000000000000000, 0.000000000000000000 ) ) ;
#50612 = AXIS2_PLACEMENT_3D ( 'NONE', #31991, #8595, #47784 ) ;
#50613 = DIRECTION ( 'NONE',  ( -0.000000000000000000, 1.000000000000000000, -0.000000000000000000 ) ) ;
#50614 = EDGE_LOOP ( 'NONE', ( #30067, #23773, #31896, #35377 ) ) ;
#50615 = AXIS2_PLACEMENT_3D ( 'NONE', #4265, #36314, #41038 ) ;
#50616 = FACE_OUTER_BOUND ( 'NONE', #44007, .T. ) ;
#50617 = ORIENTED_EDGE ( 'NONE', *, *, #37759, .F. ) ;
#50618 = ORIENTED_EDGE ( 'NONE', *, *, #36276, .F. ) ;
#50619 = DIRECTION ( 'NONE',  ( -0.000000000000000000, -1.000000000000000000, 0.000000000000000000 ) ) ;
#50620 = AXIS2_PLACEMENT_3D ( 'NONE', #34568, #50619, #7245 ) ;
#50621 = VERTEX_POINT ( 'NONE', #7748 ) ;
#50622 = CARTESIAN_POINT ( 'NONE',  ( -48.47912675150885065, -177.1207230881787780, 6.938893903907228378E-15 ) ) ;
#50623 = ORIENTED_EDGE ( 'NONE', *, *, #27243, .F. ) ;
#50624 = DIRECTION ( 'NONE',  ( -0.3202698538628350744, 0.000000000000000000, -0.9473263538541923934 ) ) ;
#50625 = CARTESIAN_POINT ( 'NONE',  ( -170.9669310976187830, -189.7472609257535510, -24.93467037017130394 ) ) ;
#50626 = EDGE_LOOP ( 'NONE', ( #22984, #39461, #8850, #13711 ) ) ;
#50627 = DIRECTION ( 'NONE',  ( 0.000000000000000000, 0.000000000000000000, -1.000000000000000000 ) ) ;
#50628 = VECTOR ( 'NONE', #37343, 1000.000000000000114 ) ;
#50629 = EDGE_CURVE ( 'NONE', #50821, #3974, #27457, .T. ) ;
#50630 = EDGE_CURVE ( 'NONE', #8865, #48981, #19329, .T. ) ;
#50631 = DIRECTION ( 'NONE',  ( -1.000000000000000000, 0.000000000000000000, 0.000000000000000000 ) ) ;
#50632 = LINE ( 'NONE', #30382, #22356 ) ;
#50633 = VERTEX_POINT ( 'NONE', #47187 ) ;
#50634 = VERTEX_POINT ( 'NONE', #20094 ) ;
#50635 = VECTOR ( 'NONE', #40516, 1000.000000000000000 ) ;
#50636 = ORIENTED_EDGE ( 'NONE', *, *, #36507, .F. ) ;
#50637 = CARTESIAN_POINT ( 'NONE',  ( 2.669657140899374337, -189.7472609257535510, 114.0561348912355868 ) ) ;
#50638 = CARTESIAN_POINT ( 'NONE',  ( -49.46816693883101834, -177.1207230881787780, 0.1476465640024780257 ) ) ;
#50639 = CARTESIAN_POINT ( 'NONE',  ( -144.0067397530739584, -183.6283474603465606, -80.61932246194587037 ) ) ;
#50640 = DIRECTION ( 'NONE',  ( 1.000000000000000000, 0.000000000000000000, 0.000000000000000000 ) ) ;
#50641 = CARTESIAN_POINT ( 'NONE',  ( -48.47912675150885065, -177.1207230881787780, 6.938893903907228378E-15 ) ) ;
#50642 = ORIENTED_EDGE ( 'NONE', *, *, #3174, .F. ) ;
#50643 = EDGE_CURVE ( 'NONE', #16559, #38969, #3802, .T. ) ;
#50644 = VECTOR ( 'NONE', #20259, 1000.000000000000000 ) ;
#50645 = EDGE_CURVE ( 'NONE', #45117, #50764, #35863, .T. ) ;
#50646 = CARTESIAN_POINT ( 'NONE',  ( -280.0000000000000000, -123.5000000000000284, -20.00000000000001066 ) ) ;
#50647 = EDGE_LOOP ( 'NONE', ( #9778, #21137, #18384, #22335 ) ) ;
#50649 = ORIENTED_EDGE ( 'NONE', *, *, #3186, .T. ) ;
#50648 = CARTESIAN_POINT ( 'NONE',  ( -137.6740394605055542, -183.6283474603465606, -86.14171647324867820 ) ) ;
#50650 = VECTOR ( 'NONE', #26202, 1000.000000000000000 ) ;
#50651 = ORIENTED_EDGE ( 'NONE', *, *, #23988, .F. ) ;
#50652 = ADVANCED_FACE ( 'NONE', ( #27712 ), #11164, .F. ) ;
#50653 = CARTESIAN_POINT ( 'NONE',  ( -12.13476221271687905, -189.7472609257535510, 119.5996955107804780 ) ) ;
#50654 = ORIENTED_EDGE ( 'NONE', *, *, #3409, .F. ) ;
#50655 = CARTESIAN_POINT ( 'NONE',  ( -108.6269575285486724, -183.6283474603465606, -108.4360005853207696 ) ) ;
#50656 = EDGE_CURVE ( 'NONE', #18494, #37026, #29109, .T. ) ;
#50657 = CARTESIAN_POINT ( 'NONE',  ( -139.0630283577175987, -183.6283474603465606, -86.13684908212448477 ) ) ;
#50658 = LINE ( 'NONE', #22271, #16706 ) ;
#50659 = ORIENTED_EDGE ( 'NONE', *, *, #5440, .T. ) ;
#50660 = DIRECTION ( 'NONE',  ( 0.000000000000000000, 0.000000000000000000, -1.000000000000000000 ) ) ;
#50661 = ORIENTED_EDGE ( 'NONE', *, *, #9737, .F. ) ;
#50662 = ORIENTED_EDGE ( 'NONE', *, *, #33318, .T. ) ;
#50663 = LINE ( 'NONE', #14658, #43005 ) ;
#50664 = LINE ( 'NONE', #26212, #21396 ) ;
#50665 = DIRECTION ( 'NONE',  ( 0.000000000000000000, 0.000000000000000000, -1.000000000000000000 ) ) ;
#50666 = VERTEX_POINT ( 'NONE', #47710 ) ;
#50667 = DIRECTION ( 'NONE',  ( 0.000000000000000000, -0.000000000000000000, -1.000000000000000000 ) ) ;
#50668 = AXIS2_PLACEMENT_3D ( 'NONE', #20470, #23891, #491 ) ;
#50669 = DIRECTION ( 'NONE',  ( -0.000000000000000000, 1.000000000000000000, -0.000000000000000000 ) ) ;
#50670 = CONTEXT_DEPENDENT_SHAPE_REPRESENTATION ( #16244, #33977 ) ;
#50671 = DIRECTION ( 'NONE',  ( -0.000000000000000000, 1.000000000000000000, -0.000000000000000000 ) ) ;
#50672 = LINE ( 'NONE', #46471, #11095 ) ;
#50673 = VERTEX_POINT ( 'NONE', #23005 ) ;
#50674 = DIRECTION ( 'NONE',  ( -0.4300652022765183435, 0.000000000000000000, -0.9027978299657446470 ) ) ;
#50675 = FACE_OUTER_BOUND ( 'NONE', #35409, .T. ) ;
#50676 = AXIS2_PLACEMENT_3D ( 'NONE', #19131, #42781, #2831 ) ;
#50677 = FACE_BOUND ( 'NONE', #7031, .T. ) ;
#50678 = VERTEX_POINT ( 'NONE', #19830 ) ;
#50679 = DIRECTION ( 'NONE',  ( 0.000000000000000000, -1.000000000000000000, 0.000000000000000000 ) ) ;
#50680 = CARTESIAN_POINT ( 'NONE',  ( -123.4791267515088435, -198.5000000000000000, 70.00000000000000000 ) ) ;
#50681 = ORIENTED_EDGE ( 'NONE', *, *, #28488, .T. ) ;
#50682 = LINE ( 'NONE', #43049, #38826 ) ;
#50683 = AXIS2_PLACEMENT_3D ( 'NONE', #30270, #46317, #10301 ) ;
#50684 = ORIENTED_EDGE ( 'NONE', *, *, #29374, .T. ) ;
#50685 = EDGE_CURVE ( 'NONE', #30315, #13271, #15647, .T. ) ;
#50686 = LINE ( 'NONE', #47782, #27613 ) ;
#50687 = DIRECTION ( 'NONE',  ( -1.000000000000000000, 0.000000000000000000, 0.000000000000000000 ) ) ;
#50688 = DIRECTION ( 'NONE',  ( -0.000000000000000000, 1.000000000000000000, -0.000000000000000000 ) ) ;
#50689 = ADVANCED_FACE ( 'NONE', ( #51920 ), #35091, .T. ) ;
#50690 = EDGE_CURVE ( 'NONE', #43082, #45236, #35590, .T. ) ;
#50691 = DIRECTION ( 'NONE',  ( 0.000000000000000000, 0.000000000000000000, -1.000000000000000000 ) ) ;
#50692 = EDGE_CURVE ( 'NONE', #29039, #5201, #23275, .T. ) ;
#50693 = CARTESIAN_POINT ( 'NONE',  ( -47.53180039765466347, -177.1207230881787780, 0.3202698538628485636 ) ) ;
#50694 = VERTEX_POINT ( 'NONE', #6977 ) ;
#50695 = ADVANCED_FACE ( 'NONE', ( #39534 ), #47955, .T. ) ;
#50696 = CARTESIAN_POINT ( 'NONE',  ( 17.44316424268010834, -177.1207230881787780, -105.0256126866231483 ) ) ;
#50697 = EDGE_LOOP ( 'NONE', ( #20170, #3085 ) ) ;
#50698 = PLANE ( 'NONE',  #51880 ) ;
#50699 = ORIENTED_EDGE ( 'NONE', *, *, #24967, .T. ) ;
#50700 = EDGE_CURVE ( 'NONE', #11274, #27379, #8107, .T. ) ;
#50701 = DIRECTION ( 'NONE',  ( 0.5586467658036535777, 0.000000000000000000, -0.8294056854502011022 ) ) ;
#50702 = CIRCLE ( 'NONE', #43970, 125.0000000000000000 ) ;
#50703 = VECTOR ( 'NONE', #26032, 1000.000000000000000 ) ;
#50704 = ADVANCED_FACE ( 'NONE', ( #11688 ), #27973, .T. ) ;
#50705 = VECTOR ( 'NONE', #51981, 999.9999999999998863 ) ;
#50706 = EDGE_CURVE ( 'NONE', #49151, #25657, #26935, .T. ) ;
#50707 = CARTESIAN_POINT ( 'NONE',  ( 60.00000000000001421, 20.00000000000000000, 60.00000000000000711 ) ) ;
#50708 = DIRECTION ( 'NONE',  ( -0.2348860457809911206, 0.000000000000000000, 0.9720229140804089729 ) ) ;
#50709 = ORIENTED_EDGE ( 'NONE', *, *, #10244, .T. ) ;
#50712 = ORIENTED_EDGE ( 'NONE', *, *, #30976, .F. ) ;
#50711 = DIRECTION ( 'NONE',  ( -0.1768902751225592818, 0.000000000000000000, -0.9842305779475992722 ) ) ;
#50710 = CARTESIAN_POINT ( 'NONE',  ( -2.957822182692360080, 57.09729520864777896, -16.88242217723719918 ) ) ;
#50713 = EDGE_CURVE ( 'NONE', #37730, #20241, #369, .T. ) ;
#50714 = DIRECTION ( 'NONE',  ( 1.000000000000000000, -0.000000000000000000, -0.000000000000000000 ) ) ;
#50715 = ORIENTED_EDGE ( 'NONE', *, *, #6550, .F. ) ;
#50716 = DIRECTION ( 'NONE',  ( -1.000000000000000000, 0.000000000000000000, 0.000000000000000000 ) ) ;
#50717 = ORIENTED_EDGE ( 'NONE', *, *, #18270, .T. ) ;
#50718 = ADVANCED_FACE ( 'NONE', ( #24298 ), #32178, .F. ) ;
#50719 = CARTESIAN_POINT ( 'NONE',  ( -62.97606545226381058, -193.5000000000000000, -123.1496609813404177 ) ) ;
#50722 = ORIENTED_EDGE ( 'NONE', *, *, #46858, .F. ) ;
#50721 = CARTESIAN_POINT ( 'NONE',  ( 65.79610465833508215, -183.6283474603465606, -50.65739320401927870 ) ) ;
#50720 = CARTESIAN_POINT ( 'NONE',  ( -134.2540868116286958, -175.3837268820161057, 89.54698061029652933 ) ) ;
#50723 = AXIS2_PLACEMENT_3D ( 'NONE', #43004, #7010, #39048 ) ;
#50724 = ORIENTED_EDGE ( 'NONE', *, *, #13149, .F. ) ;
#50725 = EDGE_CURVE ( 'NONE', #32264, #49349, #50107, .T. ) ;
#50726 = EDGE_CURVE ( 'NONE', #45363, #40953, #17197, .T. ) ;
#50727 = FACE_OUTER_BOUND ( 'NONE', #9010, .T. ) ;
#50728 = VERTEX_POINT ( 'NONE', #12196 ) ;
#50729 = DIRECTION ( 'NONE',  ( 0.000000000000000000, 0.000000000000000000, 1.000000000000000000 ) ) ;
#50730 = CYLINDRICAL_SURFACE ( 'NONE', #39939, 20.00000000000001776 ) ;
#50731 = ORIENTED_EDGE ( 'NONE', *, *, #12852, .T. ) ;
#50732 = CARTESIAN_POINT ( 'NONE',  ( -155.9155026329808607, -183.6283474603465606, -61.91627321685029983 ) ) ;
#50733 = DIRECTION ( 'NONE',  ( 0.000000000000000000, 0.000000000000000000, -1.000000000000000000 ) ) ;
#50734 = CARTESIAN_POINT ( 'NONE',  ( 29.27398957514434130, -183.6283474603465606, -97.87467957287998388 ) ) ;
#50735 = DIRECTION ( 'NONE',  ( 0.000000000000000000, 1.000000000000000000, 0.000000000000000000 ) ) ;
#50736 = CARTESIAN_POINT ( 'NONE',  ( 76.48781641346532467, -193.5000000000000000, 2.874563619424060246 ) ) ;
#50737 = ORIENTED_EDGE ( 'NONE', *, *, #47229, .T. ) ;
#50738 = SHAPE_REPRESENTATION_RELATIONSHIP ( 'NONE' , 'NONE' ,  #11639, #34299 ) ;
#50739 = CYLINDRICAL_SURFACE ( 'NONE', #25458, 125.0000000000000000 ) ;
#50740 = ADVANCED_FACE ( 'NONE', ( #41102 ), #44792, .T. ) ;
#50741 = CARTESIAN_POINT ( 'NONE',  ( 33.75048693540708911, -193.5000000000000000, 94.14505102712816154 ) ) ;
#50742 = DIRECTION ( 'NONE',  ( 1.000000000000000000, 5.781354811211829468E-17, -6.525800561035010214E-17 ) ) ;
#50743 = ORIENTED_EDGE ( 'NONE', *, *, #35248, .T. ) ;
#50744 = CARTESIAN_POINT ( 'NONE',  ( -156.6671849566220089, -189.7472609257535510, 60.59166255800404599 ) ) ;
#50745 = CARTESIAN_POINT ( 'NONE',  ( 46.00000000000000711, 33.00000000000000000, -46.00000000000000000 ) ) ;
#50746 = VECTOR ( 'NONE', #32608, 1000.000000000000000 ) ;
#50747 = AXIS2_PLACEMENT_3D ( 'NONE', #21520, #16812, #41214 ) ;
#50748 = LINE ( 'NONE', #10033, #28562 ) ;
#50749 = DIRECTION ( 'NONE',  ( -1.000000000000000000, -3.701062773504881123E-15, -9.758900497077147268E-15 ) ) ;
#50750 = VERTEX_POINT ( 'NONE', #28481 ) ;
#50751 = AXIS2_PLACEMENT_3D ( 'NONE', #48737, #49527, #16935 ) ;
#50752 = DIRECTION ( 'NONE',  ( 1.000000000000000000, 0.000000000000000000, 0.000000000000000000 ) ) ;
#50753 = DIRECTION ( 'NONE',  ( 0.000000000000000000, 0.3546048870425235200, -0.9350162426854194964 ) ) ;
#50754 = CARTESIAN_POINT ( 'NONE',  ( -164.2529447963538871, -177.1207230881787780, 44.41421852208711840 ) ) ;
#50755 = CARTESIAN_POINT ( 'NONE',  ( -170.0000000000000284, -130.6726371812771959, 60.00000000000000711 ) ) ;
#50756 = VERTEX_POINT ( 'NONE', #29277 ) ;
#50757 = ADVANCED_FACE ( 'NONE', ( #44275 ), #5375, .T. ) ;
#50758 = ADVANCED_FACE ( 'NONE', ( #36906 ), #20609, .F. ) ;
#50759 = VECTOR ( 'NONE', #13222, 1000.000000000000000 ) ;
#50760 = CARTESIAN_POINT ( 'NONE',  ( 14.72514937628682574, -175.3837268820161057, -106.6827995071083848 ) ) ;
#50761 = EDGE_CURVE ( 'NONE', #46206, #28789, #32945, .T. ) ;
#50762 = EDGE_CURVE ( 'NONE', #13489, #29626, #16423, .T. ) ;
#50763 = CARTESIAN_POINT ( 'NONE',  ( -40.24578378811990831, -175.3837268820161057, 124.7285535218268251 ) ) ;
#50764 = VERTEX_POINT ( 'NONE', #28999 ) ;
#50765 = ORIENTED_EDGE ( 'NONE', *, *, #25910, .F. ) ;
#50766 = EDGE_LOOP ( 'NONE', ( #46693, #12003, #11262, #18918 ) ) ;
#50767 = LINE ( 'NONE', #3192, #693 ) ;
#50768 = LINE ( 'NONE', #38917, #21082 ) ;
#50769 = DIRECTION ( 'NONE',  ( -1.000000000000000000, 0.000000000000000000, 0.000000000000000000 ) ) ;
#50770 = EDGE_LOOP ( 'NONE', ( #42404, #34072, #45688, #23674 ) ) ;
#50771 = FACE_OUTER_BOUND ( 'NONE', #11722, .T. ) ;
#50772 = CARTESIAN_POINT ( 'NONE',  ( -166.6265240196292439, -193.5000000000000000, 40.81902153125349741 ) ) ;
#50775 = ORIENTED_EDGE ( 'NONE', *, *, #27247, .T. ) ;
#50774 = CARTESIAN_POINT ( 'NONE',  ( -339.1964088526558498, -123.5000000000000284, 0.000000000000000000 ) ) ;
#50773 = LINE ( 'NONE', #38666, #42606 ) ;
#50776 = AXIS2_PLACEMENT_3D ( 'NONE', #44516, #11219, #36630 ) ;
#50777 = EDGE_CURVE ( 'NONE', #30132, #13839, #45906, .T. ) ;
#50778 = DIRECTION ( 'NONE',  ( -0.000000000000000000, 0.3546048870425463906, 0.9350162426854107256 ) ) ;
#50779 = VECTOR ( 'NONE', #3644, 1000.000000000000000 ) ;
#50780 = ORIENTED_EDGE ( 'NONE', *, *, #49762, .F. ) ;
#50781 = DIRECTION ( 'NONE',  ( 0.000000000000000000, 1.000000000000000000, -0.000000000000000000 ) ) ;
#50782 = ORIENTED_EDGE ( 'NONE', *, *, #43262, .F. ) ;
#50783 = LINE ( 'NONE', #38930, #3099 ) ;
#50784 = CARTESIAN_POINT ( 'NONE',  ( -332.3517673607765914, -105.0395444947681369, -56.09938080879045685 ) ) ;
#50785 = CARTESIAN_POINT ( 'NONE',  ( 67.29303306501927295, -193.5000000000000000, 47.13604789772129777 ) ) ;
#50786 = EDGE_LOOP ( 'NONE', ( #33268, #2684, #2025, #5995 ) ) ;
#50787 = ADVANCED_FACE ( 'NONE', ( #37154 ), #32440, .F. ) ;
#50788 = ORIENTED_EDGE ( 'NONE', *, *, #28834, .F. ) ;
#50789 = LINE ( 'NONE', #6651, #40734 ) ;
#50790 = DIRECTION ( 'NONE',  ( -0.4031234292879730674, 0.000000000000000000, 0.9151456172430181280 ) ) ;
#50791 = ORIENTED_EDGE ( 'NONE', *, *, #39174, .T. ) ;
#50792 = CIRCLE ( 'NONE', #41544, 125.0000000000000000 ) ;
#50793 = CARTESIAN_POINT ( 'NONE',  ( -48.30901192927175458, -175.3837268820161057, -124.9998842437354227 ) ) ;
#50794 = VECTOR ( 'NONE', #20363, 1000.000000000000000 ) ;
#50795 = CARTESIAN_POINT ( 'NONE',  ( -332.3517673607765914, -182.8437365148560616, 8.849911663702917153 ) ) ;
#50796 = ORIENTED_EDGE ( 'NONE', *, *, #8348, .F. ) ;
#50797 = DIRECTION ( 'NONE',  ( 0.000000000000000000, 1.000000000000000000, 0.000000000000000000 ) ) ;
#50798 = AXIS2_PLACEMENT_3D ( 'NONE', #32325, #36812, #808 ) ;
#50799 = DIRECTION ( 'NONE',  ( 0.000000000000000000, -0.8854560256532157947, -0.4647231720437573488 ) ) ;
#50800 = AXIS2_PLACEMENT_3D ( 'NONE', #25492, #33887, #22318 ) ;
#50801 = PRODUCT_DEFINITION_SHAPE ( 'NONE', 'NONE',  #44373 ) ;
#50802 = VERTEX_POINT ( 'NONE', #12461 ) ;
#50803 = CARTESIAN_POINT ( 'NONE',  ( 60.00000000000001421, -113.5000000000000000, -40.00000000000001421 ) ) ;
#50804 = EDGE_LOOP ( 'NONE', ( #42892, #5933, #20493, #4532 ) ) ;
#50805 = CARTESIAN_POINT ( 'NONE',  ( 0.000000000000000000, -180.7855672281370119, 14.11962419296635396 ) ) ;
#50806 = DIRECTION ( 'NONE',  ( -0.000000000000000000, 1.000000000000000000, 0.000000000000000000 ) ) ;
#50807 = ORIENTED_EDGE ( 'NONE', *, *, #28215, .T. ) ;
#50808 = PLANE ( 'NONE',  #13463 ) ;
#50809 = DIRECTION ( 'NONE',  ( -0.9960498426152177842, 0.000000000000000000, 0.08879589532292482545 ) ) ;
#50810 = CARTESIAN_POINT ( 'NONE',  ( -126.2322430781613605, -193.5000000000000000, 97.87467957288053810 ) ) ;
#50811 = EDGE_CURVE ( 'NONE', #19283, #40712, #31623, .T. ) ;
#50812 = ORIENTED_EDGE ( 'NONE', *, *, #6757, .T. ) ;
#50813 = PLANE ( 'NONE',  #16175 ) ;
#50814 = VECTOR ( 'NONE', #19751, 1000.000000000000000 ) ;
#50815 = DIRECTION ( 'NONE',  ( 0.000000000000000000, 1.000000000000000000, 0.000000000000000000 ) ) ;
#50816 = DIRECTION ( 'NONE',  ( -0.000000000000000000, 1.000000000000000000, 0.000000000000000000 ) ) ;
#50818 = ORIENTED_EDGE ( 'NONE', *, *, #50360, .F. ) ;
#50817 = CYLINDRICAL_SURFACE ( 'NONE', #48859, 125.0000000000000000 ) ;
#50819 = AXIS2_PLACEMENT_3D ( 'NONE', #30538, #15057, #26854 ) ;
#50820 = VECTOR ( 'NONE', #26045, 1000.000000000000114 ) ;
#50821 = VERTEX_POINT ( 'NONE', #16694 ) ;
#50822 = EDGE_CURVE ( 'NONE', #29368, #32936, #33326, .T. ) ;
#50823 = EDGE_CURVE ( 'NONE', #41662, #46894, #41351, .T. ) ;
#50824 = PLANE ( 'NONE',  #40854 ) ;
#50825 = AXIS2_PLACEMENT_3D ( 'NONE', #38764, #3030, #42457 ) ;
#50826 = DIRECTION ( 'NONE',  ( 0.000000000000000000, -1.000000000000000000, 0.000000000000000000 ) ) ;
#50827 = ORIENTED_EDGE ( 'NONE', *, *, #15792, .F. ) ;
#50828 = DIRECTION ( 'NONE',  ( 0.000000000000000000, -6.753856733136369375E-14, -1.000000000000000000 ) ) ;
#50829 = CIRCLE ( 'NONE', #34005, 125.0000000000000000 ) ;
#50830 = ORIENTED_EDGE ( 'NONE', *, *, #32711, .T. ) ;
#50831 = CARTESIAN_POINT ( 'NONE',  ( -330.4913330509368166, -73.83865025250280212, 33.67120938215256132 ) ) ;
#50832 = CARTESIAN_POINT ( 'NONE',  ( 5.761208793373444359E-16, 50.59471834446340921, -21.36672353920344491 ) ) ;
#50833 = AXIS2_PLACEMENT_3D ( 'NONE', #44949, #21025, #16577 ) ;
#50835 = VECTOR ( 'NONE', #44966, 1000.000000000000000 ) ;
#50834 = DIRECTION ( 'NONE',  ( -0.9890401873221654760, 0.000000000000000000, 0.1476465640024710868 ) ) ;
#50836 = LINE ( 'NONE', #1704, #19060 ) ;
#50837 = ORIENTED_EDGE ( 'NONE', *, *, #51268, .F. ) ;
#50838 = VERTEX_POINT ( 'NONE', #25335 ) ;
#50839 = ORIENTED_EDGE ( 'NONE', *, *, #13135, .T. ) ;
#50840 = CIRCLE ( 'NONE', #31534, 125.0000000000000000 ) ;
#50841 = DIRECTION ( 'NONE',  ( -0.000000000000000000, 1.000000000000000000, -0.000000000000000000 ) ) ;
#50842 = DIRECTION ( 'NONE',  ( 0.000000000000000000, 0.000000000000000000, -1.000000000000000000 ) ) ;
#50843 = CARTESIAN_POINT ( 'NONE',  ( 141.7825277784304205, -193.5000000000000000, -41.45482488023466061 ) ) ;
#50844 = EDGE_CURVE ( 'NONE', #39155, #3968, #37414, .T. ) ;
#50845 = DIRECTION ( 'NONE',  ( 0.000000000000000000, -0.000000000000000000, 1.000000000000000000 ) ) ;
#50846 = CARTESIAN_POINT ( 'NONE',  ( -74.51199343215195370, -183.6283474603465606, -122.2591094863195025 ) ) ;
#50847 = ORIENTED_EDGE ( 'NONE', *, *, #27253, .T. ) ;
#50848 = DIRECTION ( 'NONE',  ( -0.000000000000000000, 1.000000000000000000, -0.000000000000000000 ) ) ;
#50849 = CARTESIAN_POINT ( 'NONE',  ( 20.66186849114819069, -189.7472609257535510, -104.1370384486465070 ) ) ;
#50850 = EDGE_CURVE ( 'NONE', #18822, #15614, #13510, .T. ) ;
#50851 = ORIENTED_EDGE ( 'NONE', *, *, #45847, .T. ) ;
#50852 = ORIENTED_EDGE ( 'NONE', *, *, #36982, .F. ) ;
#50853 = FACE_OUTER_BOUND ( 'NONE', #51272, .T. ) ;
#50854 = VECTOR ( 'NONE', #25463, 1000.000000000000000 ) ;
#50855 = CARTESIAN_POINT ( 'NONE',  ( 73.87536152799695799, -189.7472609257535510, -25.58083653558412252 ) ) ;
#50856 = CARTESIAN_POINT ( 'NONE',  ( -28.74596282265200387, -177.1207230881787780, 123.4325817657431230 ) ) ;
#50857 = CARTESIAN_POINT ( 'NONE',  ( -330.4913330509368166, -124.0000000000001990, -59.00000000000002132 ) ) ;
#50858 = VECTOR ( 'NONE', #32866, 1000.000000000000000 ) ;
#50859 = VECTOR ( 'NONE', #46595, 1000.000000000000114 ) ;
#50860 = CARTESIAN_POINT ( 'NONE',  ( -155.9608607592037401, -183.6283474603465606, 63.81752780153057358 ) ) ;
#50861 = LINE ( 'NONE', #14868, #50316 ) ;
#50862 = EDGE_LOOP ( 'NONE', ( #13000, #1215, #49371, #8803 ) ) ;
#50864 = ADVANCED_FACE ( 'NONE', ( #5644 ), #10795, .T. ) ;
#50863 = DIRECTION ( 'NONE',  ( -0.000000000000000000, -0.7485107481710977506, 0.6631226582407989678 ) ) ;
#50865 = ORIENTED_EDGE ( 'NONE', *, *, #35449, .F. ) ;
#50866 = CARTESIAN_POINT ( 'NONE',  ( -23.01747912075234836, -193.5000000000000000, -122.3793467049370634 ) ) ;
#50867 = CARTESIAN_POINT ( 'NONE',  ( -49.03777351731249468, -189.7472609257535510, -0.8294056854502022125 ) ) ;
#50868 = EDGE_LOOP ( 'NONE', ( #21042, #40487, #22615, #40744 ) ) ;
#50869 = VECTOR ( 'NONE', #25088, 1000.000000000000114 ) ;
#50870 = DIRECTION ( 'NONE',  ( 0.000000000000000000, -0.000000000000000000, 1.000000000000000000 ) ) ;
#50871 = DIRECTION ( 'NONE',  ( 0.1768902751225733261, 0.000000000000000000, -0.9842305779475966077 ) ) ;
#50872 = CARTESIAN_POINT ( 'NONE',  ( -332.3517673607765914, -158.9146170832377720, -48.43351006119259949 ) ) ;
#50873 = VECTOR ( 'NONE', #32864, 1000.000000000000114 ) ;
#50874 = CARTESIAN_POINT ( 'NONE',  ( -48.47912675150885065, -183.6283474603465606, 6.938893903907228378E-15 ) ) ;
#50875 = EDGE_CURVE ( 'NONE', #22314, #27143, #5900, .T. ) ;
#50877 = AXIS2_PLACEMENT_3D ( 'NONE', #3541, #19827, #22746 ) ;
#50876 = CARTESIAN_POINT ( 'NONE',  ( -339.1964088526558498, -90.39567187580801999, 48.84008046109089918 ) ) ;
#50878 = VERTEX_POINT ( 'NONE', #41612 ) ;
#50879 = CARTESIAN_POINT ( 'NONE',  ( -129.5578577291867646, -193.5000000000000000, 93.82025162278056030 ) ) ;
#50881 = ORIENTED_EDGE ( 'NONE', *, *, #10270, .F. ) ;
#50880 = LINE ( 'NONE', #23009, #969 ) ;
#50882 = ORIENTED_EDGE ( 'NONE', *, *, #40003, .T. ) ;
#50883 = PLANE ( 'NONE',  #46457 ) ;
#50884 = EDGE_CURVE ( 'NONE', #47574, #34020, #1939, .T. ) ;
#50885 = VERTEX_POINT ( 'NONE', #9831 ) ;
#50886 = DIRECTION ( 'NONE',  ( 0.6749830015182038956, 0.000000000000000000, 0.7378332790417333475 ) ) ;
#50887 = EDGE_CURVE ( 'NONE', #23810, #9413, #3913, .T. ) ;
#50888 = AXIS2_PLACEMENT_3D ( 'NONE', #17532, #33281, #24878 ) ;
#50889 = VECTOR ( 'NONE', #7038, 1000.000000000000114 ) ;
#50890 = VERTEX_POINT ( 'NONE', #37686 ) ;
#50891 = DIRECTION ( 'NONE',  ( 0.000000000000000000, -0.000000000000000000, -1.000000000000000000 ) ) ;
#50892 = PLANE ( 'NONE',  #38022 ) ;
#50893 = EDGE_LOOP ( 'NONE', ( #47372, #32079, #30883, #34650 ) ) ;
#50894 = LINE ( 'NONE', #43245, #17415 ) ;
#50895 = AXIS2_PLACEMENT_3D ( 'NONE', #12899, #5038, #11019 ) ;
#50896 = AXIS2_PLACEMENT_3D ( 'NONE', #40438, #20224, #35727 ) ;
#50897 = ADVANCED_FACE ( 'NONE', ( #50037 ), #18936, .T. ) ;
#50898 = LINE ( 'NONE', #11440, #21053 ) ;
#50899 = CARTESIAN_POINT ( 'NONE',  ( -172.9089226952081901, -175.3837268820161057, 11.92584929509617986 ) ) ;
#50900 = ORIENTED_EDGE ( 'NONE', *, *, #43803, .F. ) ;
#50901 = ORIENTED_EDGE ( 'NONE', *, *, #10035, .T. ) ;
#50902 = ORIENTED_EDGE ( 'NONE', *, *, #21951, .T. ) ;
#50903 = CARTESIAN_POINT ( 'NONE',  ( -336.3521761649654422, -119.0014323656137947, -58.88711093124865670 ) ) ;
#50904 = FACE_OUTER_BOUND ( 'NONE', #3629, .T. ) ;
#50905 = AXIS2_PLACEMENT_3D ( 'NONE', #19557, #39275, #3281 ) ;
#50906 = AXIS2_PLACEMENT_3D ( 'NONE', #12638, #3992, #44191 ) ;
#50907 = EDGE_CURVE ( 'NONE', #28554, #8596, #17364, .T. ) ;
#50908 =( NAMED_UNIT ( * ) PLANE_ANGLE_UNIT ( ) SI_UNIT ( $, .RADIAN. ) );
#50909 = AXIS2_PLACEMENT_3D ( 'NONE', #2338, #14172, #5509 ) ;
#50911 = AXIS2_PLACEMENT_3D ( 'NONE', #18356, #26741, #34374 ) ;
#50910 = DIRECTION ( 'NONE',  ( -0.000000000000000000, 1.000000000000000000, -0.000000000000000000 ) ) ;
#50912 = DIRECTION ( 'NONE',  ( -0.000000000000000000, 0.9709418174260519008, -0.2393156642875582940 ) ) ;
#50913 = ORIENTED_EDGE ( 'NONE', *, *, #27009, .F. ) ;
#50914 = AXIS2_PLACEMENT_3D ( 'NONE', #34930, #31783, #31249 ) ;
#50915 = FACE_OUTER_BOUND ( 'NONE', #9445, .T. ) ;
#50916 = ORIENTED_EDGE ( 'NONE', *, *, #38870, .T. ) ;
#50918 = VERTEX_POINT ( 'NONE', #49782 ) ;
#50917 = PLANE ( 'NONE',  #37380 ) ;
#50919 = EDGE_LOOP ( 'NONE', ( #11310, #18741, #16229, #2479 ) ) ;
#50920 = DIRECTION ( 'NONE',  ( 0.000000000000000000, -1.000000000000000000, -0.000000000000000000 ) ) ;
#50921 = CARTESIAN_POINT ( 'NONE',  ( -172.9089226952081617, -189.7472609257535510, 11.92584929509620117 ) ) ;
#50922 = PLANE ( 'NONE',  #4508 ) ;
#50923 = CARTESIAN_POINT ( 'NONE',  ( -65.65563056894596627, -177.1207230881787780, 123.8142468240612999 ) ) ;
#50924 = ORIENTED_EDGE ( 'NONE', *, *, #22051, .T. ) ;
#50925 = CARTESIAN_POINT ( 'NONE',  ( -48.47912675150885065, -117.5479369270332057, 6.938893903907228378E-15 ) ) ;
#50926 = ORIENTED_EDGE ( 'NONE', *, *, #22122, .F. ) ;
#50927 = VERTEX_POINT ( 'NONE', #27063 ) ;
#50928 = FACE_OUTER_BOUND ( 'NONE', #9565, .T. ) ;
#50929 = VECTOR ( 'NONE', #14038, 1000.000000000000000 ) ;
#50930 = PLANE ( 'NONE',  #2104 ) ;
#50931 = AXIS2_PLACEMENT_3D ( 'NONE', #8456, #4010, #20542 ) ;
#50932 = DIRECTION ( 'NONE',  ( -0.000000000000000000, 1.000000000000000000, -0.000000000000000000 ) ) ;
#50933 = DIRECTION ( 'NONE',  ( -0.000000000000000000, -1.000000000000000000, 0.000000000000000000 ) ) ;
#50934 = ORIENTED_EDGE ( 'NONE', *, *, #10158, .T. ) ;
#50935 = CARTESIAN_POINT ( 'NONE',  ( -180.0000000000000568, -130.6726371812771959, -60.00000000000000711 ) ) ;
#50936 = CYLINDRICAL_SURFACE ( 'NONE', #41534, 125.0000000000000000 ) ;
#50937 = VECTOR ( 'NONE', #19189, 1000.000000000000000 ) ;
#50938 = EDGE_CURVE ( 'NONE', #5668, #45033, #14010, .T. ) ;
#50939 = EDGE_CURVE ( 'NONE', #18052, #7546, #33988, .T. ) ;
#50940 = CARTESIAN_POINT ( 'NONE',  ( -154.5708152632604708, -193.5000000000000000, 64.19309449102807719 ) ) ;
#50941 = LINE ( 'NONE', #14942, #25406 ) ;
#50942 = ORIENTED_EDGE ( 'NONE', *, *, #44753, .T. ) ;
#50943 = DIRECTION ( 'NONE',  ( 0.9266896074318317078, 0.000000000000000000, 0.3758275821142421647 ) ) ;
#50944 = FACE_OUTER_BOUND ( 'NONE', #22565, .T. ) ;
#50945 = DIRECTION ( 'NONE',  ( 0.000000000000000000, 0.000000000000000000, -1.000000000000000000 ) ) ;
#50946 = ORIENTED_EDGE ( 'NONE', *, *, #31699, .T. ) ;
#50947 = CIRCLE ( 'NONE', #30778, 125.0000000000000000 ) ;
#50948 = AXIS2_PLACEMENT_3D ( 'NONE', #17651, #9238, #26034 ) ;
#50949 = CARTESIAN_POINT ( 'NONE',  ( -336.3521761649654422, -92.15051119686104641, -50.05135858667769355 ) ) ;
#50950 = AXIS2_PLACEMENT_3D ( 'NONE', #9540, #37657, #18209 ) ;
#50951 = AXIS2_PLACEMENT_3D ( 'NONE', #27380, #43432, #15310 ) ;
#50952 = CARTESIAN_POINT ( 'NONE',  ( -153.7332855749581881, -193.5000000000000000, 67.42819922234390617 ) ) ;
#50953 = ORIENTED_EDGE ( 'NONE', *, *, #3102, .T. ) ;
#50954 = PLANE ( 'NONE',  #9467 ) ;
#50955 = EDGE_CURVE ( 'NONE', #31330, #6494, #43104, .T. ) ;
#50956 = VECTOR ( 'NONE', #43520, 1000.000000000000000 ) ;
#50957 = ORIENTED_EDGE ( 'NONE', *, *, #47509, .T. ) ;
#50958 = EDGE_CURVE ( 'NONE', #44532, #38288, #37939, .T. ) ;
#50959 = VECTOR ( 'NONE', #13169, 1000.000000000000114 ) ;
#50960 = CARTESIAN_POINT ( 'NONE',  ( -332.3517673607765914, -93.75055682584159911, 51.01861988938794923 ) ) ;
#50961 = EDGE_CURVE ( 'NONE', #13339, #29051, #25582, .T. ) ;
#50962 = FACE_BOUND ( 'NONE', #26902, .T. ) ;
#50963 = PLANE ( 'NONE',  #18722 ) ;
#50964 = DIRECTION ( 'NONE',  ( 0.9266896074318343723, 0.000000000000000000, -0.3758275821142357809 ) ) ;
#50965 = ORIENTED_EDGE ( 'NONE', *, *, #1293, .F. ) ;
#50966 = VERTEX_POINT ( 'NONE', #30760 ) ;
#50967 = CARTESIAN_POINT ( 'NONE',  ( -336.3521761649654422, -145.9479049231020440, -54.58714071513102795 ) ) ;
#50968 = AXIS2_PLACEMENT_3D ( 'NONE', #11729, #16738, #3855 ) ;
#50969 = AXIS2_PLACEMENT_3D ( 'NONE', #51853, #22109, #25275 ) ;
#50970 = VERTEX_POINT ( 'NONE', #33737 ) ;
#50971 = DIRECTION ( 'NONE',  ( -0.1182731709213592358, 0.000000000000000000, -0.9929810960135178055 ) ) ;
#50972 = VECTOR ( 'NONE', #28168, 1000.000000000000000 ) ;
#50973 = DIRECTION ( 'NONE',  ( -0.000000000000000000, 1.000000000000000000, 0.000000000000000000 ) ) ;
#50974 = CARTESIAN_POINT ( 'NONE',  ( -19.92568551777507224, -189.7472609257535510, -121.6951149130962904 ) ) ;
#50975 = VERTEX_POINT ( 'NONE', #25856 ) ;
#50978 = ORIENTED_EDGE ( 'NONE', *, *, #4506, .T. ) ;
#50977 = CARTESIAN_POINT ( 'NONE',  ( -49.17567778057184569, -189.7472609257535510, -0.7175072570443327136 ) ) ;
#50976 = CARTESIAN_POINT ( 'NONE',  ( -4.434052336286734786, 54.62761619819747949, -18.21243447522283532 ) ) ;
#50979 = VECTOR ( 'NONE', #27156, 1000.000000000000000 ) ;
#50980 = VECTOR ( 'NONE', #40531, 1000.000000000000000 ) ;
#50981 = CIRCLE ( 'NONE', #24122, 125.0000000000000000 ) ;
#50982 = CARTESIAN_POINT ( 'NONE',  ( -161.6832731452239784, -193.5000000000000000, -53.00774697410100345 ) ) ;
#50983 = ORIENTED_EDGE ( 'NONE', *, *, #8758, .T. ) ;
#50984 = DIRECTION ( 'NONE',  ( 0.000000000000000000, -1.000000000000000000, 0.000000000000000000 ) ) ;
#50985 = ORIENTED_EDGE ( 'NONE', *, *, #33184, .F. ) ;
#50986 = AXIS2_PLACEMENT_3D ( 'NONE', #5073, #40789, #17434 ) ;
#50987 = DIRECTION ( 'NONE',  ( -0.000000000000000000, 1.000000000000000000, -0.000000000000000000 ) ) ;
#50988 = EDGE_LOOP ( 'NONE', ( #22764, #31434, #26472, #18735 ) ) ;
#50991 = VERTEX_POINT ( 'NONE', #22878 ) ;
#50990 = DIRECTION ( 'NONE',  ( 0.000000000000000000, -0.9350162426854169428, -0.3546048870425300148 ) ) ;
#50989 = FACE_OUTER_BOUND ( 'NONE', #12745, .T. ) ;
#50992 = VERTEX_POINT ( 'NONE', #33492 ) ;
#50993 = CIRCLE ( 'NONE', #30835, 125.0000000000000000 ) ;
#50994 = DIRECTION ( 'NONE',  ( 0.000000000000000000, 0.000000000000000000, -1.000000000000000000 ) ) ;
#50995 = ORIENTED_EDGE ( 'NONE', *, *, #46373, .T. ) ;
#50996 = LINE ( 'NONE', #6066, #38753 ) ;
#50997 = CARTESIAN_POINT ( 'NONE',  ( -49.29161362951453640, -189.7472609257535510, 0.5829794791144718991 ) ) ;
#50998 = ORIENTED_EDGE ( 'NONE', *, *, #11520, .T. ) ;
#50999 = FACE_OUTER_BOUND ( 'NONE', #34154, .T. ) ;
#51000 = FACE_OUTER_BOUND ( 'NONE', #2882, .T. ) ;
#51001 = PLANE ( 'NONE',  #10641 ) ;
#51002 = CARTESIAN_POINT ( 'NONE',  ( -365.0000000000001137, -168.5000000000000284, 0.000000000000000000 ) ) ;
#51003 = EDGE_CURVE ( 'NONE', #30945, #9782, #46722, .T. ) ;
#51004 = EDGE_CURVE ( 'NONE', #13064, #46003, #50150, .T. ) ;
#51005 = VERTEX_POINT ( 'NONE', #14145 ) ;
#51006 = EDGE_CURVE ( 'NONE', #36852, #20677, #5616, .T. ) ;
#51007 =( LENGTH_UNIT ( ) NAMED_UNIT ( * ) SI_UNIT ( .MILLI., .METRE. ) );
#51008 = CARTESIAN_POINT ( 'NONE',  ( -47.47956591500005885, -193.5000000000000000, 0.02963332782257025594 ) ) ;
#51009 = CARTESIAN_POINT ( 'NONE',  ( -339.1964088526558498, -66.09477493971894546, 13.63415328425207917 ) ) ;
#51010 = EDGE_CURVE ( 'NONE', #21717, #1947, #32609, .T. ) ;
#51011 = CARTESIAN_POINT ( 'NONE',  ( -135.6699833737243353, -175.3837268820161057, 89.56983042009328244 ) ) ;
#51012 = ORIENTED_EDGE ( 'NONE', *, *, #40249, .T. ) ;
#51013 = TOROIDAL_SURFACE ( 'NONE', #50187, 1.951623109906645004, 10.00000000000000000 ) ;
#51014 = AXIS2_PLACEMENT_3D ( 'NONE', #8381, #28341, #17061 ) ;
#51015 = CARTESIAN_POINT ( 'NONE',  ( -92.16375985330358844, -189.7472609257535510, 117.1181148702521710 ) ) ;
#51016 = ADVANCED_FACE ( 'NONE', ( #20784 ), #37063, .T. ) ;
#51017 = CARTESIAN_POINT ( 'NONE',  ( -48.47912675150885065, -175.3837268820161057, 6.938893903907228378E-15 ) ) ;
#51018 = ADVANCED_FACE ( 'NONE', ( #40476 ), #16596, .F. ) ;
#51020 = CIRCLE ( 'NONE', #33372, 125.0000000000000000 ) ;
#51019 = DIRECTION ( 'NONE',  ( -0.000000000000000000, 1.000000000000000000, -0.000000000000000000 ) ) ;
#51021 = CARTESIAN_POINT ( 'NONE',  ( -305.0000000000000568, -70.60684477890951882, 28.32515014536777187 ) ) ;
#51022 = DIRECTION ( 'NONE',  ( 0.000000000000000000, 0.000000000000000000, 1.000000000000000000 ) ) ;
#51023 = VERTEX_POINT ( 'NONE', #49169 ) ;
#51024 = EDGE_CURVE ( 'NONE', #21423, #51701, #12368, .T. ) ;
#51025 = EDGE_CURVE ( 'NONE', #16663, #5355, #45238, .T. ) ;
#51026 = ADVANCED_FACE ( 'NONE', ( #34360 ), #34098, .T. ) ;
#51027 = AXIS2_PLACEMENT_3D ( 'NONE', #38205, #2214, #19026 ) ;
#51028 = DIRECTION ( 'NONE',  ( 0.000000000000000000, 0.000000000000000000, -1.000000000000000000 ) ) ;
#51029 = EDGE_CURVE ( 'NONE', #14630, #23392, #44443, .T. ) ;
#51030 = DIRECTION ( 'NONE',  ( -0.000000000000000000, 0.2393156642875685636, 0.9709418174260492362 ) ) ;
#51031 = DIRECTION ( 'NONE',  ( -0.9266896074318317078, 0.000000000000000000, -0.3758275821142421647 ) ) ;
#51032 = CARTESIAN_POINT ( 'NONE',  ( -339.1964088526558498, -75.22798428563991990, -33.92731199008514409 ) ) ;
#51033 = AXIS2_PLACEMENT_3D ( 'NONE', #31641, #43988, #51898 ) ;
#51034 = EDGE_CURVE ( 'NONE', #1472, #44801, #48656, .T. ) ;
#51035 = ORIENTED_EDGE ( 'NONE', *, *, #3115, .F. ) ;
#51036 = DIRECTION ( 'NONE',  ( -1.000000000000000000, 0.000000000000000000, 0.000000000000000000 ) ) ;
#51037 = CIRCLE ( 'NONE', #17463, 125.0000000000000000 ) ;
#51038 = DIRECTION ( 'NONE',  ( 0.000000000000000000, 0.000000000000000000, -1.000000000000000000 ) ) ;
#51039 = EDGE_LOOP ( 'NONE', ( #44455, #1184, #19671, #29754 ) ) ;
#51040 = VERTEX_POINT ( 'NONE', #16855 ) ;
#51041 = ORIENTED_EDGE ( 'NONE', *, *, #35748, .F. ) ;
#51042 = CARTESIAN_POINT ( 'NONE',  ( -339.1964088526558498, -103.0458197858333165, -55.34326076196084188 ) ) ;
#51043 = CARTESIAN_POINT ( 'NONE',  ( -37.67038537088847505, -183.6283474603465606, -124.5318076226586470 ) ) ;
#51044 = VERTEX_POINT ( 'NONE', #38029 ) ;
#51045 = EDGE_CURVE ( 'NONE', #27304, #4539, #44970, .T. ) ;
#51046 = PLANE ( 'NONE',  #11598 ) ;
#51047 = DIRECTION ( 'NONE',  ( 0.000000000000000000, -1.000000000000000000, 0.000000000000000000 ) ) ;
#51050 = ORIENTED_EDGE ( 'NONE', *, *, #16, .F. ) ;
#51049 = CARTESIAN_POINT ( 'NONE',  ( -339.1964088526558498, -172.3400804610915600, -33.10432812419107051 ) ) ;
#51048 = DIRECTION ( 'NONE',  ( 0.000000000000000000, 1.000000000000000000, 0.000000000000000000 ) ) ;
#51051 = AXIS2_PLACEMENT_3D ( 'NONE', #49573, #34045, #38236 ) ;
#51052 = CARTESIAN_POINT ( 'NONE',  ( -170.0000000000000284, -113.5000000000000142, -60.00000000000001421 ) ) ;
#51053 = EDGE_LOOP ( 'NONE', ( #6802, #19091, #21648, #35736 ) ) ;
#51054 = CARTESIAN_POINT ( 'NONE',  ( -136.1415351158078693, -189.7472609257535510, -89.10837311819173578 ) ) ;
#51055 = VECTOR ( 'NONE', #16370, 1000.000000000000000 ) ;
#51056 = EDGE_LOOP ( 'NONE', ( #51748, #45050, #15542, #2720 ) ) ;
#51057 = FACE_OUTER_BOUND ( 'NONE', #41719, .T. ) ;
#51058 = CYLINDRICAL_SURFACE ( 'NONE', #18756, 125.0000000000000000 ) ;
#51060 = CARTESIAN_POINT ( 'NONE',  ( -49.35486169370449971, -193.5000000000000000, 0.4827922027307437469 ) ) ;
#51059 = CARTESIAN_POINT ( 'NONE',  ( -70.75782287548091176, -175.3837268820161057, 122.9986166548864901 ) ) ;
#51061 = ORIENTED_EDGE ( 'NONE', *, *, #31542, .T. ) ;
#51062 = ADVANCED_FACE ( 'NONE', ( #2308 ), #21303, .F. ) ;
#51063 = AXIS2_PLACEMENT_3D ( 'NONE', #51344, #5010, #27675 ) ;
#51064 = EDGE_LOOP ( 'NONE', ( #44761, #47424, #23980, #46072 ) ) ;
#51065 = DIRECTION ( 'NONE',  ( 0.000000000000000000, 0.000000000000000000, 1.000000000000000000 ) ) ;
#51066 = DIRECTION ( 'NONE',  ( -0.000000000000000000, 1.000000000000000000, -0.000000000000000000 ) ) ;
#51067 = ORIENTED_EDGE ( 'NONE', *, *, #43483, .T. ) ;
#51068 = CARTESIAN_POINT ( 'NONE',  ( -97.70585564814136603, -193.5000000000000000, 113.8100815915419304 ) ) ;
#51069 = CARTESIAN_POINT ( 'NONE',  ( 66.11593792271145276, -189.7472609257535510, -47.37063079638321739 ) ) ;
#51070 = EDGE_CURVE ( 'NONE', #20987, #47304, #41005, .T. ) ;
#51071 = EDGE_CURVE ( 'NONE', #18280, #40458, #7331, .T. ) ;
#51072 = ORIENTED_EDGE ( 'NONE', *, *, #50308, .F. ) ;
#51073 = ADVANCED_FACE ( 'NONE', ( #44699 ), #18344, .F. ) ;
#51074 = CARTESIAN_POINT ( 'NONE',  ( 58.45385938022560168, -183.6283474603465606, 62.78108192022013867 ) ) ;
#51075 = CARTESIAN_POINT ( 'NONE',  ( -330.4913330509368166, -64.86990808808717190, -6.615309698015095385 ) ) ;
#51076 = EDGE_CURVE ( 'NONE', #36064, #28789, #42229, .T. ) ;
#51077 = VECTOR ( 'NONE', #9738, 1000.000000000000000 ) ;
#51078 = VERTEX_POINT ( 'NONE', #20512 ) ;
#51079 = CARTESIAN_POINT ( 'NONE',  ( -332.3517673607765914, -176.5004679656469477, -25.97334715265976612 ) ) ;
#51080 = ORIENTED_EDGE ( 'NONE', *, *, #39749, .T. ) ;
#51081 = CARTESIAN_POINT ( 'NONE',  ( -340.0000000000000568, -78.50000000000002842, -5.000000000000001776 ) ) ;
#51082 = EDGE_CURVE ( 'NONE', #32088, #38087, #8148, .T. ) ;
#51083 = CARTESIAN_POINT ( 'NONE',  ( -49.29161362951452929, -177.1207230881787780, -0.5829794791144748967 ) ) ;
#51084 = EDGE_LOOP ( 'NONE', ( #6783, #35959, #9399, #40517 ) ) ;
#51085 = CARTESIAN_POINT ( 'NONE',  ( -60.00000000000000000, 0.000000000000000000, -60.00000000000000711 ) ) ;
#51086 = LINE ( 'NONE', #30556, #41499 ) ;
#51087 = DIRECTION ( 'NONE',  ( -0.000000000000000000, 1.000000000000000000, -0.000000000000000000 ) ) ;
#51088 = ADVANCED_FACE ( 'NONE', ( #7540 ), #42495, .F. ) ;
#51089 = VERTEX_POINT ( 'NONE', #14647 ) ;
#51090 = DIRECTION ( 'NONE',  ( 0.000000000000000000, -0.000000000000000000, -1.000000000000000000 ) ) ;
#51091 = AXIS2_PLACEMENT_3D ( 'NONE', #28083, #27585, #43864 ) ;
#51092 = AXIS2_PLACEMENT_3D ( 'NONE', #16989, #2755, #47176 ) ;
#51093 = EDGE_CURVE ( 'NONE', #22006, #34216, #35869, .T. ) ;
#51094 = VECTOR ( 'NONE', #12293, 1000.000000000000000 ) ;
#51095 = DIRECTION ( 'NONE',  ( 0.000000000000000000, 0.000000000000000000, 1.000000000000000000 ) ) ;
#51096 = CARTESIAN_POINT ( 'NONE',  ( -49.46816693883101124, -175.3837268820161057, -0.1476465640024848536 ) ) ;
#51098 = ORIENTED_EDGE ( 'NONE', *, *, #8991, .T. ) ;
#51097 = CARTESIAN_POINT ( 'NONE',  ( -339.1964088526558498, -123.0000000000002700, -59.00000000000002132 ) ) ;
#51099 = CIRCLE ( 'NONE', #19188, 125.0000000000000000 ) ;
#51100 = EDGE_CURVE ( 'NONE', #42455, #21438, #31438, .T. ) ;
#51101 = EDGE_LOOP ( 'NONE', ( #16260, #2255, #21347, #7652 ) ) ;
#51102 = CARTESIAN_POINT ( 'NONE',  ( 58.95724912996274725, -193.5000000000000000, 61.91627321685103880 ) ) ;
#51103 = EDGE_CURVE ( 'NONE', #39243, #9591, #47482, .T. ) ;
#51104 = DIRECTION ( 'NONE',  ( 0.000000000000000000, 1.000000000000000000, 0.000000000000000000 ) ) ;
#51105 = ORIENTED_EDGE ( 'NONE', *, *, #15462, .T. ) ;
#51106 = AXIS2_PLACEMENT_3D ( 'NONE', #47220, #2792, #46694 ) ;
#51107 = VERTEX_POINT ( 'NONE', #11209 ) ;
#51108 = CARTESIAN_POINT ( 'NONE',  ( -336.3521761649654422, -181.1761995186066088, -12.53476669029101842 ) ) ;
#51109 = EDGE_LOOP ( 'NONE', ( #5564, #14230, #1232, #25845 ) ) ;
#51110 = CARTESIAN_POINT ( 'NONE',  ( -332.3517673607765914, -182.3871109312487420, -4.498567634386014369 ) ) ;
#51111 = CARTESIAN_POINT ( 'NONE',  ( 62.13187335169531167, -193.5000000000000000, -58.22548115875872554 ) ) ;
#51112 = DIRECTION ( 'NONE',  ( -0.000000000000000000, -1.000000000000000000, -0.000000000000000000 ) ) ;
#51113 = LINE ( 'NONE', #48177, #23266 ) ;
#51114 = ORIENTED_EDGE ( 'NONE', *, *, #27684, .F. ) ;
#51115 = EDGE_LOOP ( 'NONE', ( #13836, #14844, #3950, #3654 ) ) ;
#51116 = ORIENTED_EDGE ( 'NONE', *, *, #40074, .T. ) ;
#51117 = VECTOR ( 'NONE', #23050, 1000.000000000000000 ) ;
#51118 = EDGE_CURVE ( 'NONE', #35424, #25619, #43269, .T. ) ;
#51119 = LINE ( 'NONE', #47156, #50979 ) ;
#51120 = CARTESIAN_POINT ( 'NONE',  ( -121.5885020763900854, -183.6283474603465606, -101.3904297239421055 ) ) ;
#51121 = DIRECTION ( 'NONE',  ( -0.000000000000000000, 0.2393156642875582940, 0.9709418174260519008 ) ) ;
#51122 = CARTESIAN_POINT ( 'NONE',  ( -99.62791064391784346, -175.3837268820161057, -114.0561348912352173 ) ) ;
#51123 = CARTESIAN_POINT ( 'NONE',  ( -48.88225018079683082, -189.7472609257535510, 0.9151456172430223468 ) ) ;
#51124 = ORIENTED_EDGE ( 'NONE', *, *, #19417, .T. ) ;
#51125 = CARTESIAN_POINT ( 'NONE',  ( -48.47912675150885065, -183.6283474603465606, 6.938893903907228378E-15 ) ) ;
#51126 = CARTESIAN_POINT ( 'NONE',  ( 52.75081385575904136, -175.3837268820161057, 71.61357856150601719 ) ) ;
#51127 = ORIENTED_EDGE ( 'NONE', *, *, #39475, .T. ) ;
#51128 = ORIENTED_EDGE ( 'NONE', *, *, #22174, .T. ) ;
#51129 = AXIS2_PLACEMENT_3D ( 'NONE', #28410, #43927, #8446 ) ;
#51130 = LINE ( 'NONE', #18017, #34057 ) ;
#51131 = CARTESIAN_POINT ( 'NONE',  ( -59.86929868745821182, -193.5000000000000000, -124.4799742258549600 ) ) ;
#51133 = AXIS2_PLACEMENT_3D ( 'NONE', #51725, #34892, #42533 ) ;
#51132 = DIRECTION ( 'NONE',  ( 0.000000000000000000, 0.000000000000000000, 1.000000000000000000 ) ) ;
#51134 = CARTESIAN_POINT ( 'NONE',  ( -339.1964088526558498, -182.0095552316575152, 7.608018572113563138 ) ) ;
#51135 = VECTOR ( 'NONE', #33044, 1000.000000000000000 ) ;
#51136 = FACE_OUTER_BOUND ( 'NONE', #14378, .T. ) ;
#51138 = EDGE_CURVE ( 'NONE', #46759, #41926, #15436, .T. ) ;
#51137 = DIRECTION ( 'NONE',  ( 1.000000000000000000, -8.718379230999705894E-17, 9.132017516997905925E-31 ) ) ;
#51139 = EDGE_LOOP ( 'NONE', ( #43513, #25306, #50642, #48974 ) ) ;
#51140 = CARTESIAN_POINT ( 'NONE',  ( -147.0463339291295881, -193.5000000000000000, 76.87330921200150158 ) ) ;
#51141 = VERTEX_POINT ( 'NONE', #38800 ) ;
#51142 = CARTESIAN_POINT ( 'NONE',  ( -166.8403286750647965, -175.3837268820161057, -40.19484891389966918 ) ) ;
#51143 = VECTOR ( 'NONE', #39800, 1000.000000000000000 ) ;
#51144 = LINE ( 'NONE', #39007, #28666 ) ;
#51145 = ORIENTED_EDGE ( 'NONE', *, *, #49485, .T. ) ;
#51146 = DIRECTION ( 'NONE',  ( -0.000000000000000000, 1.000000000000000000, -0.000000000000000000 ) ) ;
#51147 = FACE_OUTER_BOUND ( 'NONE', #37581, .T. ) ;
#51148 = DIRECTION ( 'NONE',  ( 0.000000000000000000, 1.000000000000000000, 0.000000000000000000 ) ) ;
#51149 = DIRECTION ( 'NONE',  ( -0.5586467658036415873, 0.000000000000000000, -0.8294056854502090959 ) ) ;
#51150 = VECTOR ( 'NONE', #41403, 999.9999999999998863 ) ;
#51151 = CARTESIAN_POINT ( 'NONE',  ( -339.1964088526558498, -157.4273119900845757, 48.27201571436049932 ) ) ;
#51152 = VERTEX_POINT ( 'NONE', #19114 ) ;
#51153 = EDGE_CURVE ( 'NONE', #42763, #138, #51828, .T. ) ;
#51154 = CARTESIAN_POINT ( 'NONE',  ( -339.1964088526558498, -89.57268800991437274, 48.27201571435973904 ) ) ;
#51156 = ORIENTED_EDGE ( 'NONE', *, *, #17958, .F. ) ;
#51155 = LINE ( 'NONE', #15141, #21115 ) ;
#51157 = EDGE_LOOP ( 'NONE', ( #45422, #48528, #23546, #44856 ) ) ;
#51158 = LINE ( 'NONE', #46170, #51480 ) ;
#51159 = ORIENTED_EDGE ( 'NONE', *, *, #51573, .F. ) ;
#51160 = EDGE_CURVE ( 'NONE', #9630, #23170, #31667, .T. ) ;
#51161 = CARTESIAN_POINT ( 'NONE',  ( 73.32544842769512172, -177.1207230881787780, -23.23456943914042228 ) ) ;
#51162 = EDGE_LOOP ( 'NONE', ( #12715, #30937, #24647, #21426 ) ) ;
#51163 = AXIS2_PLACEMENT_3D ( 'NONE', #25663, #41695, #13579 ) ;
#51164 = CARTESIAN_POINT ( 'NONE',  ( 76.21810084846656252, -177.1207230881787780, -8.694908215727989997 ) ) ;
#51165 = LINE ( 'NONE', #6995, #49793 ) ;
#51166 = EDGE_LOOP ( 'NONE', ( #40009, #24418, #12484, #9961 ) ) ;
#51167 = CARTESIAN_POINT ( 'NONE',  ( -114.4014177456970884, -183.6283474603465606, 105.0256126866236031 ) ) ;
#51168 = AXIS2_PLACEMENT_3D ( 'NONE', #44035, #23030, #39817 ) ;
#51169 = FACE_OUTER_BOUND ( 'NONE', #39123, .T. ) ;
#51170 = LINE ( 'NONE', #47733, #15686 ) ;
#51171 = ORIENTED_EDGE ( 'NONE', *, *, #33174, .F. ) ;
#51172 = ORIENTED_EDGE ( 'NONE', *, *, #43323, .T. ) ;
#51173 = EDGE_LOOP ( 'NONE', ( #16199, #2139, #9027, #2874 ) ) ;
#51174 = CARTESIAN_POINT ( 'NONE',  ( -82.67254833784559764, -177.1207230881787780, -120.2323164553483963 ) ) ;
#51175 = CARTESIAN_POINT ( 'NONE',  ( -47.66663987350317200, -183.6283474603465606, -0.5829794791144634614 ) ) ;
#51176 = CARTESIAN_POINT ( 'NONE',  ( -160.2705093830644216, -193.5000000000000000, -55.92572546981520532 ) ) ;
#51177 = CARTESIAN_POINT ( 'NONE',  ( -339.1964088526558498, -84.00150778970767362, -43.83057281297470098 ) ) ;
#51178 = FACE_OUTER_BOUND ( 'NONE', #42559, .T. ) ;
#51179 = ORIENTED_EDGE ( 'NONE', *, *, #8938, .F. ) ;
#51180 = VECTOR ( 'NONE', #14129, 1000.000000000000114 ) ;
#51181 = DIRECTION ( 'NONE',  ( 0.02963332782254913048, 0.000000000000000000, 0.9995608365087946812 ) ) ;
#51182 = VERTEX_POINT ( 'NONE', #23044 ) ;
#51184 = VERTEX_POINT ( 'NONE', #11467 ) ;
#51183 = CARTESIAN_POINT ( 'NONE',  ( -47.49008656418669005, -189.7472609257535510, -0.1476465640024710591 ) ) ;
#51185 = ORIENTED_EDGE ( 'NONE', *, *, #34552, .T. ) ;
#51186 = DIRECTION ( 'NONE',  ( -0.9785564922995046988, 0.000000000000000000, 0.2059786187410953262 ) ) ;
#51187 = DIRECTION ( 'NONE',  ( 0.000000000000000000, -0.9709418174260519008, 0.2393156642875582940 ) ) ;
#51188 = FACE_OUTER_BOUND ( 'NONE', #51115, .T. ) ;
#51189 = EDGE_CURVE ( 'NONE', #39634, #42649, #27504, .T. ) ;
#51190 = DIRECTION ( 'NONE',  ( -1.000000000000000000, -8.589602288500793681E-15, 5.928974370888963984E-15 ) ) ;
#51191 = EDGE_LOOP ( 'NONE', ( #9158, #9816, #24492, #30819 ) ) ;
#51192 = DIRECTION ( 'NONE',  ( 0.000000000000000000, -0.000000000000000000, 1.000000000000000000 ) ) ;
#51193 = ORIENTED_EDGE ( 'NONE', *, *, #26947, .F. ) ;
#51194 = ORIENTED_EDGE ( 'NONE', *, *, #48696, .F. ) ;
#51195 = DIRECTION ( 'NONE',  ( -0.000000000000000000, 0.4647231720437789981, 0.8854560256532044704 ) ) ;
#51196 = LINE ( 'NONE', #357, #27270 ) ;
#51197 = AXIS2_PLACEMENT_3D ( 'NONE', #4218, #33102, #45221 ) ;
#51198 = LINE ( 'NONE', #39842, #20273 ) ;
#51199 = ORIENTED_EDGE ( 'NONE', *, *, #39100, .F. ) ;
#51200 = FACE_OUTER_BOUND ( 'NONE', #50766, .T. ) ;
#51201 = CARTESIAN_POINT ( 'NONE',  ( -138.3705904895685137, -183.6283474603465606, -86.85922373029302435 ) ) ;
#51202 = DIRECTION ( 'NONE',  ( -0.000000000000000000, -0.9350162426854121689, 0.3546048870425426158 ) ) ;
#51203 = CARTESIAN_POINT ( 'NONE',  ( -48.65601702663141737, -193.5000000000000000, -0.9842305779475923888 ) ) ;
#51204 = VERTEX_POINT ( 'NONE', #3585 ) ;
#51205 = DIRECTION ( 'NONE',  ( -0.000000000000000000, 1.000000000000000000, -0.000000000000000000 ) ) ;
#51206 = DIRECTION ( 'NONE',  ( 0.000000000000000000, -0.000000000000000000, 1.000000000000000000 ) ) ;
#51207 = FACE_BOUND ( 'NONE', #46462, .T. ) ;
#51208 = VERTEX_POINT ( 'NONE', #19618 ) ;
#51209 = EDGE_CURVE ( 'NONE', #18089, #27933, #23321, .T. ) ;
#51210 = DIRECTION ( 'NONE',  ( -0.02963332782255633305, 0.000000000000000000, -0.9995608365087944591 ) ) ;
#51211 = DIRECTION ( 'NONE',  ( -0.000000000000000000, 1.000000000000000000, 0.000000000000000000 ) ) ;
#51212 = ORIENTED_EDGE ( 'NONE', *, *, #42998, .F. ) ;
#51213 = CARTESIAN_POINT ( 'NONE',  ( 33.75048693540709621, -189.7472609257535510, 94.14505102712816154 ) ) ;
#51214 = ORIENTED_EDGE ( 'NONE', *, *, #14510, .F. ) ;
#51215 = VECTOR ( 'NONE', #14067, 1000.000000000000000 ) ;
#51216 = VECTOR ( 'NONE', #6420, 1000.000000000000000 ) ;
#51217 = CARTESIAN_POINT ( 'NONE',  ( -9.671950287350391307, -193.5000000000000000, -118.8234112238815499 ) ) ;
#51218 = FACE_BOUND ( 'NONE', #24093, .T. ) ;
#51220 = ORIENTED_EDGE ( 'NONE', *, *, #38767, .F. ) ;
#51219 = CARTESIAN_POINT ( 'NONE',  ( 55.92943606843918047, -193.5000000000000000, -66.89437584437831674 ) ) ;
#51221 = CARTESIAN_POINT ( 'NONE',  ( -49.08592689732745384, -189.7472609257535510, 0.7948544414133550395 ) ) ;
#51222 = VERTEX_POINT ( 'NONE', #3334 ) ;
#51223 = VERTEX_POINT ( 'NONE', #14389 ) ;
#51224 = CARTESIAN_POINT ( 'NONE',  ( -5.461633243180957109, -189.7472609257535510, 116.2991637277478247 ) ) ;
#51225 = CIRCLE ( 'NONE', #28501, 16.00000000000000000 ) ;
#51226 = EDGE_LOOP ( 'NONE', ( #7424, #15301, #16396, #34682 ) ) ;
#51227 = DIRECTION ( 'NONE',  ( -0.000000000000000000, 1.000000000000000000, -0.000000000000000000 ) ) ;
#51228 = EDGE_CURVE ( 'NONE', #28668, #40958, #14051, .T. ) ;
#51229 = EDGE_CURVE ( 'NONE', #49925, #33429, #10431, .T. ) ;
#51230 = DIRECTION ( 'NONE',  ( -0.000000000000000000, 1.000000000000000000, -0.000000000000000000 ) ) ;
#51231 = LINE ( 'NONE', #6818, #44189 ) ;
#51232 = EDGE_LOOP ( 'NONE', ( #37107, #11827, #22055, #24059 ) ) ;
#51235 = VERTEX_POINT ( 'NONE', #22545 ) ;
#51234 = CARTESIAN_POINT ( 'NONE',  ( -112.2501518587238962, -175.3837268820161057, -106.3450133598699807 ) ) ;
#51233 = DIRECTION ( 'NONE',  ( -1.000000000000000000, -7.812315528781839335E-15, 6.921107616850815004E-15 ) ) ;
#51236 = DIRECTION ( 'NONE',  ( 0.9646355819083594074, 0.000000000000000000, -0.2635871660690647933 ) ) ;
#51237 = ORIENTED_EDGE ( 'NONE', *, *, #7569, .F. ) ;
#51238 = FACE_OUTER_BOUND ( 'NONE', #609, .T. ) ;
#51239 = VERTEX_POINT ( 'NONE', #18585 ) ;
#51240 = ADVANCED_FACE ( 'NONE', ( #46712 ), #10957, .F. ) ;
#51241 = DIRECTION ( 'NONE',  ( 0.000000000000000000, -0.1205366802553095168, 0.9927088740980556381 ) ) ;
#51242 = ORIENTED_EDGE ( 'NONE', *, *, #36834, .F. ) ;
#51244 = CARTESIAN_POINT ( 'NONE',  ( 8.294189685504184339, -193.5000000000000000, -110.2396968984190977 ) ) ;
#51243 = FACE_OUTER_BOUND ( 'NONE', #16472, .T. ) ;
#51245 = EDGE_LOOP ( 'NONE', ( #40883, #23114, #18699, #48852 ) ) ;
#51246 = EDGE_CURVE ( 'NONE', #41798, #44424, #40014, .T. ) ;
#51247 = VECTOR ( 'NONE', #23665, 1000.000000000000114 ) ;
#51248 = AXIS2_PLACEMENT_3D ( 'NONE', #46812, #18430, #14490 ) ;
#51249 = CARTESIAN_POINT ( 'NONE',  ( -339.1964088526558498, -123.5000000000000284, 0.000000000000000000 ) ) ;
#51250 = ORIENTED_EDGE ( 'NONE', *, *, #22270, .F. ) ;
#51251 = LINE ( 'NONE', #27046, #8597 ) ;
#51252 = EDGE_CURVE ( 'NONE', #10174, #21356, #46978, .T. ) ;
#51253 = CARTESIAN_POINT ( 'NONE',  ( -330.4913330509368166, -123.5000000000000284, -60.00000000000000000 ) ) ;
#51254 = VERTEX_POINT ( 'NONE', #7019 ) ;
#51255 = DIRECTION ( 'NONE',  ( -0.000000000000000000, 1.000000000000000000, -0.000000000000000000 ) ) ;
#51256 = CARTESIAN_POINT ( 'NONE',  ( -330.4913330509368166, -157.9941932480463436, 49.09328500076600932 ) ) ;
#51257 = PLANE ( 'NONE',  #46742 ) ;
#51258 = PLANE ( 'NONE',  #18177 ) ;
#51259 = ORIENTED_EDGE ( 'NONE', *, *, #48478, .F. ) ;
#51260 = CARTESIAN_POINT ( 'NONE',  ( 0.000000000000000000, 0.000000000000000000, 0.000000000000000000 ) ) ;
#51261 = DIRECTION ( 'NONE',  ( -0.6528221181905119463, 0.000000000000000000, -0.7575112421616284619 ) ) ;
#51262 = CARTESIAN_POINT ( 'NONE',  ( -47.97059563285963435, -177.1207230881787780, 0.8610436117673654355 ) ) ;
#51263 = CARTESIAN_POINT ( 'NONE',  ( -72.72541169915515979, -183.6283474603465606, 121.6072260099955429 ) ) ;
#51264 = VERTEX_POINT ( 'NONE', #40344 ) ;
#51265 = CIRCLE ( 'NONE', #2559, 125.0000000000000000 ) ;
#51266 = CARTESIAN_POINT ( 'NONE',  ( 9.336583202542589888, -193.5000000000000000, 110.8257356506556306 ) ) ;
#51267 = PLANE ( 'NONE',  #21066 ) ;
#51268 = EDGE_CURVE ( 'NONE', #12134, #3363, #51692, .T. ) ;
#51269 = CARTESIAN_POINT ( 'NONE',  ( -113.5519059482138857, -177.1207230881787780, 105.5544085257715210 ) ) ;
#51271 = VERTEX_POINT ( 'NONE', #44832 ) ;
#51270 = CARTESIAN_POINT ( 'NONE',  ( 2.266533711611407043, -175.3837268820161057, 113.1409892739925453 ) ) ;
#51272 = EDGE_LOOP ( 'NONE', ( #39385, #7924, #11930, #28714 ) ) ;
#51273 = DIRECTION ( 'NONE',  ( 0.000000000000000000, -1.000000000000000000, 0.000000000000000000 ) ) ;
#51274 = LINE ( 'NONE', #48098, #11937 ) ;
#51275 = DIRECTION ( 'NONE',  ( -0.000000000000000000, -0.7485107481710953081, 0.6631226582408016323 ) ) ;
#51276 = DIRECTION ( 'NONE',  ( 0.1182731709213592358, 0.000000000000000000, 0.9929810960135178055 ) ) ;
#51277 = AXIS2_PLACEMENT_3D ( 'NONE', #5843, #29991, #49712 ) ;
#51278 = ORIENTED_EDGE ( 'NONE', *, *, #9893, .F. ) ;
#51279 = CARTESIAN_POINT ( 'NONE',  ( -332.3517673607765914, -66.84438072661991725, -16.67542351306652648 ) ) ;
#51280 = ORIENTED_EDGE ( 'NONE', *, *, #14260, .T. ) ;
#51281 = VERTEX_POINT ( 'NONE', #51963 ) ;
#51282 = ORIENTED_EDGE ( 'NONE', *, *, #46811, .T. ) ;
#51283 = CARTESIAN_POINT ( 'NONE',  ( 60.00000000000001421, -173.5000000000000284, 60.00000000000000000 ) ) ;
#51284 = EDGE_CURVE ( 'NONE', #6162, #14589, #20651, .T. ) ;
#51285 = ADVANCED_FACE ( 'NONE', ( #35640 ), #4365, .F. ) ;
#51286 = DIRECTION ( 'NONE',  ( 0.000000000000000000, 0.000000000000000000, 1.000000000000000000 ) ) ;
#51287 = ORIENTED_EDGE ( 'NONE', *, *, #46279, .F. ) ;
#51288 = DIRECTION ( 'NONE',  ( -0.000000000000000000, 1.000000000000000000, -0.000000000000000000 ) ) ;
#51289 = FACE_OUTER_BOUND ( 'NONE', #19803, .T. ) ;
#51292 = VERTEX_POINT ( 'NONE', #44047 ) ;
#51291 = CARTESIAN_POINT ( 'NONE',  ( -339.1964088526558498, -103.0458197858324496, 55.34326076196052213 ) ) ;
#51290 = CARTESIAN_POINT ( 'NONE',  ( -5.461633243180942898, -193.5000000000000000, 116.2991637277478247 ) ) ;
#51293 = CIRCLE ( 'NONE', #24425, 16.00000000000000355 ) ;
#51294 = DIRECTION ( 'NONE',  ( 0.000000000000000000, 0.000000000000000000, -1.000000000000000000 ) ) ;
#51295 = ORIENTED_EDGE ( 'NONE', *, *, #3543, .T. ) ;
#51296 = CARTESIAN_POINT ( 'NONE',  ( -47.55243714407701816, -177.1207230881787780, -0.3758275821142288420 ) ) ;
#51297 = VERTEX_POINT ( 'NONE', #8556 ) ;
#51298 = CARTESIAN_POINT ( 'NONE',  ( -49.03777351731250889, -189.7472609257535510, 0.8294056854502042109 ) ) ;
#51299 = ADVANCED_FACE ( 'NONE', ( #36412 ), #24592, .T. ) ;
#51300 = CARTESIAN_POINT ( 'NONE',  ( -339.1964088526558498, -115.8919814278862503, 58.50955523165745831 ) ) ;
#51302 = PLANE ( 'NONE',  #20652 ) ;
#51301 = CARTESIAN_POINT ( 'NONE',  ( -84.19171550243319757, -189.7472609257535510, 119.7898618611247628 ) ) ;
#51303 = ORIENTED_EDGE ( 'NONE', *, *, #21703, .T. ) ;
#51304 = EDGE_CURVE ( 'NONE', #3228, #4055, #48447, .T. ) ;
#51305 = CARTESIAN_POINT ( 'NONE',  ( -47.92047998570520662, -175.3837268820161057, 0.8294056854502119824 ) ) ;
#51306 = ORIENTED_EDGE ( 'NONE', *, *, #39433, .F. ) ;
#51307 = CARTESIAN_POINT ( 'NONE',  ( -49.32472275501067571, -193.5000000000000000, -0.5338233779647935107 ) ) ;
#51308 = ADVANCED_FACE ( 'NONE', ( #32485 ), #24095, .F. ) ;
#51309 = CARTESIAN_POINT ( 'NONE',  ( -106.4764934152197497, -213.5000000000000000, -110.7307791902282759 ) ) ;
#51310 = ORIENTED_EDGE ( 'NONE', *, *, #43398, .T. ) ;
#51311 = CARTESIAN_POINT ( 'NONE',  ( 42.96730897722186171, 30.00000000000000355, -41.16782622478179832 ) ) ;
#51312 = VECTOR ( 'NONE', #47119, 1000.000000000000114 ) ;
#51313 = LINE ( 'NONE', #23196, #34885 ) ;
#51314 = ADVANCED_FACE ( 'NONE', ( #690 ), #36162, .F. ) ;
#51315 = EDGE_LOOP ( 'NONE', ( #27432, #12999, #17512, #5097 ) ) ;
#51316 = FACE_BOUND ( 'NONE', #16424, .T. ) ;
#51317 = DIRECTION ( 'NONE',  ( 1.043714542225393381E-14, 0.3546048870425235200, -0.9350162426854194964 ) ) ;
#51318 = AXIS2_PLACEMENT_3D ( 'NONE', #30837, #50815, #42910 ) ;
#51319 = VERTEX_POINT ( 'NONE', #12512 ) ;
#51320 = CARTESIAN_POINT ( 'NONE',  ( 66.03142248012325410, -177.1207230881787780, 50.12318939044039467 ) ) ;
#51321 = ORIENTED_EDGE ( 'NONE', *, *, #14766, .F. ) ;
#51322 = DIRECTION ( 'NONE',  ( -0.000000000000000000, 1.000000000000000000, -0.000000000000000000 ) ) ;
#51323 = DIRECTION ( 'NONE',  ( 0.000000000000000000, 0.000000000000000000, 1.000000000000000000 ) ) ;
#51324 = ORIENTED_EDGE ( 'NONE', *, *, #1266, .F. ) ;
#51325 = DIRECTION ( 'NONE',  ( -0.000000000000000000, 1.000000000000000000, -0.000000000000000000 ) ) ;
#51326 = CARTESIAN_POINT ( 'NONE',  ( -48.47912675150885065, -183.6283474603465606, 6.938893903907228378E-15 ) ) ;
#51327 = LINE ( 'NONE', #39474, #46724 ) ;
#51328 = VECTOR ( 'NONE', #28746, 1000.000000000000000 ) ;
#51329 = CARTESIAN_POINT ( 'NONE',  ( -49.40581635894068313, -177.1207230881787780, -0.3758275821142418316 ) ) ;
#51330 = EDGE_CURVE ( 'NONE', #20850, #6563, #31709, .T. ) ;
#51331 = VECTOR ( 'NONE', #42347, 1000.000000000000000 ) ;
#51332 = LINE ( 'NONE', #3482, #14439 ) ;
#51333 = CARTESIAN_POINT ( 'NONE',  ( -48.47912675150885065, -175.3837268820161057, 6.938893903907228378E-15 ) ) ;
#51335 = ORIENTED_EDGE ( 'NONE', *, *, #25022, .T. ) ;
#51334 = LINE ( 'NONE', #6673, #27002 ) ;
#51336 = ORIENTED_EDGE ( 'NONE', *, *, #4140, .F. ) ;
#51337 = DIRECTION ( 'NONE',  ( 0.000000000000000000, 0.000000000000000000, -1.000000000000000000 ) ) ;
#51338 = EDGE_CURVE ( 'NONE', #41926, #43754, #40887, .T. ) ;
#51339 = CARTESIAN_POINT ( 'NONE',  ( -153.2421220336517820, -193.5000000000000000, -66.33788548805446794 ) ) ;
#51340 = ORIENTED_EDGE ( 'NONE', *, *, #46544, .F. ) ;
#51341 = ORIENTED_EDGE ( 'NONE', *, *, #15580, .F. ) ;
#51342 = FACE_OUTER_BOUND ( 'NONE', #45425, .T. ) ;
#51343 = EDGE_LOOP ( 'NONE', ( #26994, #1729, #6140, #7944 ) ) ;
#51344 = CARTESIAN_POINT ( 'NONE',  ( -48.47912675150885065, -175.3837268820161057, 6.938893903907228378E-15 ) ) ;
#51345 = CARTESIAN_POINT ( 'NONE',  ( -48.47912675150885065, -189.7472609257535510, 6.938893903907228378E-15 ) ) ;
#51346 = VECTOR ( 'NONE', #47189, 1000.000000000000114 ) ;
#51347 = EDGE_CURVE ( 'NONE', #39427, #43863, #15952, .T. ) ;
#51348 = ADVANCED_FACE ( 'NONE', ( #35910 ), #31959, .T. ) ;
#51349 = EDGE_CURVE ( 'NONE', #34284, #42517, #43786, .T. ) ;
#51350 = EDGE_CURVE ( 'NONE', #44477, #45342, #18252, .T. ) ;
#51351 = CARTESIAN_POINT ( 'NONE',  ( 74.31448861501726810, -183.6283474603465606, -23.38221600314288651 ) ) ;
#51352 = DIRECTION ( 'NONE',  ( 0.000000000000000000, -1.000000000000000000, -0.000000000000000000 ) ) ;
#51353 = CIRCLE ( 'NONE', #27797, 124.9999999999999858 ) ;
#51354 = VERTEX_POINT ( 'NONE', #28778 ) ;
#51355 = ORIENTED_EDGE ( 'NONE', *, *, #5805, .F. ) ;
#51356 = ADVANCED_FACE ( 'NONE', ( #8051 ), #28010, .T. ) ;
#51358 = EDGE_LOOP ( 'NONE', ( #33232, #51737, #2392, #15762 ) ) ;
#51357 = AXIS2_PLACEMENT_3D ( 'NONE', #14237, #49978, #50247 ) ;
#51359 = CARTESIAN_POINT ( 'NONE',  ( -48.24424070572786860, -177.1207230881787780, -0.9720229140804037549 ) ) ;
#51360 = CARTESIAN_POINT ( 'NONE',  ( -99.22478721462985618, -175.3837268820161057, -113.1409892739921901 ) ) ;
#51361 = CARTESIAN_POINT ( 'NONE',  ( -47.82630463331832971, -193.5000000000000000, -0.7575112421616121416 ) ) ;
#51362 = EDGE_CURVE ( 'NONE', #23489, #48517, #44328, .T. ) ;
#51363 = CARTESIAN_POINT ( 'NONE',  ( -49.45768324380835423, -175.3837268820161057, -0.2059786187411025149 ) ) ;
#51364 = DIRECTION ( 'NONE',  ( 0.000000000000000000, 0.000000000000000000, 1.000000000000000000 ) ) ;
#51365 = VERTEX_POINT ( 'NONE', #49305 ) ;
#51366 = EDGE_CURVE ( 'NONE', #20985, #43547, #49824, .T. ) ;
#51367 = CARTESIAN_POINT ( 'NONE',  ( -123.4791267515088435, -198.5000000000000000, 70.00000000000000000 ) ) ;
#51368 = CARTESIAN_POINT ( 'NONE',  ( 15.29189835570547551, -189.7472609257535510, 106.3450133598704213 ) ) ;
#51369 = ADVANCED_FACE ( 'NONE', ( #37723 ), #45624, .F. ) ;
#51370 = VERTEX_POINT ( 'NONE', #42168 ) ;
#51371 = ORIENTED_EDGE ( 'NONE', *, *, #32776, .T. ) ;
#51372 = AXIS2_PLACEMENT_3D ( 'NONE', #33933, #18183, #49487 ) ;
#51373 = AXIS2_PLACEMENT_3D ( 'NONE', #34587, #25939, #41713 ) ;
#51374 = CARTESIAN_POINT ( 'NONE',  ( -172.6359455740846442, -193.5000000000000000, -14.49428645563791562 ) ) ;
#51375 = EDGE_CURVE ( 'NONE', #44410, #45844, #5417, .T. ) ;
#51376 = DIRECTION ( 'NONE',  ( -0.000000000000000000, 1.000000000000000000, -0.000000000000000000 ) ) ;
#51377 = ORIENTED_EDGE ( 'NONE', *, *, #41395, .T. ) ;
#51378 = DIRECTION ( 'NONE',  ( -0.000000000000000000, -3.491481338843133355E-15, -1.000000000000000000 ) ) ;
#51379 = ADVANCED_FACE ( 'NONE', ( #5159 ), #13293, .T. ) ;
#51380 = CARTESIAN_POINT ( 'NONE',  ( -82.67254833784559764, -183.6283474603465606, -120.2323164553484105 ) ) ;
#51381 = LINE ( 'NONE', #11149, #25946 ) ;
#51382 = EDGE_LOOP ( 'NONE', ( #9236, #934, #39309, #4120 ) ) ;
#51383 = CARTESIAN_POINT ( 'NONE',  ( -120.2975302769383177, -183.6283474603465606, 102.3089288139534005 ) ) ;
#51384 = EDGE_CURVE ( 'NONE', #48674, #21917, #1976, .T. ) ;
#51385 = ORIENTED_EDGE ( 'NONE', *, *, #43648, .T. ) ;
#51386 = CARTESIAN_POINT ( 'NONE',  ( -330.4913330509368166, -123.5000000000000284, 0.000000000000000000 ) ) ;
#51387 = CARTESIAN_POINT ( 'NONE',  ( -167.1580984288390823, -193.5000000000000000, -39.24667733211878584 ) ) ;
#51388 = ORIENTED_EDGE ( 'NONE', *, *, #4709, .T. ) ;
#51389 = AXIS2_PLACEMENT_3D ( 'NONE', #28741, #37157, #41106 ) ;
#51390 = DIRECTION ( 'NONE',  ( 0.000000000000000000, -0.1205366802553337752, -0.9927088740980526405 ) ) ;
#51391 = CARTESIAN_POINT ( 'NONE',  ( -48.41988612361515010, -189.7472609257535510, 0.9982437317643287900 ) ) ;
#51392 = CARTESIAN_POINT ( 'NONE',  ( -336.3521761649654422, -123.5000000000000284, 0.000000000000000000 ) ) ;
#51393 = CARTESIAN_POINT ( 'NONE',  ( -117.6201219941651601, -189.7472609257535510, 104.1370384486469902 ) ) ;
#51394 = ADVANCED_FACE ( 'NONE', ( #13812 ), #30092, .T. ) ;
#51395 = AXIS2_PLACEMENT_3D ( 'NONE', #7631, #39926, #23651 ) ;
#51396 = EDGE_CURVE ( 'NONE', #50209, #512, #21950, .T. ) ;
#51397 = CARTESIAN_POINT ( 'NONE',  ( -0.6536498292959314060, -183.6283474603465606, 114.4068333132749160 ) ) ;
#51398 = VERTEX_POINT ( 'NONE', #36948 ) ;
#51399 = VERTEX_POINT ( 'NONE', #9355 ) ;
#51400 = CARTESIAN_POINT ( 'NONE',  ( -152.3176060415594861, -183.6283474603465606, -69.58857822034966034 ) ) ;
#51402 = EDGE_LOOP ( 'NONE', ( #47282, #22923, #7102, #29405 ) ) ;
#51401 = DIRECTION ( 'NONE',  ( -0.000000000000000000, 1.000000000000000000, -0.000000000000000000 ) ) ;
#51403 = ORIENTED_EDGE ( 'NONE', *, *, #41074, .T. ) ;
#51404 = LINE ( 'NONE', #35098, #11176 ) ;
#51405 = AXIS2_PLACEMENT_3D ( 'NONE', #39928, #511, #16572 ) ;
#51406 = AXIS2_PLACEMENT_3D ( 'NONE', #5939, #21953, #26403 ) ;
#51407 = DIRECTION ( 'NONE',  ( 1.000000000000000000, -0.000000000000000000, -0.000000000000000000 ) ) ;
#51408 = AXIS2_PLACEMENT_3D ( 'NONE', #3090, #7042, #19132 ) ;
#51409 = VECTOR ( 'NONE', #29818, 999.9999999999998863 ) ;
#51410 = ORIENTED_EDGE ( 'NONE', *, *, #30764, .T. ) ;
#51411 = CARTESIAN_POINT ( 'NONE',  ( -166.0019676197264005, -193.5000000000000000, 39.55227055146320225 ) ) ;
#51412 = CARTESIAN_POINT ( 'NONE',  ( -84.82349129030166068, -175.3837268820161057, -119.5996955107802222 ) ) ;
#51413 = VERTEX_POINT ( 'NONE', #25625 ) ;
#51414 = DIRECTION ( 'NONE',  ( 0.000000000000000000, 1.000000000000000000, 0.000000000000000000 ) ) ;
#51415 = EDGE_CURVE ( 'NONE', #42978, #25561, #11564, .T. ) ;
#51416 = ADVANCED_FACE ( 'NONE', ( #5684 ), #939, .T. ) ;
#51417 = CARTESIAN_POINT ( 'NONE',  ( -68.21229068036657850, -183.6283474603465606, -123.4325817657429809 ) ) ;
#51418 = FACE_OUTER_BOUND ( 'NONE', #47586, .T. ) ;
#51419 = EDGE_LOOP ( 'NONE', ( #31425, #17500, #34172, #26533 ) ) ;
#51420 = EDGE_LOOP ( 'NONE', ( #20430, #2181, #43241, #16988 ) ) ;
#51421 = EDGE_CURVE ( 'NONE', #22277, #6242, #37198, .T. ) ;
#51422 = EDGE_LOOP ( 'NONE', ( #44307, #21340, #36408, #23971 ) ) ;
#51423 = ADVANCED_FACE ( 'NONE', ( #17238 ), #33775, .F. ) ;
#51424 = CARTESIAN_POINT ( 'NONE',  ( 0.000000000000000000, -157.0158200571378018, 48.55604808772604741 ) ) ;
#51425 = CARTESIAN_POINT ( 'NONE',  ( -332.3517673607765914, -76.43926241122620979, -35.68215131113738181 ) ) ;
#51426 = FACE_OUTER_BOUND ( 'NONE', #25941, .T. ) ;
#51427 = FACE_OUTER_BOUND ( 'NONE', #28764, .T. ) ;
#51428 = FACE_OUTER_BOUND ( 'NONE', #41616, .T. ) ;
#51429 = VECTOR ( 'NONE', #14932, 1000.000000000000000 ) ;
#51430 = ORIENTED_EDGE ( 'NONE', *, *, #25944, .T. ) ;
#51431 = CIRCLE ( 'NONE', #28739, 125.0000000000000000 ) ;
#51432 = CARTESIAN_POINT ( 'NONE',  ( -490.0000000000001137, -168.5000000000000284, 14.36509618646847386 ) ) ;
#51433 = ORIENTED_EDGE ( 'NONE', *, *, #38414, .F. ) ;
#51435 = ORIENTED_EDGE ( 'NONE', *, *, #1130, .T. ) ;
#51434 = DIRECTION ( 'NONE',  ( -0.2920567706369694982, 0.000000000000000000, -0.9564009842765243130 ) ) ;
#51436 = ORIENTED_EDGE ( 'NONE', *, *, #29985, .F. ) ;
#51437 = DIRECTION ( 'NONE',  ( -0.2920567706369628924, 0.000000000000000000, -0.9564009842765264224 ) ) ;
#51438 = DIRECTION ( 'NONE',  ( -0.000000000000000000, 1.000000000000000000, -0.000000000000000000 ) ) ;
#51439 = DIRECTION ( 'NONE',  ( 0.9842305779475980509, 0.000000000000000000, -0.1768902751225666647 ) ) ;
#51440 = CARTESIAN_POINT ( 'NONE',  ( -332.3517673607765914, -128.9912765084839066, 58.76657425099337928 ) ) ;
#51441 = ORIENTED_EDGE ( 'NONE', *, *, #47971, .F. ) ;
#51442 = DIRECTION ( 'NONE',  ( 0.000000000000000000, 0.9350162426854157216, 0.3546048870425330679 ) ) ;
#51443 = ORIENTED_EDGE ( 'NONE', *, *, #16609, .F. ) ;
#51444 = VECTOR ( 'NONE', #33622, 1000.000000000000000 ) ;
#51445 = EDGE_CURVE ( 'NONE', #21618, #4514, #29828, .T. ) ;
#51446 = ORIENTED_EDGE ( 'NONE', *, *, #49091, .T. ) ;
#51447 = AXIS2_PLACEMENT_3D ( 'NONE', #20617, #1156, #17204 ) ;
#51449 = AXIS2_PLACEMENT_3D ( 'NONE', #18691, #35471, #51791 ) ;
#51448 = CARTESIAN_POINT ( 'NONE',  ( -48.47912675150885065, -193.5000000000000000, -0.9999999999999931166 ) ) ;
#51450 = CARTESIAN_POINT ( 'NONE',  ( -336.3521761649654422, -92.15051119686104641, -50.05135858667769355 ) ) ;
#51451 = DIRECTION ( 'NONE',  ( 0.000000000000000000, 0.8854560256532062468, -0.4647231720437755564 ) ) ;
#51452 = DIRECTION ( 'NONE',  ( -0.3482016354343995812, 0.000000000000000000, 0.9374196611341205632 ) ) ;
#51453 = LINE ( 'NONE', #35659, #23704 ) ;
#51454 = EDGE_LOOP ( 'NONE', ( #24394, #18339, #34877, #8046 ) ) ;
#51455 = CARTESIAN_POINT ( 'NONE',  ( 32.49319223169170812, -193.5000000000000000, -95.22858582633060109 ) ) ;
#51456 = LINE ( 'NONE', #35932, #39935 ) ;
#51457 = LINE ( 'NONE', #14422, #47571 ) ;
#51458 = ORIENTED_EDGE ( 'NONE', *, *, #43976, .T. ) ;
#51459 = DIRECTION ( 'NONE',  ( 0.000000000000000000, -1.000000000000000000, 0.000000000000000000 ) ) ;
#51460 = CIRCLE ( 'NONE', #34634, 125.0000000000000000 ) ;
#51461 = DIRECTION ( 'NONE',  ( 1.043714542225393539E-14, 0.6631226582408017434, 0.7485107481710954191 ) ) ;
#51462 = ORIENTED_EDGE ( 'NONE', *, *, #30150, .F. ) ;
#51463 = CARTESIAN_POINT ( 'NONE',  ( -339.1964088526558498, -150.4759391377560576, -52.47426709956116042 ) ) ;
#51464 = ORIENTED_EDGE ( 'NONE', *, *, #12434, .T. ) ;
#51465 = AXIS2_PLACEMENT_3D ( 'NONE', #6430, #26376, #14832 ) ;
#51466 = LINE ( 'NONE', #15466, #30984 ) ;
#51467 = FACE_BOUND ( 'NONE', #5637, .T. ) ;
#51469 = EDGE_LOOP ( 'NONE', ( #7186, #1949, #32537, #45401 ) ) ;
#51468 = DIRECTION ( 'NONE',  ( -0.8455960035018311727, 0.000000000000000000, 0.5338233779647826305 ) ) ;
#51470 = ADVANCED_FACE ( 'NONE', ( #16983 ), #37973, .T. ) ;
#51472 = VECTOR ( 'NONE', #21594, 1000.000000000000114 ) ;
#51471 = DIRECTION ( 'NONE',  ( 0.000000000000000000, 1.000000000000000000, 0.000000000000000000 ) ) ;
#51473 = CIRCLE ( 'NONE', #24600, 2.000000000000001776 ) ;
#51474 = ORIENTED_EDGE ( 'NONE', *, *, #1810, .T. ) ;
#51475 = ORIENTED_EDGE ( 'NONE', *, *, #8860, .T. ) ;
#51476 = CARTESIAN_POINT ( 'NONE',  ( -145.0195698084541505, -175.3837268820161057, 79.40367028273128369 ) ) ;
#51477 = VECTOR ( 'NONE', #39721, 1000.000000000000114 ) ;
#51478 = ORIENTED_EDGE ( 'NONE', *, *, #46397, .T. ) ;
#51479 = LINE ( 'NONE', #35174, #42710 ) ;
#51480 = VECTOR ( 'NONE', #19080, 1000.000000000000000 ) ;
#51481 = CARTESIAN_POINT ( 'NONE',  ( -48.47912675150885065, -189.7472609257535510, 6.938893903907228378E-15 ) ) ;
#51482 = EDGE_LOOP ( 'NONE', ( #26127, #41976, #28274, #23543 ) ) ;
#51485 = VERTEX_POINT ( 'NONE', #9870 ) ;
#51484 = PRESENTATION_STYLE_ASSIGNMENT (( #35433 ) ) ;
#51483 = LINE ( 'NONE', #52016, #46006 ) ;
#51486 = ADVANCED_FACE ( 'NONE', ( #13018 ), #41922, .T. ) ;
#51487 = CARTESIAN_POINT ( 'NONE',  ( -150.5215542367829755, -175.3837268820161057, -72.19655804061973470 ) ) ;
#51488 = ORIENTED_EDGE ( 'NONE', *, *, #37041, .F. ) ;
#51489 = LINE ( 'NONE', #35185, #18874 ) ;
#51490 = CIRCLE ( 'NONE', #10336, 14.36509618646847386 ) ;
#51491 = ORIENTED_EDGE ( 'NONE', *, *, #51268, .T. ) ;
#51492 = CARTESIAN_POINT ( 'NONE',  ( -332.3517673607765914, -80.42027357919624819, -40.34602258462219027 ) ) ;
#51493 = EDGE_LOOP ( 'NONE', ( #21529, #27319, #292, #937 ) ) ;
#51495 = CARTESIAN_POINT ( 'NONE',  ( 74.28166149629942083, -189.7472609257535510, 17.48697739784543259 ) ) ;
#51494 = CARTESIAN_POINT ( 'NONE',  ( -48.47912675150885065, -188.5000000000000284, 6.938893903907228378E-15 ) ) ;
#51496 = VERTEX_POINT ( 'NONE', #33528 ) ;
#51497 = AXIS2_PLACEMENT_3D ( 'NONE', #14503, #6619, #51038 ) ;
#51498 = LINE ( 'NONE', #38880, #38283 ) ;
#51499 = EDGE_LOOP ( 'NONE', ( #19898, #7843, #10725, #43647, #17284, #23524 ) ) ;
#51500 = CARTESIAN_POINT ( 'NONE',  ( -180.0000000000000568, -130.6726371812771959, -60.00000000000000711 ) ) ;
#51501 = DIRECTION ( 'NONE',  ( -0.000000000000000000, 1.000000000000000000, -0.000000000000000000 ) ) ;
#51502 = CARTESIAN_POINT ( 'NONE',  ( -167.4530144994566285, -193.5000000000000000, -34.94873081740325205 ) ) ;
#51503 = CARTESIAN_POINT ( 'NONE',  ( -48.47912675150885065, -213.5000000000000000, 6.938893903907228378E-15 ) ) ;
#51504 = DIRECTION ( 'NONE',  ( -0.9063077870366494926, 0.000000000000000000, 0.4226182617407002740 ) ) ;
#51505 = CYLINDRICAL_SURFACE ( 'NONE', #28053, 125.0000000000000000 ) ;
#51506 = ORIENTED_EDGE ( 'NONE', *, *, #27175, .F. ) ;
#51507 = ADVANCED_FACE ( 'NONE', ( #13547 ), #38502, .T. ) ;
#51508 = VECTOR ( 'NONE', #23442, 1000.000000000000000 ) ;
#51509 = CARTESIAN_POINT ( 'NONE',  ( 0.000000000000000000, -182.5000000000000568, 0.000000000000000000 ) ) ;
#51510 = DIRECTION ( 'NONE',  ( 0.000000000000000000, -1.000000000000000000, 0.000000000000000000 ) ) ;
#51511 = DIRECTION ( 'NONE',  ( 0.000000000000000000, 0.000000000000000000, 1.000000000000000000 ) ) ;
#51512 = EDGE_LOOP ( 'NONE', ( #49180, #45584 ) ) ;
#51513 = VECTOR ( 'NONE', #45684, 1000.000000000000000 ) ;
#51514 = CARTESIAN_POINT ( 'NONE',  ( -78.00521078983979351, -193.5000000000000000, 121.4627941443857111 ) ) ;
#51515 = CARTESIAN_POINT ( 'NONE',  ( -330.4913330509368166, -89.00580675195269009, 49.09328500076528456 ) ) ;
#51516 = DIRECTION ( 'NONE',  ( -1.000000000000000000, 0.000000000000000000, 0.000000000000000000 ) ) ;
#51518 = ORIENTED_EDGE ( 'NONE', *, *, #40361, .F. ) ;
#51517 = LINE ( 'NONE', #26561, #34190 ) ;
#51519 = EDGE_LOOP ( 'NONE', ( #36877, #40414, #17054, #40370 ) ) ;
#51520 = ORIENTED_EDGE ( 'NONE', *, *, #23464, .F. ) ;
#51521 = ADVANCED_FACE ( 'NONE', ( #34296 ), #2748, .F. ) ;
#51522 = CARTESIAN_POINT ( 'NONE',  ( -48.47912675150885065, -177.1207230881787780, 6.938893903907228378E-15 ) ) ;
#51523 = LINE ( 'NONE', #7389, #45466 ) ;
#51524 = FACE_OUTER_BOUND ( 'NONE', #8826, .T. ) ;
#51525 = CARTESIAN_POINT ( 'NONE',  ( 59.00260725618640123, -177.1207230881787780, -63.81752780152988436 ) ) ;
#51526 = AXIS2_PLACEMENT_3D ( 'NONE', #29653, #1019, #49899 ) ;
#51527 = ORIENTED_EDGE ( 'NONE', *, *, #3459, .T. ) ;
#51528 = EDGE_CURVE ( 'NONE', #36042, #10996, #46804, .T. ) ;
#51529 = CARTESIAN_POINT ( 'NONE',  ( -305.0000000000000568, -123.5000000000000284, 0.000000000000000000 ) ) ;
#51530 = ADVANCED_FACE ( 'NONE', ( #30595 ), #51013, .T. ) ;
#51531 = CIRCLE ( 'NONE', #6219, 60.00000000000000000 ) ;
#51532 = ORIENTED_EDGE ( 'NONE', *, *, #22028, .F. ) ;
#51533 = ORIENTED_EDGE ( 'NONE', *, *, #19897, .T. ) ;
#51534 = EDGE_CURVE ( 'NONE', #25869, #51239, #2498, .T. ) ;
#51535 = ORIENTED_EDGE ( 'NONE', *, *, #26501, .F. ) ;
#51536 = PLANE ( 'NONE',  #20002 ) ;
#51537 = DIRECTION ( 'NONE',  ( 0.000000000000000000, -0.000000000000000000, -1.000000000000000000 ) ) ;
#51539 = VERTEX_POINT ( 'NONE', #26401 ) ;
#51538 = CIRCLE ( 'NONE', #34720, 125.0000000000000000 ) ;
#51540 = FILL_AREA_STYLE ('',( #35753 ) ) ;
#51541 = FACE_OUTER_BOUND ( 'NONE', #25361, .T. ) ;
#51544 = ORIENTED_EDGE ( 'NONE', *, *, #38051, .T. ) ;
#51543 = DIRECTION ( 'NONE',  ( 1.000000000000000000, -0.000000000000000000, -0.000000000000000000 ) ) ;
#51542 = FACE_OUTER_BOUND ( 'NONE', #6811, .T. ) ;
#51545 = EDGE_CURVE ( 'NONE', #3888, #27923, #27170, .T. ) ;
#51546 = DIRECTION ( 'NONE',  ( -0.000000000000000000, -0.8229838658936536877, 0.5680647467311596976 ) ) ;
#51547 = VERTEX_POINT ( 'NONE', #6192 ) ;
#51548 = FACE_OUTER_BOUND ( 'NONE', #28963, .T. ) ;
#51549 = ORIENTED_EDGE ( 'NONE', *, *, #1585, .T. ) ;
#51550 = FACE_OUTER_BOUND ( 'NONE', #50093, .T. ) ;
#51551 = DIRECTION ( 'NONE',  ( 1.000000000000000000, -0.000000000000000000, -0.000000000000000000 ) ) ;
#51553 = CARTESIAN_POINT ( 'NONE',  ( -336.3521761649654422, -110.9652333097088217, -57.67619951860654481 ) ) ;
#51552 = LINE ( 'NONE', #33, #38331 ) ;
#51554 = EDGE_CURVE ( 'NONE', #18044, #33019, #26676, .T. ) ;
#51555 = ORIENTED_EDGE ( 'NONE', *, *, #13741, .F. ) ;
#51556 = CARTESIAN_POINT ( 'NONE',  ( 12.12533326292403935, -193.5000000000000000, 109.3256576763158847 ) ) ;
#51557 = LINE ( 'NONE', #44187, #32039 ) ;
#51558 = ORIENTED_EDGE ( 'NONE', *, *, #40096, .T. ) ;
#51559 = DIRECTION ( 'NONE',  ( -0.000000000000000000, 1.000000000000000000, -0.000000000000000000 ) ) ;
#51560 = VECTOR ( 'NONE', #10312, 1000.000000000000000 ) ;
#51561 = LINE ( 'NONE', #15836, #10594 ) ;
#51562 = ORIENTED_EDGE ( 'NONE', *, *, #8679, .F. ) ;
#51563 = PLANE ( 'NONE',  #5814 ) ;
#51565 = AXIS2_PLACEMENT_3D ( 'NONE', #35588, #31660, #3540 ) ;
#51564 = DIRECTION ( 'NONE',  ( -0.9473263538541876194, 0.000000000000000000, -0.3202698538628486746 ) ) ;
#51566 = CARTESIAN_POINT ( 'NONE',  ( -336.3521761649654422, -82.40546666720629787, 42.41660376256258047 ) ) ;
#51567 = VERTEX_POINT ( 'NONE', #34542 ) ;
#51568 = DIRECTION ( 'NONE',  ( -0.000000000000000000, -1.000000000000000000, 0.000000000000000000 ) ) ;
#51569 = ORIENTED_EDGE ( 'NONE', *, *, #946, .F. ) ;
#51570 = FACE_OUTER_BOUND ( 'NONE', #46889, .T. ) ;
#51571 = FACE_OUTER_BOUND ( 'NONE', #38024, .T. ) ;
#51572 = FACE_OUTER_BOUND ( 'NONE', #38475, .T. ) ;
#51573 = EDGE_CURVE ( 'NONE', #18899, #42898, #14591, .T. ) ;
#51574 = DIRECTION ( 'NONE',  ( -0.000000000000000000, 1.000000000000000000, -0.000000000000000000 ) ) ;
#51575 = DIRECTION ( 'NONE',  ( 0.000000000000000000, 0.000000000000000000, 1.000000000000000000 ) ) ;
#51576 = EDGE_CURVE ( 'NONE', #31784, #32782, #27438, .T. ) ;
#51577 = AXIS2_PLACEMENT_3D ( 'NONE', #43256, #48251, #27492 ) ;
#51578 = DIRECTION ( 'NONE',  ( -0.000000000000000000, 0.000000000000000000, 1.000000000000000000 ) ) ;
#51579 = CARTESIAN_POINT ( 'NONE',  ( -70.42295845586433245, -193.5000000000000000, -123.0587999703024877 ) ) ;
#51580 = DIRECTION ( 'NONE',  ( -0.000000000000000000, 1.000000000000000000, -0.000000000000000000 ) ) ;
#51582 = ORIENTED_EDGE ( 'NONE', *, *, #9516, .T. ) ;
#51581 = DIRECTION ( 'NONE',  ( 0.000000000000000000, -0.9350162426854107256, 0.3546048870425463906 ) ) ;
#51583 = ORIENTED_EDGE ( 'NONE', *, *, #44529, .T. ) ;
#51584 = CARTESIAN_POINT ( 'NONE',  ( -133.1483155860611021, -177.1207230881787780, -90.59430563621275212 ) ) ;
#51585 = ADVANCED_FACE ( 'NONE', ( #42707 ), #19050, .T. ) ;
#51586 = EDGE_CURVE ( 'NONE', #51869, #36336, #15789, .T. ) ;
#51587 = CARTESIAN_POINT ( 'NONE',  ( -332.3517673607765914, -145.9479049231020440, -54.58714071513102795 ) ) ;
#51588 = ORIENTED_EDGE ( 'NONE', *, *, #14298, .T. ) ;
#51589 = VERTEX_POINT ( 'NONE', #22207 ) ;
#51590 = EDGE_CURVE ( 'NONE', #21919, #9092, #31706, .T. ) ;
#51591 = DIRECTION ( 'NONE',  ( -0.3482016354343995812, 0.000000000000000000, 0.9374196611341205632 ) ) ;
#51592 = VERTEX_POINT ( 'NONE', #15119 ) ;
#51593 = CARTESIAN_POINT ( 'NONE',  ( -137.2624501260119700, -183.6283474603465606, 87.99159897727969337 ) ) ;
#51594 = LINE ( 'NONE', #27926, #25825 ) ;
#51595 = AXIS2_PLACEMENT_3D ( 'NONE', #8960, #41797, #24994 ) ;
#51596 = EDGE_CURVE ( 'NONE', #39834, #6765, #34795, .T. ) ;
#51597 = AXIS2_PLACEMENT_3D ( 'NONE', #45192, #9180, #49638 ) ;
#51598 = DIRECTION ( 'NONE',  ( 0.000000000000000000, 1.000000000000000000, 0.000000000000000000 ) ) ;
#51599 = CARTESIAN_POINT ( 'NONE',  ( -168.6933499419502880, -177.1207230881787780, 30.40954281680879845 ) ) ;
#51600 = VERTEX_POINT ( 'NONE', #30875 ) ;
#51601 = ORIENTED_EDGE ( 'NONE', *, *, #51732, .T. ) ;
#51602 = CIRCLE ( 'NONE', #27242, 125.0000000000000000 ) ;
#51603 = VERTEX_POINT ( 'NONE', #14862 ) ;
#51604 = CARTESIAN_POINT ( 'NONE',  ( -48.64924157374594671, -193.5000000000000000, 124.9998842437354227 ) ) ;
#51605 = DIRECTION ( 'NONE',  ( 0.000000000000000000, 0.000000000000000000, 1.000000000000000000 ) ) ;
#51606 = DIRECTION ( 'NONE',  ( -0.4031234292879730674, 0.000000000000000000, 0.9151456172430181280 ) ) ;
#51607 = AXIS2_PLACEMENT_3D ( 'NONE', #9217, #41254, #5281 ) ;
#51608 = PLANE ( 'NONE',  #10243 ) ;
#51609 = CARTESIAN_POINT ( 'NONE',  ( -49.17567778057184569, -177.1207230881787780, -0.7175072570443327136 ) ) ;
#51610 = ORIENTED_EDGE ( 'NONE', *, *, #16616, .F. ) ;
#51611 = DIRECTION ( 'NONE',  ( 0.000000000000000000, -1.000000000000000000, 0.000000000000000000 ) ) ;
#51612 = UNCERTAINTY_MEASURE_WITH_UNIT (LENGTH_MEASURE( 1.000000000000000082E-05 ), #44130, 'distance_accuracy_value', 'NONE');
#51613 = VECTOR ( 'NONE', #5607, 1000.000000000000114 ) ;
#51614 = CARTESIAN_POINT ( 'NONE',  ( 43.86477233319989466, -189.7472609257535510, -84.24728067915975771 ) ) ;
#51615 = CARTESIAN_POINT ( 'NONE',  ( -153.2421220336517536, -175.3837268820161057, -66.33788548805449636 ) ) ;
#51616 = EDGE_LOOP ( 'NONE', ( #48883, #45010, #48742, #18025 ) ) ;
#51617 = ORIENTED_EDGE ( 'NONE', *, *, #33302, .F. ) ;
#51618 = EDGE_LOOP ( 'NONE', ( #47393, #31802, #24583, #2880 ) ) ;
#51619 = DIRECTION ( 'NONE',  ( 1.000000000000000000, -0.000000000000000000, 0.000000000000000000 ) ) ;
#51620 = PLANE ( 'NONE',  #14089 ) ;
#51621 = ORIENTED_EDGE ( 'NONE', *, *, #36096, .T. ) ;
#51622 = DIRECTION ( 'NONE',  ( -0.000000000000000000, 1.000000000000000000, -0.000000000000000000 ) ) ;
#51623 = CARTESIAN_POINT ( 'NONE',  ( -339.1964088526558498, -89.57268800991437274, 48.27201571435973904 ) ) ;
#51624 = DIRECTION ( 'NONE',  ( 0.000000000000000000, 1.000000000000000000, -0.000000000000000000 ) ) ;
#51625 = ORIENTED_EDGE ( 'NONE', *, *, #23052, .T. ) ;
#51626 = CARTESIAN_POINT ( 'NONE',  ( 60.00000000000001421, 20.00000000000000000, 60.00000000000000711 ) ) ;
#51627 = VERTEX_POINT ( 'NONE', #31125 ) ;
#51628 = DIRECTION ( 'NONE',  ( -1.000000000000000000, -0.000000000000000000, -0.000000000000000000 ) ) ;
#51629 = FACE_BOUND ( 'NONE', #32671, .T. ) ;
#51630 = VECTOR ( 'NONE', #27246, 1000.000000000000000 ) ;
#51631 = EDGE_CURVE ( 'NONE', #153, #43387, #46924, .T. ) ;
#51632 = DIRECTION ( 'NONE',  ( 0.000000000000000000, 0.000000000000000000, -1.000000000000000000 ) ) ;
#51633 = EDGE_LOOP ( 'NONE', ( #23301, #2075, #18220, #12819 ) ) ;
#51634 = AXIS2_PLACEMENT_3D ( 'NONE', #44387, #4179, #15489 ) ;
#51635 = VECTOR ( 'NONE', #37931, 1000.000000000000000 ) ;
#51636 = EDGE_CURVE ( 'NONE', #6855, #10180, #43453, .T. ) ;
#51637 = DIRECTION ( 'NONE',  ( -1.000000000000000000, -0.000000000000000000, 0.000000000000000000 ) ) ;
#51638 = EDGE_CURVE ( 'NONE', #26450, #44661, #47417, .T. ) ;
#51639 = FACE_OUTER_BOUND ( 'NONE', #30570, .T. ) ;
#51640 = DIRECTION ( 'NONE',  ( 0.000000000000000000, -1.000000000000000000, -0.000000000000000000 ) ) ;
#51641 = EDGE_CURVE ( 'NONE', #43457, #22526, #14331, .T. ) ;
#51642 = CARTESIAN_POINT ( 'NONE',  ( 46.00000000000000711, 35.00000000000000000, -46.00000000000000000 ) ) ;
#51643 = AXIS2_PLACEMENT_3D ( 'NONE', #2772, #23008, #42975 ) ;
#51644 = EDGE_CURVE ( 'NONE', #15404, #17350, #16674, .T. ) ;
#51645 = VERTEX_POINT ( 'NONE', #27696 ) ;
#51646 = DIRECTION ( 'NONE',  ( -0.9646355819083614058, 0.000000000000000000, 0.2635871660690581320 ) ) ;
#51647 = ORIENTED_EDGE ( 'NONE', *, *, #50690, .F. ) ;
#51648 = ORIENTED_EDGE ( 'NONE', *, *, #20491, .F. ) ;
#51649 = EDGE_CURVE ( 'NONE', #35024, #16698, #11670, .T. ) ;
#51650 = CIRCLE ( 'NONE', #11339, 14.36509618646847386 ) ;
#51651 = DIRECTION ( 'NONE',  ( 0.000000000000000000, 1.000000000000000000, -0.000000000000000000 ) ) ;
#51653 = VERTEX_POINT ( 'NONE', #11918 ) ;
#51652 = DIRECTION ( 'NONE',  ( -1.000000000000000000, 0.000000000000000000, 0.000000000000000000 ) ) ;
#51654 = EDGE_CURVE ( 'NONE', #20241, #14966, #31898, .T. ) ;
#51655 = VECTOR ( 'NONE', #12989, 1000.000000000000114 ) ;
#51656 = ORIENTED_EDGE ( 'NONE', *, *, #22554, .F. ) ;
#51657 = DIRECTION ( 'NONE',  ( 0.000000000000000000, 1.000000000000000000, 0.000000000000000000 ) ) ;
#51658 = EDGE_CURVE ( 'NONE', #25920, #13751, #43729, .T. ) ;
#51659 = VECTOR ( 'NONE', #19472, 1000.000000000000000 ) ;
#51660 = EDGE_CURVE ( 'NONE', #25409, #28008, #654, .T. ) ;
#51661 = VECTOR ( 'NONE', #13601, 1000.000000000000000 ) ;
#51662 = CARTESIAN_POINT ( 'NONE',  ( 13.86276369408136411, -193.5000000000000000, -107.1890582354654669 ) ) ;
#51663 = ORIENTED_EDGE ( 'NONE', *, *, #47130, .F. ) ;
#51664 = ADVANCED_FACE ( 'NONE', ( #47692 ), #24531, .T. ) ;
#51665 = CARTESIAN_POINT ( 'NONE',  ( -103.4012653778457320, -183.6283474603465606, -112.2878385610366649 ) ) ;
#51666 = DIRECTION ( 'NONE',  ( 0.000000000000000000, -1.000000000000000000, 0.000000000000000000 ) ) ;
#51667 = ORIENTED_EDGE ( 'NONE', *, *, #9515, .T. ) ;
#51668 = FACE_OUTER_BOUND ( 'NONE', #34948, .T. ) ;
#51669 = DIRECTION ( 'NONE',  ( 0.000000000000000000, -1.288321301492108820E-13, 1.000000000000000000 ) ) ;
#51670 = EDGE_CURVE ( 'NONE', #46650, #19973, #44255, .T. ) ;
#51671 = LINE ( 'NONE', #39037, #22739 ) ;
#51672 = CARTESIAN_POINT ( 'NONE',  ( -49.13194886969936448, -193.5000000000000000, -0.7575112421616214675 ) ) ;
#51673 = ORIENTED_EDGE ( 'NONE', *, *, #26528, .T. ) ;
#51674 = ORIENTED_EDGE ( 'NONE', *, *, #30676, .F. ) ;
#51675 = ADVANCED_FACE ( 'NONE', ( #47939 ), #16400, .T. ) ;
#51676 = ORIENTED_EDGE ( 'NONE', *, *, #40714, .T. ) ;
#51677 = CARTESIAN_POINT ( 'NONE',  ( -330.4913330509368166, -102.1108035431471279, 54.98865587491800255 ) ) ;
#51678 = PLANE ( 'NONE',  #42792 ) ;
#51679 = VECTOR ( 'NONE', #34746, 1000.000000000000000 ) ;
#51680 = DIRECTION ( 'NONE',  ( 0.9646355819083556327, 0.000000000000000000, 0.2635871660690782825 ) ) ;
#51681 = CIRCLE ( 'NONE', #34039, 125.0000000000000000 ) ;
#51682 = DIRECTION ( 'NONE',  ( -0.8455960035018234011, 0.000000000000000000, -0.5338233779647948429 ) ) ;
#51683 = DIRECTION ( 'NONE',  ( 0.8294056854501971054, 0.000000000000000000, 0.5586467658036594619 ) ) ;
#51684 = ORIENTED_EDGE ( 'NONE', *, *, #6044, .T. ) ;
#51685 = CIRCLE ( 'NONE', #44085, 60.00000000000000000 ) ;
#51686 = ADVANCED_FACE ( 'NONE', ( #12691 ), #51620, .F. ) ;
#51687 = LINE ( 'NONE', #15688, #20721 ) ;
#51688 = ORIENTED_EDGE ( 'NONE', *, *, #27130, .F. ) ;
#51690 = ORIENTED_EDGE ( 'NONE', *, *, #48156, .T. ) ;
#51689 = PLANE ( 'NONE',  #16429 ) ;
#51691 = VERTEX_POINT ( 'NONE', #19555 ) ;
#51692 = LINE ( 'NONE', #40104, #11514 ) ;
#51693 = CARTESIAN_POINT ( 'NONE',  ( -160.7804753152582293, -189.7472609257535510, -52.57768177182448710 ) ) ;
#51694 = DIRECTION ( 'NONE',  ( -0.000000000000000000, 1.000000000000000000, -0.000000000000000000 ) ) ;
#51695 = PLANE ( 'NONE',  #12478 ) ;
#51696 = ORIENTED_EDGE ( 'NONE', *, *, #7670, .T. ) ;
#51697 = DIRECTION ( 'NONE',  ( 0.000000000000000000, 1.000000000000000000, 0.000000000000000000 ) ) ;
#51698 = ORIENTED_EDGE ( 'NONE', *, *, #26665, .F. ) ;
#51699 = AXIS2_PLACEMENT_3D ( 'NONE', #45169, #40934, #24390 ) ;
#51700 = EDGE_CURVE ( 'NONE', #17596, #4, #3162, .T. ) ;
#51701 = VERTEX_POINT ( 'NONE', #4565 ) ;
#51702 = DIRECTION ( 'NONE',  ( -0.000000000000000000, -0.000000000000000000, 1.000000000000000000 ) ) ;
#51703 = DIRECTION ( 'NONE',  ( -0.000000000000000000, 0.9350162426854194964, 0.3546048870425235200 ) ) ;
#51704 = CARTESIAN_POINT ( 'NONE',  ( -339.1964088526558498, -156.6043281241916816, -48.84008046109114076 ) ) ;
#51705 = ADVANCED_FACE ( 'NONE', ( #20589 ), #31638, .F. ) ;
#51706 = EDGE_CURVE ( 'NONE', #1891, #30689, #40030, .T. ) ;
#51707 = DIRECTION ( 'NONE',  ( 0.000000000000000000, 1.000000000000000000, 0.000000000000000000 ) ) ;
#51708 = LINE ( 'NONE', #7556, #3556 ) ;
#51709 = EDGE_CURVE ( 'NONE', #31952, #2646, #4054, .T. ) ;
#51710 = ORIENTED_EDGE ( 'NONE', *, *, #34702, .F. ) ;
#51711 = LINE ( 'NONE', #27769, #43938 ) ;
#51712 = CARTESIAN_POINT ( 'NONE',  ( -49.40581635894069024, -177.1207230881787780, 0.3758275821142362250 ) ) ;
#51713 = EDGE_CURVE ( 'NONE', #9367, #5804, #12174, .T. ) ;
#51714 = FACE_BOUND ( 'NONE', #51402, .T. ) ;
#51715 = ORIENTED_EDGE ( 'NONE', *, *, #31701, .F. ) ;
#51716 = VECTOR ( 'NONE', #7104, 1000.000000000000000 ) ;
#51717 = CIRCLE ( 'NONE', #3040, 4.000000000000003553 ) ;
#51718 = CARTESIAN_POINT ( 'NONE',  ( 57.66105628977221187, -189.7472609257535510, 66.02470404298190942 ) ) ;
#51719 = AXIS2_PLACEMENT_3D ( 'NONE', #38883, #46277, #50476 ) ;
#51720 = VECTOR ( 'NONE', #30811, 1000.000000000000000 ) ;
#51721 = CARTESIAN_POINT ( 'NONE',  ( 26.52087324849106054, -198.5000000000000000, -70.00000000000002842 ) ) ;
#51722 = ORIENTED_EDGE ( 'NONE', *, *, #842, .F. ) ;
#51723 = CARTESIAN_POINT ( 'NONE',  ( -339.1964088526558498, -71.02573290043878274, -26.97593913775585506 ) ) ;
#51724 = ORIENTED_EDGE ( 'NONE', *, *, #1089, .F. ) ;
#51725 = CARTESIAN_POINT ( 'NONE',  ( -157.5429198988176438, -193.5000000000000000, 61.07445476073480961 ) ) ;
#51726 = EDGE_CURVE ( 'NONE', #11608, #44829, #40285, .T. ) ;
#51727 = FACE_BOUND ( 'NONE', #36940, .T. ) ;
#51728 = CIRCLE ( 'NONE', #44172, 20.00000000000000000 ) ;
#51730 = ORIENTED_EDGE ( 'NONE', *, *, #15412, .F. ) ;
#51729 = CARTESIAN_POINT ( 'NONE',  ( -52.47502265695594303, -183.6283474603465606, -123.9361149384469627 ) ) ;
#51731 = VECTOR ( 'NONE', #12583, 1000.000000000000000 ) ;
#51732 = EDGE_CURVE ( 'NONE', #12493, #50437, #33413, .T. ) ;
#51733 = VECTOR ( 'NONE', #46523, 1000.000000000000000 ) ;
#51734 = CARTESIAN_POINT ( 'NONE',  ( -332.3517673607765914, -111.7106844931459761, -58.83036664750484590 ) ) ;
#51735 = ORIENTED_EDGE ( 'NONE', *, *, #44228, .F. ) ;
#51736 = ADVANCED_FACE ( 'NONE', ( #28206 ), #24279, .F. ) ;
#51737 = ORIENTED_EDGE ( 'NONE', *, *, #50589, .F. ) ;
#51738 = VECTOR ( 'NONE', #16521, 1000.000000000000000 ) ;
#51739 = PLANE ( 'NONE',  #1564 ) ;
#51740 = ORIENTED_EDGE ( 'NONE', *, *, #5701, .T. ) ;
#51741 = DIRECTION ( 'NONE',  ( 0.000000000000000000, -1.000000000000000000, 0.000000000000000000 ) ) ;
#51742 = LINE ( 'NONE', #48044, #49857 ) ;
#51743 =( NAMED_UNIT ( * ) SI_UNIT ( $, .STERADIAN. ) SOLID_ANGLE_UNIT ( ) );
#51744 = PLANE ( 'NONE',  #23917 ) ;
#51745 = ORIENTED_EDGE ( 'NONE', *, *, #39100, .T. ) ;
#51748 = ORIENTED_EDGE ( 'NONE', *, *, #42488, .T. ) ;
#51747 = DIRECTION ( 'NONE',  ( 0.9890401873221633666, 0.000000000000000000, 0.1476465640024850756 ) ) ;
#51746 = CARTESIAN_POINT ( 'NONE',  ( 70.19984492582109681, -193.5000000000000000, 39.24667733211968823 ) ) ;
#51749 = VECTOR ( 'NONE', #41938, 1000.000000000000000 ) ;
#51750 = ORIENTED_EDGE ( 'NONE', *, *, #8646, .F. ) ;
#51751 = VECTOR ( 'NONE', #21387, 999.9999999999998863 ) ;
#51752 = DIRECTION ( 'NONE',  ( 0.000000000000000000, 0.000000000000000000, -1.000000000000000000 ) ) ;
#51753 = EDGE_LOOP ( 'NONE', ( #11728, #8492, #6171, #32986 ) ) ;
#51754 = CARTESIAN_POINT ( 'NONE',  ( -339.1964088526558498, -157.4273119900845757, 48.27201571436049932 ) ) ;
#51755 = VERTEX_POINT ( 'NONE', #17176 ) ;
#51756 = CIRCLE ( 'NONE', #8947, 125.0000000000000000 ) ;
#51757 = LINE ( 'NONE', #15768, #50245 ) ;
#51758 = EDGE_LOOP ( 'NONE', ( #12988, #9646, #14793, #15518, #50123, #23358 ) ) ;
#51760 = DIRECTION ( 'NONE',  ( -0.000000000000000000, -0.8854560256532110207, -0.4647231720437664526 ) ) ;
#51759 = DIRECTION ( 'NONE',  ( -0.000000000000000000, -0.9350162426854169428, -0.3546048870425300148 ) ) ;
#51761 = VERTEX_POINT ( 'NONE', #37133 ) ;
#51762 = LINE ( 'NONE', #3653, #48354 ) ;
#51763 = VERTEX_POINT ( 'NONE', #33194 ) ;
#51764 = CARTESIAN_POINT ( 'NONE',  ( -330.4913330509368166, -131.2283041299240836, 59.50019592636143528 ) ) ;
#51765 = VECTOR ( 'NONE', #37711, 1000.000000000000000 ) ;
#51766 = CARTESIAN_POINT ( 'NONE',  ( -148.0127667507368585, -193.5000000000000000, -75.61781872352626976 ) ) ;
#51767 = AXIS2_PLACEMENT_3D ( 'NONE', #44402, #8388, #19686 ) ;
#51768 = CARTESIAN_POINT ( 'NONE',  ( 24.07160180756802248, -183.6283474603465606, 100.5610240384924481 ) ) ;
#51769 = CARTESIAN_POINT ( 'NONE',  ( -173.2765435274470178, -177.1207230881787780, -7.113702696401505321 ) ) ;
#51770 = DIRECTION ( 'NONE',  ( 0.000000000000000000, 0.000000000000000000, 1.000000000000000000 ) ) ;
#51771 = AXIS2_PLACEMENT_3D ( 'NONE', #10205, #21787, #25212 ) ;
#51772 = CIRCLE ( 'NONE', #6462, 60.00000000000000000 ) ;
#51773 = DIRECTION ( 'NONE',  ( 0.000000000000000000, -0.000000000000000000, 1.000000000000000000 ) ) ;
#51774 = ORIENTED_EDGE ( 'NONE', *, *, #40606, .T. ) ;
#51775 = EDGE_CURVE ( 'NONE', #16302, #23663, #5695, .T. ) ;
#51776 = EDGE_CURVE ( 'NONE', #40054, #43244, #41334, .T. ) ;
#51777 = CARTESIAN_POINT ( 'NONE',  ( 22.37192613399954055, 0.000000000000000000, -9.245099569271807593E-15 ) ) ;
#51778 = CIRCLE ( 'NONE', #9788, 125.0000000000000000 ) ;
#51779 = CARTESIAN_POINT ( 'NONE',  ( -336.3521761649654422, -67.75522407825191351, 19.39547174791671935 ) ) ;
#51780 = CARTESIAN_POINT ( 'NONE',  ( -26.53529504715431031, -175.3837268820161057, 123.0587999703026725 ) ) ;
#51781 = VECTOR ( 'NONE', #44182, 1000.000000000000000 ) ;
#51782 = DIRECTION ( 'NONE',  ( 0.9646355819083614058, 0.000000000000000000, -0.2635871660690581320 ) ) ;
#51783 = ORIENTED_EDGE ( 'NONE', *, *, #46495, .T. ) ;
#51784 = LINE ( 'NONE', #43873, #5548 ) ;
#51785 = CARTESIAN_POINT ( 'NONE',  ( -48.24424070572787571, -193.5000000000000000, 0.9720229140804191870 ) ) ;
#51787 = VERTEX_POINT ( 'NONE', #49760 ) ;
#51786 = DIRECTION ( 'NONE',  ( 0.000000000000000000, -2.775557561562891351E-15, 1.000000000000000000 ) ) ;
#51788 = ORIENTED_EDGE ( 'NONE', *, *, #2368, .T. ) ;
#51789 = ORIENTED_EDGE ( 'NONE', *, *, #34796, .T. ) ;
#51790 = VECTOR ( 'NONE', #34318, 1000.000000000000227 ) ;
#51791 = DIRECTION ( 'NONE',  ( 0.000000000000000000, 0.000000000000000000, -1.000000000000000000 ) ) ;
#51792 = AXIS2_PLACEMENT_3D ( 'NONE', #13705, #41037, #21068 ) ;
#51793 = DIRECTION ( 'NONE',  ( 1.000000000000000000, -0.000000000000000000, -0.000000000000000000 ) ) ;
#51794 = EDGE_CURVE ( 'NONE', #19072, #8637, #20863, .T. ) ;
#51795 = CARTESIAN_POINT ( 'NONE',  ( -170.2837019307126809, -183.6283474603465606, 23.23456943914128203 ) ) ;
#51796 = CARTESIAN_POINT ( 'NONE',  ( -102.5006284722403933, -183.6283474603465606, -112.7238987608084670 ) ) ;
#51797 = AXIS2_PLACEMENT_3D ( 'NONE', #26112, #22181, #10867 ) ;
#51798 = VERTEX_POINT ( 'NONE', #4837 ) ;
#51799 = DIRECTION ( 'NONE',  ( -0.000000000000000000, 0.000000000000000000, -1.000000000000000000 ) ) ;
#51800 = ADVANCED_FACE ( 'NONE', ( #45307 ), #33715, .T. ) ;
#51801 = ORIENTED_EDGE ( 'NONE', *, *, #21090, .T. ) ;
#51802 = CIRCLE ( 'NONE', #38395, 125.0000000000000000 ) ;
#51803 = ORIENTED_EDGE ( 'NONE', *, *, #36804, .T. ) ;
#51804 = AXIS2_PLACEMENT_3D ( 'NONE', #48185, #32141, #13218 ) ;
#51805 = VERTEX_POINT ( 'NONE', #37664 ) ;
#51806 = LINE ( 'NONE', #19462, #25896 ) ;
#51807 = CIRCLE ( 'NONE', #4801, 125.0000000000000000 ) ;
#51808 = AXIS2_PLACEMENT_3D ( 'NONE', #7678, #23702, #39712 ) ;
#51809 = CIRCLE ( 'NONE', #38362, 60.00000000000000000 ) ;
#51810 = ORIENTED_EDGE ( 'NONE', *, *, #857, .T. ) ;
#51811 = VECTOR ( 'NONE', #38095, 1000.000000000000000 ) ;
#51812 = SURFACE_STYLE_FILL_AREA ( #51540 ) ;
#51813 = DIRECTION ( 'NONE',  ( -0.000000000000000000, 0.2393156642875547968, -0.9709418174260527890 ) ) ;
#51816 = ORIENTED_EDGE ( 'NONE', *, *, #37609, .T. ) ;
#51815 = PLANE ( 'NONE',  #41743 ) ;
#51814 = CYLINDRICAL_SURFACE ( 'NONE', #27487, 125.0000000000000000 ) ;
#51817 = CARTESIAN_POINT ( 'NONE',  ( -115.7878797639662025, -183.6283474603465606, -104.1428419024399687 ) ) ;
#51818 = EDGE_LOOP ( 'NONE', ( #22605, #21629, #13653, #46466 ) ) ;
#51819 = DIRECTION ( 'NONE',  ( -0.8124868780056742068, 0.000000000000000000, -0.5829794791144820021 ) ) ;
#51820 = EDGE_LOOP ( 'NONE', ( #46879, #31165, #30314, #28742 ) ) ;
#51821 = CARTESIAN_POINT ( 'NONE',  ( -25.55153130240594450, -175.3837268820161057, 122.8793122007210741 ) ) ;
#51822 = DIRECTION ( 'NONE',  ( 0.8455960035018311727, 0.000000000000000000, -0.5338233779647826305 ) ) ;
#51824 = FACE_OUTER_BOUND ( 'NONE', #21685, .T. ) ;
#51823 = CARTESIAN_POINT ( 'NONE',  ( -48.47912675150885065, -175.3837268820161057, 6.938893903907228378E-15 ) ) ;
#51825 = ORIENTED_EDGE ( 'NONE', *, *, #31719, .T. ) ;
#51826 = EDGE_CURVE ( 'NONE', #10561, #39220, #29255, .T. ) ;
#51827 = CARTESIAN_POINT ( 'NONE',  ( -330.4913330509368166, -123.5000000000000284, 0.000000000000000000 ) ) ;
#51828 = CIRCLE ( 'NONE', #10663, 125.0000000000000000 ) ;
#51829 = DIRECTION ( 'NONE',  ( 0.9027978299657477557, 0.000000000000000000, -0.4300652022765115712 ) ) ;
#51830 = CIRCLE ( 'NONE', #30023, 125.0000000000000000 ) ;
#51831 = PLANE ( 'NONE',  #48533 ) ;
#51832 = ORIENTED_EDGE ( 'NONE', *, *, #25336, .T. ) ;
#51833 = CARTESIAN_POINT ( 'NONE',  ( -106.4764934152196645, -193.5000000000000000, 110.7307791902283043 ) ) ;
#51834 = DIRECTION ( 'NONE',  ( 0.000000000000000000, 1.000000000000000000, -3.491481338843133355E-15 ) ) ;
#51835 = VECTOR ( 'NONE', #4881, 1000.000000000000114 ) ;
#51836 = DIRECTION ( 'NONE',  ( -0.05924062789372142729, 0.000000000000000000, 0.9982437317643209074 ) ) ;
#51837 = ORIENTED_EDGE ( 'NONE', *, *, #15114, .F. ) ;
#51838 = EDGE_CURVE ( 'NONE', #44335, #27341, #9883, .T. ) ;
#51839 = DIRECTION ( 'NONE',  ( 0.000000000000000000, 0.000000000000000000, 1.000000000000000000 ) ) ;
#51840 = FACE_OUTER_BOUND ( 'NONE', #4482, .T. ) ;
#51841 = ORIENTED_EDGE ( 'NONE', *, *, #13221, .F. ) ;
#51842 = LINE ( 'NONE', #51079, #7311 ) ;
#51843 = ORIENTED_EDGE ( 'NONE', *, *, #50259, .F. ) ;
#51844 = VECTOR ( 'NONE', #42413, 1000.000000000000000 ) ;
#51845 = ADVANCED_FACE ( 'NONE', ( #9035 ), #29506, .T. ) ;
#51846 = CARTESIAN_POINT ( 'NONE',  ( -157.5429198988176438, -189.7472609257535510, 61.07445476073480961 ) ) ;
#51847 = VECTOR ( 'NONE', #39945, 1000.000000000000114 ) ;
#51848 = CARTESIAN_POINT ( 'NONE',  ( -55.65514169787639531, -193.5000000000000000, -123.7921848946937473 ) ) ;
#51849 = AXIS2_PLACEMENT_3D ( 'NONE', #49569, #34038, #6712 ) ;
#51850 = B_SPLINE_CURVE_WITH_KNOTS ( 'NONE', 3,
 ( #5020, #21037, #37056, #33889, #9727, #25758, #41792, #38609, #50710, #34155, #30714, #42036, #9997, #46010, #27030, #50976, #19165, #22596, #39116, #42552, #6573, #7076, #6303, #26516, #3128, #26012, #47026, #18396, #6049, #49935, #50207, #2365, #30463, #22067 ),
 .UNSPECIFIED., .F., .F.,
 ( 4, 2, 2, 2, 2, 2, 2, 2, 2, 2, 2, 2, 2, 2, 2, 2, 4 ),
 ( 0.01842143033997594576, 0.01929937734498573393, 0.02017732434999552210, 0.02105527135500531027, 0.02193321836001509845, 0.02281116536502488315, 0.02368911237003466785, 0.02456705937504445950, 0.02544500638005424420, 0.02632295338506403237, 0.02720090039007382055, 0.02807884739508360872, 0.02895679440009339689, 0.02983474140510318506, 0.03071268841011297324, 0.03159063541512276141, 0.03246858242013254958 ),
 .UNSPECIFIED. ) ;
#51851 = DIRECTION ( 'NONE',  ( 0.000000000000000000, 6.938893903907229364E-16, 1.000000000000000000 ) ) ;
#51852 = DIRECTION ( 'NONE',  ( -0.000000000000000000, 1.000000000000000000, -0.000000000000000000 ) ) ;
#51853 = CARTESIAN_POINT ( 'NONE',  ( -330.0000000000000568, -123.5000000000000284, 0.000000000000000000 ) ) ;
#51854 = CIRCLE ( 'NONE', #35761, 60.00000000000000000 ) ;
#51856 = AXIS2_PLACEMENT_3D ( 'NONE', #6120, #10559, #14257 ) ;
#51855 = DIRECTION ( 'NONE',  ( -1.000000000000000000, 0.000000000000000000, 0.000000000000000000 ) ) ;
#51857 = CARTESIAN_POINT ( 'NONE',  ( -339.1964088526558498, -67.57827586672178199, -21.74306257088745298 ) ) ;
#51858 = EDGE_CURVE ( 'NONE', #43700, #39182, #47662, .T. ) ;
#51859 = LINE ( 'NONE', #31339, #34774 ) ;
#51861 = ORIENTED_EDGE ( 'NONE', *, *, #28856, .T. ) ;
#51860 = CARTESIAN_POINT ( 'NONE',  ( 75.02564229359539638, -175.3837268820161057, -19.27620354518635182 ) ) ;
#51862 = ORIENTED_EDGE ( 'NONE', *, *, #26783, .T. ) ;
#51863 = CARTESIAN_POINT ( 'NONE',  ( 0.000000000000000000, -68.33404168156025094, 20.92168833550889673 ) ) ;
#51864 = DIRECTION ( 'NONE',  ( 0.4566292373937140270, 0.000000000000000000, -0.8896570909947467687 ) ) ;
#51865 = ORIENTED_EDGE ( 'NONE', *, *, #50436, .F. ) ;
#51866 = VECTOR ( 'NONE', #40545, 1000.000000000000000 ) ;
#51867 = CIRCLE ( 'NONE', #6554, 125.0000000000000000 ) ;
#51868 = ORIENTED_EDGE ( 'NONE', *, *, #447, .T. ) ;
#51869 = VERTEX_POINT ( 'NONE', #9808 ) ;
#51870 = DIRECTION ( 'NONE',  ( -0.000000000000000000, 1.000000000000000000, -0.000000000000000000 ) ) ;
#51871 = DIRECTION ( 'NONE',  ( 0.000000000000000000, 1.000000000000000000, -0.000000000000000000 ) ) ;
#51872 = AXIS2_PLACEMENT_3D ( 'NONE', #7948, #31615, #40520 ) ;
#51873 = CARTESIAN_POINT ( 'NONE',  ( -165.7578939544008847, -177.1207230881787780, -43.25148278810626579 ) ) ;
#51874 = CARTESIAN_POINT ( 'NONE',  ( -332.3517673607765914, -141.9604555052315220, 56.09938080879057765 ) ) ;
#51875 = ORIENTED_EDGE ( 'NONE', *, *, #20498, .F. ) ;
#51876 = ORIENTED_EDGE ( 'NONE', *, *, #17462, .F. ) ;
#51877 = EDGE_LOOP ( 'NONE', ( #28491, #13105, #11087, #5589 ) ) ;
#51878 = CARTESIAN_POINT ( 'NONE',  ( 47.91692961953209107, -189.7472609257535510, -77.99872144864700374 ) ) ;
#51879 = CARTESIAN_POINT ( 'NONE',  ( 72.14504940832448199, -189.7472609257535510, -32.78426643622660919 ) ) ;
#51880 = AXIS2_PLACEMENT_3D ( 'NONE', #18884, #3117, #39107 ) ;
#51881 = CARTESIAN_POINT ( 'NONE',  ( 36.84288420123323249, -193.5000000000000000, 91.35181687837503262 ) ) ;
#51882 = PLANE ( 'NONE',  #9427 ) ;
#51883 = DIRECTION ( 'NONE',  ( 0.000000000000000000, 0.000000000000000000, 1.000000000000000000 ) ) ;
#51884 = VERTEX_POINT ( 'NONE', #48976 ) ;
#51885 = CARTESIAN_POINT ( 'NONE',  ( -70.58093260035836636, -175.3837268820161057, 122.0143860769388766 ) ) ;
#51886 = EDGE_CURVE ( 'NONE', #38808, #779, #12953, .T. ) ;
#51887 = EDGE_CURVE ( 'NONE', #5285, #24408, #29763, .T. ) ;
#51888 = CARTESIAN_POINT ( 'NONE',  ( 62.59443091842027940, -193.5000000000000000, -57.33816169485140790 ) ) ;
#51889 = DIRECTION ( 'NONE',  ( -0.000000000000000000, 1.000000000000000000, -0.000000000000000000 ) ) ;
#51890 = AXIS2_PLACEMENT_3D ( 'NONE', #25249, #9227, #9481 ) ;
#51891 = EDGE_CURVE ( 'NONE', #39380, #4089, #49240, .T. ) ;
#51892 = VERTEX_POINT ( 'NONE', #25564 ) ;
#51893 = VERTEX_POINT ( 'NONE', #13488 ) ;
#51894 = EDGE_LOOP ( 'NONE', ( #11191, #21500, #34461, #48789 ) ) ;
#51895 = FACE_OUTER_BOUND ( 'NONE', #43494, .T. ) ;
#51896 = CARTESIAN_POINT ( 'NONE',  ( -4.176930889631405464, -189.7472609257535510, 116.8859077982279615 ) ) ;
#51897 = VERTEX_POINT ( 'NONE', #5096 ) ;
#51898 = DIRECTION ( 'NONE',  ( 0.000000000000000000, 2.914335439641035919E-13, -1.000000000000000000 ) ) ;
#51899 = CARTESIAN_POINT ( 'NONE',  ( 37.99238433767461487, -193.5000000000000000, -90.26448786734027863 ) ) ;
#51900 = DIRECTION ( 'NONE',  ( 0.000000000000000000, -0.1205366802553164696, 0.9927088740980548609 ) ) ;
#51901 = ORIENTED_EDGE ( 'NONE', *, *, #31033, .T. ) ;
#51902 = EDGE_CURVE ( 'NONE', #12238, #41636, #40136, .T. ) ;
#51903 = CARTESIAN_POINT ( 'NONE',  ( -48.47912675150885065, -175.3837268820161057, 6.938893903907228378E-15 ) ) ;
#51904 = EDGE_CURVE ( 'NONE', #34663, #40286, #1125, .T. ) ;
#51905 = EDGE_CURVE ( 'NONE', #38530, #50508, #9294, .T. ) ;
#51906 = EDGE_LOOP ( 'NONE', ( #22570, #21049, #39595, #28588 ) ) ;
#51907 = DIRECTION ( 'NONE',  ( -0.000000000000000000, -0.4647231720437724478, -0.8854560256532078011 ) ) ;
#51908 = FACE_OUTER_BOUND ( 'NONE', #51877, .T. ) ;
#51909 = AXIS2_PLACEMENT_3D ( 'NONE', #47105, #18986, #10323 ) ;
#51910 = AXIS2_PLACEMENT_3D ( 'NONE', #13301, #13818, #21182 ) ;
#51911 = EDGE_CURVE ( 'NONE', #43506, #16176, #23350, .T. ) ;
#51912 = VECTOR ( 'NONE', #5017, 1000.000000000000000 ) ;
#51913 = EDGE_CURVE ( 'NONE', #39607, #18605, #24796, .T. ) ;
#51914 = DIRECTION ( 'NONE',  ( 0.000000000000000000, 0.000000000000000000, -1.000000000000000000 ) ) ;
#51915 = EDGE_LOOP ( 'NONE', ( #30364, #39659, #51933, #1581 ) ) ;
#51916 = CIRCLE ( 'NONE', #13296, 60.00000000000000000 ) ;
#51917 = DIRECTION ( 'NONE',  ( 0.000000000000000000, 0.000000000000000000, -1.000000000000000000 ) ) ;
#51918 = FACE_OUTER_BOUND ( 'NONE', #51191, .T. ) ;
#51919 = DIRECTION ( 'NONE',  ( 0.000000000000000000, 0.000000000000000000, 1.000000000000000000 ) ) ;
#51920 = FACE_OUTER_BOUND ( 'NONE', #51454, .T. ) ;
#51921 = ORIENTED_EDGE ( 'NONE', *, *, #6979, .F. ) ;
#51922 = DIRECTION ( 'NONE',  ( 0.000000000000000000, -0.000000000000000000, 1.000000000000000000 ) ) ;
#51923 = ORIENTED_EDGE ( 'NONE', *, *, #4657, .F. ) ;
#51924 = ORIENTED_EDGE ( 'NONE', *, *, #1467, .T. ) ;
#51925 = VECTOR ( 'NONE', #9991, 1000.000000000000000 ) ;
#51926 = PLANE ( 'NONE',  #33679 ) ;
#51928 = EDGE_LOOP ( 'NONE', ( #19350, #13720, #44009, #41920 ) ) ;
#51927 = DIRECTION ( 'NONE',  ( -0.000000000000000000, 1.000000000000000000, 0.000000000000000000 ) ) ;
#51929 = VERTEX_POINT ( 'NONE', #38436 ) ;
#51930 = CARTESIAN_POINT ( 'NONE',  ( 46.00000000000000000, 20.00000000000000000, 4.999999999999997335 ) ) ;
#51931 = VECTOR ( 'NONE', #6251, 1000.000000000000000 ) ;
#51932 = LINE ( 'NONE', #15920, #36921 ) ;
#51933 = ORIENTED_EDGE ( 'NONE', *, *, #44164, .T. ) ;
#51934 = DIRECTION ( 'NONE',  ( -0.000000000000000000, 1.000000000000000000, -0.000000000000000000 ) ) ;
#51935 = PLANE ( 'NONE',  #6907 ) ;
#51936 = EDGE_LOOP ( 'NONE', ( #26230, #37468, #18731, #47291 ) ) ;
#51937 = DIRECTION ( 'NONE',  ( 0.000000000000000000, 0.000000000000000000, -1.000000000000000000 ) ) ;
#51938 = DIRECTION ( 'NONE',  ( -0.000000000000000000, 0.000000000000000000, 1.000000000000000000 ) ) ;
#51939 = DIRECTION ( 'NONE',  ( 5.399917434947259359E-17, 1.000000000000000000, -0.000000000000000000 ) ) ;
#51940 = DIRECTION ( 'NONE',  ( 0.6300878435817038881, 0.000000000000000000, 0.7765238627180482966 ) ) ;
#51941 = EDGE_LOOP ( 'NONE', ( #791, #35078, #1592, #11927 ) ) ;
#51942 = ORIENTED_EDGE ( 'NONE', *, *, #50440, .T. ) ;
#51943 = ORIENTED_EDGE ( 'NONE', *, *, #51838, .F. ) ;
#51944 = CARTESIAN_POINT ( 'NONE',  ( -336.3521761649653854, -183.2372378732723632, -5.609136410542876483 ) ) ;
#51945 =( GEOMETRIC_REPRESENTATION_CONTEXT ( 3 ) GLOBAL_UNCERTAINTY_ASSIGNED_CONTEXT ( ( #38989 ) ) GLOBAL_UNIT_ASSIGNED_CONTEXT ( ( #28353, #33350, #44915 ) ) REPRESENTATION_CONTEXT ( 'NONE', 'WORKASPACE' ) );
#51946 = CARTESIAN_POINT ( 'NONE',  ( 4.298610786024391605E-15, 0.000000000000000000, -41.00000000000000711 ) ) ;
#51947 = AXIS2_PLACEMENT_3D ( 'NONE', #41087, #25568, #1672 ) ;
#51948 = VECTOR ( 'NONE', #33320, 1000.000000000000000 ) ;
#51949 = FACE_OUTER_BOUND ( 'NONE', #49407, .T. ) ;
#51950 = PLANE ( 'NONE',  #9389 ) ;
#51951 = CARTESIAN_POINT ( 'NONE',  ( 48.06131630543706024, -189.7472609257535510, -79.40367028273054473 ) ) ;
#51952 = ORIENTED_EDGE ( 'NONE', *, *, #20788, .T. ) ;
#51953 = VECTOR ( 'NONE', #34410, 1000.000000000000000 ) ;
#51954 = EDGE_CURVE ( 'NONE', #1774, #11977, #42640, .T. ) ;
#51955 = ADVANCED_FACE ( 'NONE', ( #46590 ), #34485, .T. ) ;
#51956 = EDGE_CURVE ( 'NONE', #4337, #43203, #2174, .T. ) ;
#51957 = DIRECTION ( 'NONE',  ( 5.399917434947259359E-17, 1.000000000000000000, -0.000000000000000000 ) ) ;
#51958 = ORIENTED_EDGE ( 'NONE', *, *, #2875, .T. ) ;
#51960 = ORIENTED_EDGE ( 'NONE', *, *, #14983, .T. ) ;
#51959 = LINE ( 'NONE', #48254, #15559 ) ;
#51961 = VECTOR ( 'NONE', #44876, 999.9999999999998863 ) ;
#51962 = EDGE_LOOP ( 'NONE', ( #7029, #39836, #12728, #8356 ) ) ;
#51963 = CARTESIAN_POINT ( 'NONE',  ( -48.64924157374596092, -189.7472609257535510, 123.9998842437354227 ) ) ;
#51964 = ADVANCED_FACE ( 'NONE', ( #46856 ), #34239, .F. ) ;
#51965 = CARTESIAN_POINT ( 'NONE',  ( -48.47912675150885065, -189.7472609257535510, 6.938893903907228378E-15 ) ) ;
#51966 = DIRECTION ( 'NONE',  ( -0.000000000000000000, -1.000000000000000000, 0.000000000000000000 ) ) ;
#51967 = FACE_OUTER_BOUND ( 'NONE', #33471, .T. ) ;
#51968 = ORIENTED_EDGE ( 'NONE', *, *, #49111, .F. ) ;
#51969 = ADVANCED_FACE ( 'NONE', ( #50534 ), #15058, .F. ) ;
#51970 = LINE ( 'NONE', #44334, #34261 ) ;
#51971 = EDGE_LOOP ( 'NONE', ( #18100, #27681, #48463, #4863 ) ) ;
#51972 = EDGE_CURVE ( 'NONE', #28974, #39629, #43491, .T. ) ;
#51973 = VECTOR ( 'NONE', #20139, 1000.000000000000000 ) ;
#51974 = ORIENTED_EDGE ( 'NONE', *, *, #46544, .T. ) ;
#51975 = LINE ( 'NONE', #19375, #49733 ) ;
#51976 = EDGE_CURVE ( 'NONE', #16698, #25045, #38163, .T. ) ;
#51977 = FACE_OUTER_BOUND ( 'NONE', #21687, .T. ) ;
#51978 = CARTESIAN_POINT ( 'NONE',  ( -48.47912675150885065, -183.6283474603465606, 6.938893903907228378E-15 ) ) ;
#51979 = CARTESIAN_POINT ( 'NONE',  ( 141.7825277784304205, -213.5000000000000000, -9.999999999999987566 ) ) ;
#51980 = ADVANCED_FACE ( 'NONE', ( #43145 ), #35259, .T. ) ;
#51981 = DIRECTION ( 'NONE',  ( -0.8124868780056742068, 0.000000000000000000, -0.5829794791144820021 ) ) ;
#51982 = CARTESIAN_POINT ( 'NONE',  ( -332.3517673607765914, -123.5000000000000284, 0.000000000000000000 ) ) ;
#51983 = ORIENTED_EDGE ( 'NONE', *, *, #6272, .T. ) ;
#51984 = CARTESIAN_POINT ( 'NONE',  ( 64.44365795514079309, -189.7472609257535510, -53.60452120946192878 ) ) ;
#51985 = PLANE ( 'NONE',  #38302 ) ;
#51986 = FACE_BOUND ( 'NONE', #16748, .T. ) ;
#51987 = ORIENTED_EDGE ( 'NONE', *, *, #10908, .T. ) ;
#51988 = AXIS2_PLACEMENT_3D ( 'NONE', #14184, #25992, #30438 ) ;
#51989 = DIRECTION ( 'NONE',  ( -0.9929810960135169173, 0.000000000000000000, -0.1182731709213660498 ) ) ;
#51990 = VECTOR ( 'NONE', #43775, 1000.000000000000000 ) ;
#51991 = CARTESIAN_POINT ( 'NONE',  ( -336.3521761649654422, -123.5000000000000284, 0.000000000000000000 ) ) ;
#51992 = VERTEX_POINT ( 'NONE', #6652 ) ;
#51993 = CARTESIAN_POINT ( 'NONE',  ( 60.90550954139437323, -189.7472609257535510, 60.49794494914088006 ) ) ;
#51994 = VERTEX_POINT ( 'NONE', #30288 ) ;
#51995 = ADVANCED_FACE ( 'NONE', ( #46335 ), #26605, .F. ) ;
#51996 = DIRECTION ( 'NONE',  ( 0.000000000000000000, 0.000000000000000000, 1.000000000000000000 ) ) ;
#51997 = FACE_BOUND ( 'NONE', #8635, .T. ) ;
#51998 = DIRECTION ( 'NONE',  ( -0.000000000000000000, 1.000000000000000000, -0.000000000000000000 ) ) ;
#51999 = LINE ( 'NONE', #44611, #24384 ) ;
#52000 = ORIENTED_EDGE ( 'NONE', *, *, #43212, .F. ) ;
#52001 = AXIS2_PLACEMENT_3D ( 'NONE', #49459, #51900, #3786 ) ;
#52002 = ORIENTED_EDGE ( 'NONE', *, *, #12101, .F. ) ;
#52003 = EDGE_CURVE ( 'NONE', #25203, #903, #35009, .T. ) ;
#52004 = DIRECTION ( 'NONE',  ( 0.000000000000000000, 0.000000000000000000, 1.000000000000000000 ) ) ;
#52005 = ORIENTED_EDGE ( 'NONE', *, *, #49702, .T. ) ;
#52006 = DIRECTION ( 'NONE',  ( -0.7175072570443299380, 0.000000000000000000, -0.6965510290629983725 ) ) ;
#52007 = CARTESIAN_POINT ( 'NONE',  ( -336.3521761649654422, -83.15397741537739762, 43.07972642080338233 ) ) ;
#52008 = EDGE_CURVE ( 'NONE', #21927, #40700, #26715, .T. ) ;
#52009 = EDGE_CURVE ( 'NONE', #5680, #42978, #42369, .T. ) ;
#52010 = EDGE_CURVE ( 'NONE', #13886, #39193, #2443, .T. ) ;
#52011 = EDGE_CURVE ( 'NONE', #9854, #38994, #4897, .T. ) ;
#52012 = EDGE_CURVE ( 'NONE', #13290, #47261, #7151, .T. ) ;
#52013 = CARTESIAN_POINT ( 'NONE',  ( -56.71246971489870958, -175.3837268820161057, -124.7285535218267540 ) ) ;
#52014 = CARTESIAN_POINT ( 'NONE',  ( -330.4913330509368166, -68.15673923803900891, 20.45418021416622878 ) ) ;
#52015 = ORIENTED_EDGE ( 'NONE', *, *, #16405, .T. ) ;
#52018 = ORIENTED_EDGE ( 'NONE', *, *, #14962, .F. ) ;
#52017 = CARTESIAN_POINT ( 'NONE',  ( -156.9880281022168447, -175.3837268820161057, -60.01515274640934905 ) ) ;
#52016 = CARTESIAN_POINT ( 'NONE',  ( -0.3054481938615516423, -193.5000000000000000, 115.3442529744090450 ) ) ;
#52019 = ORIENTED_EDGE ( 'NONE', *, *, #2875, .F. ) ;
#52020 = AXIS2_PLACEMENT_3D ( 'NONE', #44606, #4660, #20688 ) ;
#52021 = ADVANCED_FACE ( 'NONE', ( #3220 ), #19250, .F. ) ;
#52022 = DIRECTION ( 'NONE',  ( -0.000000000000000000, 1.000000000000000000, 0.000000000000000000 ) ) ;
#52023 = ORIENTED_EDGE ( 'NONE', *, *, #2418, .F. ) ;
#52024 = CARTESIAN_POINT ( 'NONE',  ( -49.29161362951452929, -175.3837268820161057, -0.5829794791144748967 ) ) ;
#52025 = EDGE_LOOP ( 'NONE', ( #39500, #24118, #29609, #14397 ) ) ;
#52026 = FACE_OUTER_BOUND ( 'NONE', #1548, .T. ) ;
#52027 = VERTEX_POINT ( 'NONE', #51309 ) ;
#52028 = ADVANCED_FACE ( 'NONE', ( #20013 ), #51831, .T. ) ;
#52030 = DIRECTION ( 'NONE',  ( -1.000000000000000000, 0.000000000000000000, -0.000000000000000000 ) ) ;
#52029 = FACE_OUTER_BOUND ( 'NONE', #45931, .T. ) ;
#52031 = ORIENTED_EDGE ( 'NONE', *, *, #26130, .F. ) ;
#52032 = ADVANCED_FACE ( 'NONE', ( #36041 ), #43668, .F. ) ;
#52033 = ORIENTED_EDGE ( 'NONE', *, *, #11166, .T. ) ;
#52034 = DIRECTION ( 'NONE',  ( -1.000000000000000000, 0.000000000000000000, 0.000000000000000000 ) ) ;
#52035 = PLANE ( 'NONE',  #30720 ) ;
#52036 = EDGE_CURVE ( 'NONE', #50002, #45115, #39283, .T. ) ;
#52037 = CARTESIAN_POINT ( 'NONE',  ( 76.01188277843579044, -193.5000000000000000, 11.26891947860284482 ) ) ;
#52038 = LINE ( 'NONE', #8387, #8916 ) ;
#52039 = CARTESIAN_POINT ( 'NONE',  ( -238.7407812814481076, -213.5000000000000000, 10.00000000000000178 ) ) ;
#52040 = CARTESIAN_POINT ( 'NONE',  ( -332.3517673607765914, -88.64083255475578937, 47.62880233550460218 ) ) ;
#52041 = NEXT_ASSEMBLY_USAGE_OCCURRENCE ( 'NAUO1', ' ', ' ', #47283, #19619, $ ) ;
#52042 = NEXT_ASSEMBLY_USAGE_OCCURRENCE ( 'NAUO2', ' ', ' ', #47283, #34451, $ ) ;
#52043 = NEXT_ASSEMBLY_USAGE_OCCURRENCE ( 'NAUO3', ' ', ' ', #47283, #38299, $ ) ;
#52044 = NEXT_ASSEMBLY_USAGE_OCCURRENCE ( 'NAUO4', ' ', ' ', #47283, #1043, $ ) ;
#52045 = NEXT_ASSEMBLY_USAGE_OCCURRENCE ( 'NAUO5', ' ', ' ', #47283, #8752, $ ) ;
#52046 = NEXT_ASSEMBLY_USAGE_OCCURRENCE ( 'NAUO6', ' ', ' ', #47283, #11949, $ ) ;
#52047 = NEXT_ASSEMBLY_USAGE_OCCURRENCE ( 'NAUO7', ' ', ' ', #47283, #36651, $ ) ;
#52048 = NEXT_ASSEMBLY_USAGE_OCCURRENCE ( 'NAUO8', ' ', ' ', #47283, #25740, $ ) ;
#52049 = NEXT_ASSEMBLY_USAGE_OCCURRENCE ( 'NAUO9', ' ', ' ', #47283, #44373, $ ) ;
#52050 = NEXT_ASSEMBLY_USAGE_OCCURRENCE ( 'NAUO10', ' ', ' ', #47283, #36651, $ ) ;
#52051 = NEXT_ASSEMBLY_USAGE_OCCURRENCE ( 'NAUO11', ' ', ' ', #47283, #36651, $ ) ;
ENDSEC;
END-ISO-10303-21;
